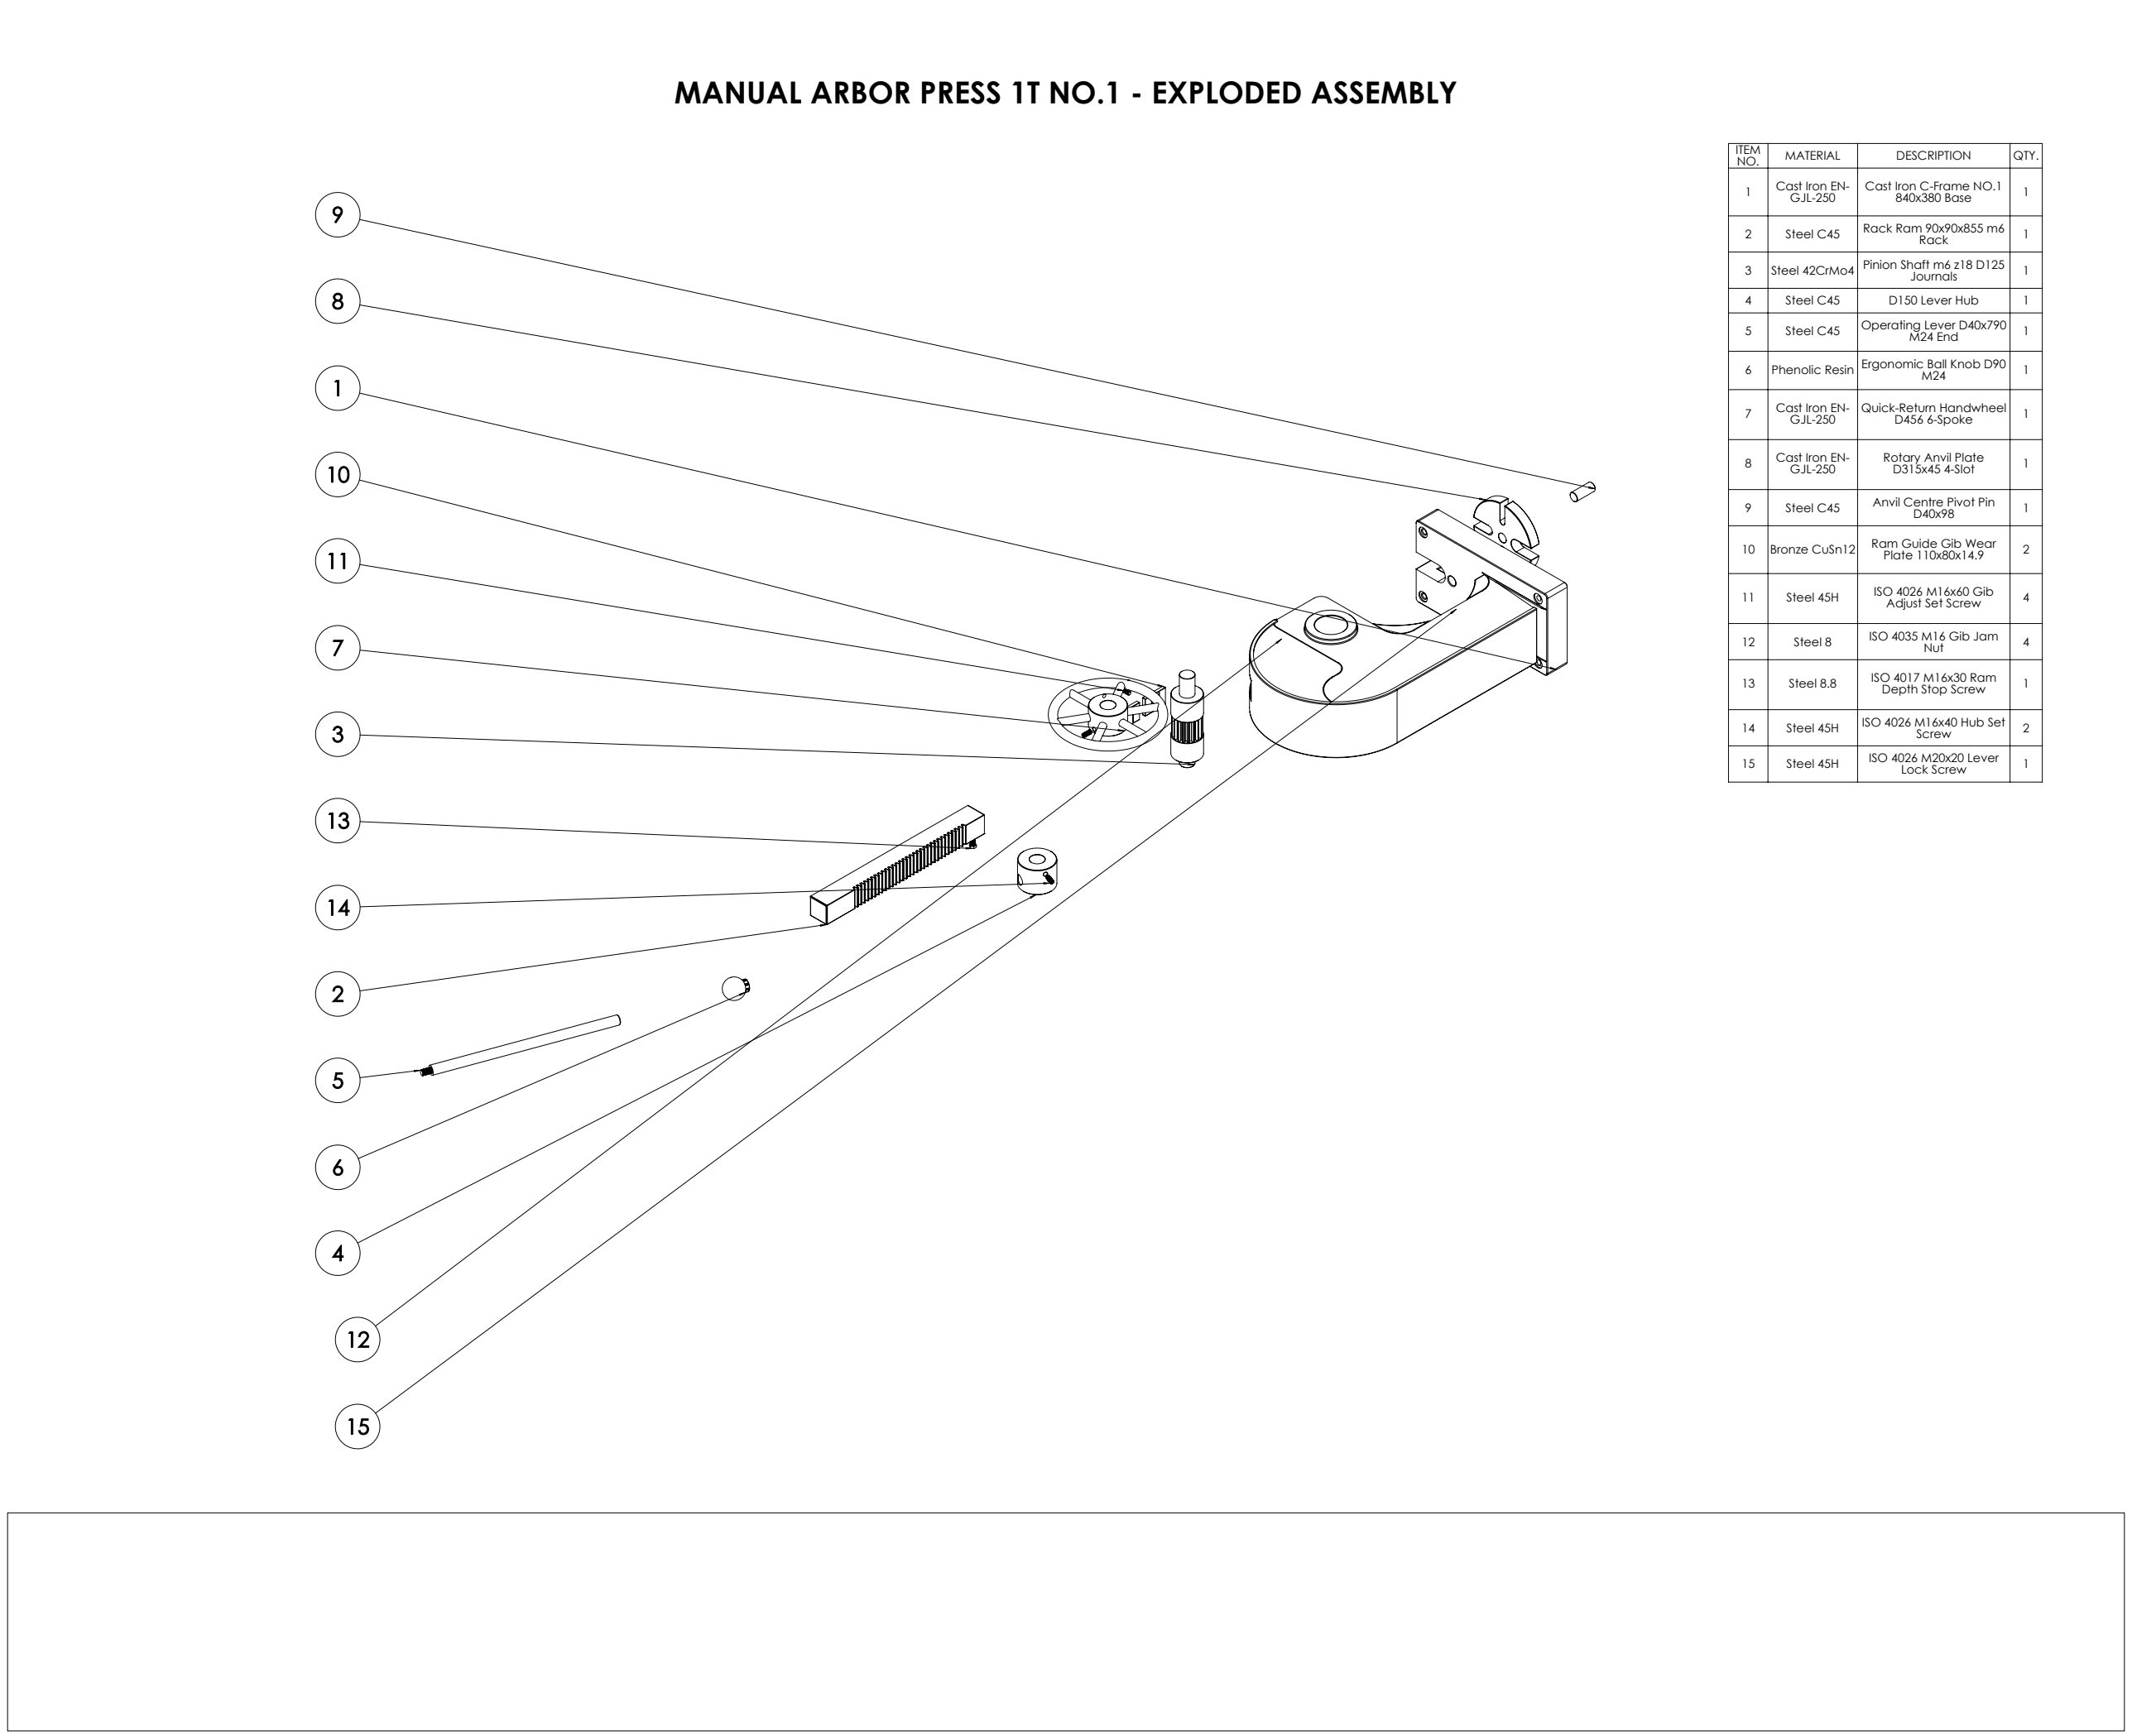
ISO-10303-21;
HEADER;
/* Generated by software containing ST-Developer
 * from STEP Tools, Inc. (www.steptools.com) 
 */

FILE_DESCRIPTION(
/* description */ (''),
/* implementation_level */ '2;1');

FILE_NAME(
/* name */ 'MAS-305',
/* time_stamp */ '2026-10-19T23:58:09-07:00',
/* author */ (''),
/* organization */ (''),
/* preprocessor_version */ 'ST-DEVELOPER v20.2',
/* originating_system */ 'Autodesk Translation Framework v15.15.0.0',
/* authorisation */ '');

FILE_SCHEMA (('AP203_CONFIGURATION_CONTROLLED_3D_DESIGN_OF_MECHANICAL_PARTS_AND_ASSEMBLIES_MIM_LF { 1 0 10303 203 3 1 4 }',
'AUTOMOTIVE_DESIGN { 1 0 10303 214 3 1 1 }','INTEGRATED_CNC_SCHEMA','MODEL_BASED_INTEGRATED_MANUFACTURING_SCHEMA',
'PROCESS_PLANNING_SCHEMA','AP242_MANAGED_MODEL_BASED_3D_ENGINEERING_MIM_LF { 1 0 10303 442 3 1 4 }'));
ENDSEC;

DATA;
#10=MECHANICAL_DESIGN_GEOMETRIC_PRESENTATION_REPRESENTATION('',(#407,#408,
#409,#410,#411,#412,#413,#414,#415,#416,#417,#418,#419,#420,#421,#422,#423,
#424,#425,#426,#427,#428,#429,#430,#431,#432,#433,#434,#435,#436,#437,#438,
#439,#440,#441,#442,#443,#444,#445,#446,#447,#448,#449,#450,#451,#452,#453,
#454,#455,#456,#457,#458,#459,#460,#461,#462,#463,#464,#465,#466),#70757);
#11=ITEM_DEFINED_TRANSFORMATION($,$,#27054,#28962);
#12=ITEM_DEFINED_TRANSFORMATION($,$,#27231,#28963);
#13=ITEM_DEFINED_TRANSFORMATION($,$,#27283,#28964);
#14=ITEM_DEFINED_TRANSFORMATION($,$,#27389,#28965);
#15=ITEM_DEFINED_TRANSFORMATION($,$,#27510,#28966);
#16=ITEM_DEFINED_TRANSFORMATION($,$,#27399,#28967);
#17=ITEM_DEFINED_TRANSFORMATION($,$,#27547,#28968);
#18=ITEM_DEFINED_TRANSFORMATION($,$,#27669,#28969);
#19=ITEM_DEFINED_TRANSFORMATION($,$,#27689,#28970);
#20=ITEM_DEFINED_TRANSFORMATION($,$,#27432,#28971);
#21=ITEM_DEFINED_TRANSFORMATION($,$,#27510,#28972);
#22=ITEM_DEFINED_TRANSFORMATION($,$,#27547,#28973);
#23=ITEM_DEFINED_TRANSFORMATION($,$,#27547,#28974);
#24=ITEM_DEFINED_TRANSFORMATION($,$,#27547,#28975);
#25=ITEM_DEFINED_TRANSFORMATION($,$,#27669,#28976);
#26=ITEM_DEFINED_TRANSFORMATION($,$,#27669,#28977);
#27=ITEM_DEFINED_TRANSFORMATION($,$,#27669,#28978);
#28=ITEM_DEFINED_TRANSFORMATION($,$,#27689,#28979);
#29=ITEM_DEFINED_TRANSFORMATION($,$,#27791,#28980);
#30=ITEM_DEFINED_TRANSFORMATION($,$,#27818,#28981);
#31=ITEM_DEFINED_TRANSFORMATION($,$,#28305,#28982);
#32=ITEM_DEFINED_TRANSFORMATION($,$,#28396,#28983);
#33=ITEM_DEFINED_TRANSFORMATION($,$,#28892,#28984);
#34=(
REPRESENTATION_RELATIONSHIP($,$,#70818,#70817)
REPRESENTATION_RELATIONSHIP_WITH_TRANSFORMATION(#11)
SHAPE_REPRESENTATION_RELATIONSHIP()
);
#35=(
REPRESENTATION_RELATIONSHIP($,$,#70819,#70817)
REPRESENTATION_RELATIONSHIP_WITH_TRANSFORMATION(#12)
SHAPE_REPRESENTATION_RELATIONSHIP()
);
#36=(
REPRESENTATION_RELATIONSHIP($,$,#70820,#70817)
REPRESENTATION_RELATIONSHIP_WITH_TRANSFORMATION(#13)
SHAPE_REPRESENTATION_RELATIONSHIP()
);
#37=(
REPRESENTATION_RELATIONSHIP($,$,#70821,#70817)
REPRESENTATION_RELATIONSHIP_WITH_TRANSFORMATION(#14)
SHAPE_REPRESENTATION_RELATIONSHIP()
);
#38=(
REPRESENTATION_RELATIONSHIP($,$,#70824,#70817)
REPRESENTATION_RELATIONSHIP_WITH_TRANSFORMATION(#15)
SHAPE_REPRESENTATION_RELATIONSHIP()
);
#39=(
REPRESENTATION_RELATIONSHIP($,$,#70822,#70817)
REPRESENTATION_RELATIONSHIP_WITH_TRANSFORMATION(#16)
SHAPE_REPRESENTATION_RELATIONSHIP()
);
#40=(
REPRESENTATION_RELATIONSHIP($,$,#70825,#70817)
REPRESENTATION_RELATIONSHIP_WITH_TRANSFORMATION(#17)
SHAPE_REPRESENTATION_RELATIONSHIP()
);
#41=(
REPRESENTATION_RELATIONSHIP($,$,#70826,#70817)
REPRESENTATION_RELATIONSHIP_WITH_TRANSFORMATION(#18)
SHAPE_REPRESENTATION_RELATIONSHIP()
);
#42=(
REPRESENTATION_RELATIONSHIP($,$,#70827,#70817)
REPRESENTATION_RELATIONSHIP_WITH_TRANSFORMATION(#19)
SHAPE_REPRESENTATION_RELATIONSHIP()
);
#43=(
REPRESENTATION_RELATIONSHIP($,$,#70823,#70817)
REPRESENTATION_RELATIONSHIP_WITH_TRANSFORMATION(#20)
SHAPE_REPRESENTATION_RELATIONSHIP()
);
#44=(
REPRESENTATION_RELATIONSHIP($,$,#70824,#70817)
REPRESENTATION_RELATIONSHIP_WITH_TRANSFORMATION(#21)
SHAPE_REPRESENTATION_RELATIONSHIP()
);
#45=(
REPRESENTATION_RELATIONSHIP($,$,#70825,#70817)
REPRESENTATION_RELATIONSHIP_WITH_TRANSFORMATION(#22)
SHAPE_REPRESENTATION_RELATIONSHIP()
);
#46=(
REPRESENTATION_RELATIONSHIP($,$,#70825,#70817)
REPRESENTATION_RELATIONSHIP_WITH_TRANSFORMATION(#23)
SHAPE_REPRESENTATION_RELATIONSHIP()
);
#47=(
REPRESENTATION_RELATIONSHIP($,$,#70825,#70817)
REPRESENTATION_RELATIONSHIP_WITH_TRANSFORMATION(#24)
SHAPE_REPRESENTATION_RELATIONSHIP()
);
#48=(
REPRESENTATION_RELATIONSHIP($,$,#70826,#70817)
REPRESENTATION_RELATIONSHIP_WITH_TRANSFORMATION(#25)
SHAPE_REPRESENTATION_RELATIONSHIP()
);
#49=(
REPRESENTATION_RELATIONSHIP($,$,#70826,#70817)
REPRESENTATION_RELATIONSHIP_WITH_TRANSFORMATION(#26)
SHAPE_REPRESENTATION_RELATIONSHIP()
);
#50=(
REPRESENTATION_RELATIONSHIP($,$,#70826,#70817)
REPRESENTATION_RELATIONSHIP_WITH_TRANSFORMATION(#27)
SHAPE_REPRESENTATION_RELATIONSHIP()
);
#51=(
REPRESENTATION_RELATIONSHIP($,$,#70827,#70817)
REPRESENTATION_RELATIONSHIP_WITH_TRANSFORMATION(#28)
SHAPE_REPRESENTATION_RELATIONSHIP()
);
#52=(
REPRESENTATION_RELATIONSHIP($,$,#70828,#70817)
REPRESENTATION_RELATIONSHIP_WITH_TRANSFORMATION(#29)
SHAPE_REPRESENTATION_RELATIONSHIP()
);
#53=(
REPRESENTATION_RELATIONSHIP($,$,#70829,#70817)
REPRESENTATION_RELATIONSHIP_WITH_TRANSFORMATION(#30)
SHAPE_REPRESENTATION_RELATIONSHIP()
);
#54=(
REPRESENTATION_RELATIONSHIP($,$,#70830,#70817)
REPRESENTATION_RELATIONSHIP_WITH_TRANSFORMATION(#31)
SHAPE_REPRESENTATION_RELATIONSHIP()
);
#55=(
REPRESENTATION_RELATIONSHIP($,$,#70831,#70817)
REPRESENTATION_RELATIONSHIP_WITH_TRANSFORMATION(#32)
SHAPE_REPRESENTATION_RELATIONSHIP()
);
#56=(
REPRESENTATION_RELATIONSHIP($,$,#70832,#70817)
REPRESENTATION_RELATIONSHIP_WITH_TRANSFORMATION(#33)
SHAPE_REPRESENTATION_RELATIONSHIP()
);
#57=CONTEXT_DEPENDENT_SHAPE_REPRESENTATION(#34,#70794);
#58=CONTEXT_DEPENDENT_SHAPE_REPRESENTATION(#35,#70795);
#59=CONTEXT_DEPENDENT_SHAPE_REPRESENTATION(#36,#70796);
#60=CONTEXT_DEPENDENT_SHAPE_REPRESENTATION(#37,#70797);
#61=CONTEXT_DEPENDENT_SHAPE_REPRESENTATION(#38,#70798);
#62=CONTEXT_DEPENDENT_SHAPE_REPRESENTATION(#39,#70799);
#63=CONTEXT_DEPENDENT_SHAPE_REPRESENTATION(#40,#70800);
#64=CONTEXT_DEPENDENT_SHAPE_REPRESENTATION(#41,#70801);
#65=CONTEXT_DEPENDENT_SHAPE_REPRESENTATION(#42,#70802);
#66=CONTEXT_DEPENDENT_SHAPE_REPRESENTATION(#43,#70803);
#67=CONTEXT_DEPENDENT_SHAPE_REPRESENTATION(#44,#70804);
#68=CONTEXT_DEPENDENT_SHAPE_REPRESENTATION(#45,#70805);
#69=CONTEXT_DEPENDENT_SHAPE_REPRESENTATION(#46,#70806);
#70=CONTEXT_DEPENDENT_SHAPE_REPRESENTATION(#47,#70807);
#71=CONTEXT_DEPENDENT_SHAPE_REPRESENTATION(#48,#70808);
#72=CONTEXT_DEPENDENT_SHAPE_REPRESENTATION(#49,#70809);
#73=CONTEXT_DEPENDENT_SHAPE_REPRESENTATION(#50,#70810);
#74=CONTEXT_DEPENDENT_SHAPE_REPRESENTATION(#51,#70811);
#75=CONTEXT_DEPENDENT_SHAPE_REPRESENTATION(#52,#70812);
#76=CONTEXT_DEPENDENT_SHAPE_REPRESENTATION(#53,#70813);
#77=CONTEXT_DEPENDENT_SHAPE_REPRESENTATION(#54,#70814);
#78=CONTEXT_DEPENDENT_SHAPE_REPRESENTATION(#55,#70815);
#79=CONTEXT_DEPENDENT_SHAPE_REPRESENTATION(#56,#70816);
#80=NEXT_ASSEMBLY_USAGE_OCCURRENCE(
'03_Pinion_Shaft_m6_z18_D125_Journals:1',
'03_Pinion_Shaft_m6_z18_D125_Journals:1',
'03_Pinion_Shaft_m6_z18_D125_Journals:1',#70834,#70835,
'03_Pinion_Shaft_m6_z18_D125_Journals:1');
#81=NEXT_ASSEMBLY_USAGE_OCCURRENCE(
'05_Operating_Lever_D40x790_M24_End:1',
'05_Operating_Lever_D40x790_M24_End:1',
'05_Operating_Lever_D40x790_M24_End:1',#70834,#70836,
'05_Operating_Lever_D40x790_M24_End:1');
#82=NEXT_ASSEMBLY_USAGE_OCCURRENCE(
'08_Rotary_Anvil_Plate_D315x45_4-Slot:1',
'08_Rotary_Anvil_Plate_D315x45_4-Slot:1',
'08_Rotary_Anvil_Plate_D315x45_4-Slot:1',#70834,#70837,
'08_Rotary_Anvil_Plate_D315x45_4-Slot:1');
#83=NEXT_ASSEMBLY_USAGE_OCCURRENCE('09_Anvil_Centre_Pivot_Pin_D40x98:1',
'09_Anvil_Centre_Pivot_Pin_D40x98:1',
'09_Anvil_Centre_Pivot_Pin_D40x98:1',#70834,#70838,
'09_Anvil_Centre_Pivot_Pin_D40x98:1');
#84=NEXT_ASSEMBLY_USAGE_OCCURRENCE(
'10_Ram_Guide_Gib_Wear_Plate_110x80x14.9:1',
'10_Ram_Guide_Gib_Wear_Plate_110x80x14.9:1',
'10_Ram_Guide_Gib_Wear_Plate_110x80x14.9:1',#70834,#70841,
'10_Ram_Guide_Gib_Wear_Plate_110x80x14.9:1');
#85=NEXT_ASSEMBLY_USAGE_OCCURRENCE(
'07_Quick-Return_Handwheel_D456_6-Spoke:1',
'07_Quick-Return_Handwheel_D456_6-Spoke:1',
'07_Quick-Return_Handwheel_D456_6-Spoke:1',#70834,#70839,
'07_Quick-Return_Handwheel_D456_6-Spoke:1');
#86=NEXT_ASSEMBLY_USAGE_OCCURRENCE(
'11_ISO_4026_M16x60_Gib_Adjust_Set_Screw:1',
'11_ISO_4026_M16x60_Gib_Adjust_Set_Screw:1',
'11_ISO_4026_M16x60_Gib_Adjust_Set_Screw:1',#70834,#70842,
'11_ISO_4026_M16x60_Gib_Adjust_Set_Screw:1');
#87=NEXT_ASSEMBLY_USAGE_OCCURRENCE('12_ISO_4035_M16_Gib_Jam_Nut:1',
'12_ISO_4035_M16_Gib_Jam_Nut:1','12_ISO_4035_M16_Gib_Jam_Nut:1',#70834,
#70843,'12_ISO_4035_M16_Gib_Jam_Nut:1');
#88=NEXT_ASSEMBLY_USAGE_OCCURRENCE('14_ISO_4026_M16x40_Hub_Set_Screw:1',
'14_ISO_4026_M16x40_Hub_Set_Screw:1',
'14_ISO_4026_M16x40_Hub_Set_Screw:1',#70834,#70844,
'14_ISO_4026_M16x40_Hub_Set_Screw:1');
#89=NEXT_ASSEMBLY_USAGE_OCCURRENCE(
'15_ISO_4026_M20x20_Lever_Lock_Screw:1',
'15_ISO_4026_M20x20_Lever_Lock_Screw:1',
'15_ISO_4026_M20x20_Lever_Lock_Screw:1',#70834,#70840,
'15_ISO_4026_M20x20_Lever_Lock_Screw:1');
#90=NEXT_ASSEMBLY_USAGE_OCCURRENCE(
'10_Ram_Guide_Gib_Wear_Plate_110x80x14.9:2',
'10_Ram_Guide_Gib_Wear_Plate_110x80x14.9:2',
'10_Ram_Guide_Gib_Wear_Plate_110x80x14.9:2',#70834,#70841,
'10_Ram_Guide_Gib_Wear_Plate_110x80x14.9:2');
#91=NEXT_ASSEMBLY_USAGE_OCCURRENCE(
'11_ISO_4026_M16x60_Gib_Adjust_Set_Screw:2',
'11_ISO_4026_M16x60_Gib_Adjust_Set_Screw:2',
'11_ISO_4026_M16x60_Gib_Adjust_Set_Screw:2',#70834,#70842,
'11_ISO_4026_M16x60_Gib_Adjust_Set_Screw:2');
#92=NEXT_ASSEMBLY_USAGE_OCCURRENCE(
'11_ISO_4026_M16x60_Gib_Adjust_Set_Screw:3',
'11_ISO_4026_M16x60_Gib_Adjust_Set_Screw:3',
'11_ISO_4026_M16x60_Gib_Adjust_Set_Screw:3',#70834,#70842,
'11_ISO_4026_M16x60_Gib_Adjust_Set_Screw:3');
#93=NEXT_ASSEMBLY_USAGE_OCCURRENCE(
'11_ISO_4026_M16x60_Gib_Adjust_Set_Screw:4',
'11_ISO_4026_M16x60_Gib_Adjust_Set_Screw:4',
'11_ISO_4026_M16x60_Gib_Adjust_Set_Screw:4',#70834,#70842,
'11_ISO_4026_M16x60_Gib_Adjust_Set_Screw:4');
#94=NEXT_ASSEMBLY_USAGE_OCCURRENCE('12_ISO_4035_M16_Gib_Jam_Nut:2',
'12_ISO_4035_M16_Gib_Jam_Nut:2','12_ISO_4035_M16_Gib_Jam_Nut:2',#70834,
#70843,'12_ISO_4035_M16_Gib_Jam_Nut:2');
#95=NEXT_ASSEMBLY_USAGE_OCCURRENCE('12_ISO_4035_M16_Gib_Jam_Nut:3',
'12_ISO_4035_M16_Gib_Jam_Nut:3','12_ISO_4035_M16_Gib_Jam_Nut:3',#70834,
#70843,'12_ISO_4035_M16_Gib_Jam_Nut:3');
#96=NEXT_ASSEMBLY_USAGE_OCCURRENCE('12_ISO_4035_M16_Gib_Jam_Nut:4',
'12_ISO_4035_M16_Gib_Jam_Nut:4','12_ISO_4035_M16_Gib_Jam_Nut:4',#70834,
#70843,'12_ISO_4035_M16_Gib_Jam_Nut:4');
#97=NEXT_ASSEMBLY_USAGE_OCCURRENCE('14_ISO_4026_M16x40_Hub_Set_Screw:2',
'14_ISO_4026_M16x40_Hub_Set_Screw:2',
'14_ISO_4026_M16x40_Hub_Set_Screw:2',#70834,#70844,
'14_ISO_4026_M16x40_Hub_Set_Screw:2');
#98=NEXT_ASSEMBLY_USAGE_OCCURRENCE('04_D150_Lever_Hub:1',
'04_D150_Lever_Hub:1','04_D150_Lever_Hub:1',#70834,#70845,
'04_D150_Lever_Hub:1');
#99=NEXT_ASSEMBLY_USAGE_OCCURRENCE('02_Rack_Ram_90x90x855_m6_Rack:1',
'02_Rack_Ram_90x90x855_m6_Rack:1','02_Rack_Ram_90x90x855_m6_Rack:1',#70834,
#70846,'02_Rack_Ram_90x90x855_m6_Rack:1');
#100=NEXT_ASSEMBLY_USAGE_OCCURRENCE('06_Ergonomic_Ball_Knob_D90_M24:1',
'06_Ergonomic_Ball_Knob_D90_M24:1','06_Ergonomic_Ball_Knob_D90_M24:1',#70834,
#70847,'06_Ergonomic_Ball_Knob_D90_M24:1');
#101=NEXT_ASSEMBLY_USAGE_OCCURRENCE(
'01_Cast_Iron_C-Frame_NO.1_840x380_Base:1',
'01_Cast_Iron_C-Frame_NO.1_840x380_Base:1',
'01_Cast_Iron_C-Frame_NO.1_840x380_Base:1',#70834,#70848,
'01_Cast_Iron_C-Frame_NO.1_840x380_Base:1');
#102=NEXT_ASSEMBLY_USAGE_OCCURRENCE(
'13_ISO_4017_M16x30_Ram_Depth_Stop_Screw:1',
'13_ISO_4017_M16x30_Ram_Depth_Stop_Screw:1',
'13_ISO_4017_M16x30_Ram_Depth_Stop_Screw:1',#70834,#70849,
'13_ISO_4017_M16x30_Ram_Depth_Stop_Screw:1');
#103=ELLIPSE('',#28418,0.424264068711927,0.3);
#104=ELLIPSE('',#28419,0.42426406871193,0.3);
#105=ELLIPSE('',#28420,0.424264068711931,0.3);
#106=ELLIPSE('',#28425,0.42426406871193,0.3);
#107=ELLIPSE('',#28426,0.424264068711927,0.3);
#108=ELLIPSE('',#28427,0.424264068711928,0.3);
#109=ELLIPSE('',#28431,0.42426406871193,0.3);
#110=ELLIPSE('',#28438,0.424264068711929,0.3);
#111=ELLIPSE('',#28443,0.424264068711926,0.3);
#112=ELLIPSE('',#28444,0.424264068711926,0.3);
#113=ELLIPSE('',#28447,0.424264068711929,0.3);
#114=ELLIPSE('',#28449,0.424264068711931,0.3);
#115=ELLIPSE('',#28458,0.424264068711927,0.3);
#116=ELLIPSE('',#28461,0.42426406871193,0.3);
#117=ELLIPSE('',#28597,5.65698522452918,4.00009261333671);
#118=ELLIPSE('',#28598,5.65698522452918,4.00009261333671);
#119=ELLIPSE('',#28641,0.424264068711926,0.3);
#120=ELLIPSE('',#28642,0.424264068711926,0.3);
#121=ELLIPSE('',#28652,0.424264068711926,0.3);
#122=ELLIPSE('',#28653,0.424264068711926,0.3);
#123=ELLIPSE('',#28709,5.65698522452937,4.00009261333671);
#124=ELLIPSE('',#28711,5.65698522452937,4.00009261333671);
#125=ELLIPSE('',#28723,11.3137084989848,8.);
#126=ELLIPSE('',#28726,11.3137084989848,8.);
#127=ELLIPSE('',#28730,2.63010371137609,2.21164478264163);
#128=ELLIPSE('',#28733,2.63010371137609,2.21164478264163);
#129=ELLIPSE('',#28734,6.83962146739207,5.75141317362232);
#130=ELLIPSE('',#28736,3.53553390593276,2.5);
#131=ELLIPSE('',#28768,11.3130048280025,7.99950242947666);
#132=ELLIPSE('',#28770,11.3130048280025,7.99950242947666);
#133=ELLIPSE('',#28840,6.83962146739207,5.75141317362232);
#134=ELLIPSE('',#28854,3.53553390593276,2.5);
#135=SPHERICAL_SURFACE('',#28394,4.5);
#136=SPHERICAL_SURFACE('',#28433,0.3);
#137=SPHERICAL_SURFACE('',#28439,0.300000000000001);
#138=SPHERICAL_SURFACE('',#28506,0.300000000000004);
#139=SPHERICAL_SURFACE('',#28510,0.299999999999997);
#140=SPHERICAL_SURFACE('',#28532,0.3);
#141=SPHERICAL_SURFACE('',#28555,0.3);
#142=TOROIDAL_SURFACE('',#27407,21.,1.8);
#143=TOROIDAL_SURFACE('',#28397,6.555,0.3);
#144=TOROIDAL_SURFACE('',#28407,6.555,0.3);
#145=TOROIDAL_SURFACE('',#28452,4.3,0.3);
#146=TOROIDAL_SURFACE('',#28476,1.4,0.3);
#147=TOROIDAL_SURFACE('',#28484,1.4,0.3);
#148=TOROIDAL_SURFACE('',#28486,1.4,0.3);
#149=TOROIDAL_SURFACE('',#28494,1.4,0.3);
#150=TOROIDAL_SURFACE('',#28496,1.4,0.3);
#151=TOROIDAL_SURFACE('',#28501,1.4,0.3);
#152=TOROIDAL_SURFACE('',#28516,30.9296013460341,0.3);
#153=TOROIDAL_SURFACE('',#28519,30.9296013460341,0.3);
#154=TOROIDAL_SURFACE('',#28541,32.7,0.3);
#155=TOROIDAL_SURFACE('',#28557,32.7,0.3);
#156=TOROIDAL_SURFACE('',#28568,1.10499999999999,0.3);
#157=TOROIDAL_SURFACE('',#28580,1.10499999999999,0.3);
#158=TOROIDAL_SURFACE('',#28586,1.10499999999999,0.3);
#159=TOROIDAL_SURFACE('',#28592,1.10499999999999,0.3);
#160=TOROIDAL_SURFACE('',#28609,2.3,0.3);
#161=TOROIDAL_SURFACE('',#28615,30.9296013460341,0.3);
#162=TOROIDAL_SURFACE('',#28621,30.9296013460341,0.3);
#163=TOROIDAL_SURFACE('',#28626,2.3,0.3);
#164=TOROIDAL_SURFACE('',#28643,1.10499999999999,0.3);
#165=TOROIDAL_SURFACE('',#28645,1.10499999999999,0.3);
#166=TOROIDAL_SURFACE('',#28647,1.10499999999999,0.3);
#167=TOROIDAL_SURFACE('',#28649,1.10499999999999,0.3);
#168=TOROIDAL_SURFACE('',#28661,32.7,0.3);
#169=TOROIDAL_SURFACE('',#28665,32.7,0.3);
#170=TOROIDAL_SURFACE('',#28944,0.8511,0.06);
#171=(
BOUNDED_CURVE()
B_SPLINE_CURVE(2,(#43625,#43626,#43627),.UNSPECIFIED.,.F.,.F.)
B_SPLINE_CURVE_WITH_KNOTS((3,3),(0.00762589341662222,0.217939135937014),
 .UNSPECIFIED.)
CURVE()
GEOMETRIC_REPRESENTATION_ITEM()
RATIONAL_B_SPLINE_CURVE((1.00000105618797,1.00001509230994,1.))
REPRESENTATION_ITEM('')
);
#172=(
BOUNDED_CURVE()
B_SPLINE_CURVE(2,(#43631,#43632,#43633),.UNSPECIFIED.,.F.,.F.)
B_SPLINE_CURVE_WITH_KNOTS((3,3),(0.,0.167475634560782),.UNSPECIFIED.)
CURVE()
GEOMETRIC_REPRESENTATION_ITEM()
RATIONAL_B_SPLINE_CURVE((1.,1.00001872457605,1.00001886903166))
REPRESENTATION_ITEM('')
);
#173=(
BOUNDED_CURVE()
B_SPLINE_CURVE(2,(#43647,#43648,#43649),.UNSPECIFIED.,.F.,.F.)
B_SPLINE_CURVE_WITH_KNOTS((3,3),(0.137287012047938,0.14598329580768),
 .UNSPECIFIED.)
CURVE()
GEOMETRIC_REPRESENTATION_ITEM()
RATIONAL_B_SPLINE_CURVE((1.,1.,1.))
REPRESENTATION_ITEM('')
);
#174=(
BOUNDED_CURVE()
B_SPLINE_CURVE(2,(#43653,#43654,#43655),.UNSPECIFIED.,.F.,.F.)
B_SPLINE_CURVE_WITH_KNOTS((3,3),(7.75867498909367,7.76962220124035),
 .UNSPECIFIED.)
CURVE()
GEOMETRIC_REPRESENTATION_ITEM()
RATIONAL_B_SPLINE_CURVE((1.,1.,1.))
REPRESENTATION_ITEM('')
);
#175=(
BOUNDED_CURVE()
B_SPLINE_CURVE(2,(#43656,#43657,#43658),.UNSPECIFIED.,.F.,.F.)
B_SPLINE_CURVE_WITH_KNOTS((3,3),(0.,0.20316916463777),.UNSPECIFIED.)
CURVE()
GEOMETRIC_REPRESENTATION_ITEM()
RATIONAL_B_SPLINE_CURVE((1.,1.00001376388279,1.00000116347276))
REPRESENTATION_ITEM('')
);
#176=(
BOUNDED_CURVE()
B_SPLINE_CURVE(2,(#43673,#43674,#43675),.UNSPECIFIED.,.F.,.F.)
B_SPLINE_CURVE_WITH_KNOTS((3,3),(0.170079793729576,0.3375554282914),
 .UNSPECIFIED.)
CURVE()
GEOMETRIC_REPRESENTATION_ITEM()
RATIONAL_B_SPLINE_CURVE((1.00001886905196,1.00001872459619,1.))
REPRESENTATION_ITEM('')
);
#177=(
BOUNDED_CURVE()
B_SPLINE_CURVE(2,(#43679,#43680,#43681),.UNSPECIFIED.,.F.,.F.)
B_SPLINE_CURVE_WITH_KNOTS((3,3),(0.,0.210313242519936),.UNSPECIFIED.)
CURVE()
GEOMETRIC_REPRESENTATION_ITEM()
RATIONAL_B_SPLINE_CURVE((1.,1.00001509226017,1.00000105618449))
REPRESENTATION_ITEM('')
);
#178=(
BOUNDED_CURVE()
B_SPLINE_CURVE(2,(#43694,#43695,#43696),.UNSPECIFIED.,.F.,.F.)
B_SPLINE_CURVE_WITH_KNOTS((3,3),(0.,0.17930472101048),.UNSPECIFIED.)
CURVE()
GEOMETRIC_REPRESENTATION_ITEM()
RATIONAL_B_SPLINE_CURVE((1.,1.,1.))
REPRESENTATION_ITEM('')
);
#179=(
BOUNDED_CURVE()
B_SPLINE_CURVE(2,(#43703,#43704,#43705),.UNSPECIFIED.,.F.,.F.)
B_SPLINE_CURVE_WITH_KNOTS((3,3),(7.54305180428147,7.55174808804129),
 .UNSPECIFIED.)
CURVE()
GEOMETRIC_REPRESENTATION_ITEM()
RATIONAL_B_SPLINE_CURVE((1.,1.,1.))
REPRESENTATION_ITEM('')
);
#180=(
BOUNDED_CURVE()
B_SPLINE_CURVE(2,(#43722,#43723,#43724),.UNSPECIFIED.,.F.,.F.)
B_SPLINE_CURVE_WITH_KNOTS((3,3),(0.177416517606212,0.356721238616782),
 .UNSPECIFIED.)
CURVE()
GEOMETRIC_REPRESENTATION_ITEM()
RATIONAL_B_SPLINE_CURVE((1.,1.,1.))
REPRESENTATION_ITEM('')
);
#181=(
BOUNDED_CURVE()
B_SPLINE_CURVE(2,(#43757,#43758,#43759),.UNSPECIFIED.,.F.,.F.)
B_SPLINE_CURVE_WITH_KNOTS((3,3),(0.166982558562854,0.32848249154248),
 .UNSPECIFIED.)
CURVE()
GEOMETRIC_REPRESENTATION_ITEM()
RATIONAL_B_SPLINE_CURVE((1.00001732315097,1.00001703876093,1.))
REPRESENTATION_ITEM('')
);
#182=(
BOUNDED_CURVE()
B_SPLINE_CURVE(2,(#43760,#43761,#43762),.UNSPECIFIED.,.F.,.F.)
B_SPLINE_CURVE_WITH_KNOTS((3,3),(0.,0.188171618307079),.UNSPECIFIED.)
CURVE()
GEOMETRIC_REPRESENTATION_ITEM()
RATIONAL_B_SPLINE_CURVE((1.,1.,1.))
REPRESENTATION_ITEM('')
);
#183=(
BOUNDED_CURVE()
B_SPLINE_CURVE(2,(#43766,#43767,#43768),.UNSPECIFIED.,.F.,.F.)
B_SPLINE_CURVE_WITH_KNOTS((3,3),(0.00896598248719952,0.212135147124771),
 .UNSPECIFIED.)
CURVE()
GEOMETRIC_REPRESENTATION_ITEM()
RATIONAL_B_SPLINE_CURVE((1.00000116347024,1.00001376385308,1.))
REPRESENTATION_ITEM('')
);
#184=(
BOUNDED_CURVE()
B_SPLINE_CURVE(2,(#43772,#43773,#43774),.UNSPECIFIED.,.F.,.F.)
B_SPLINE_CURVE_WITH_KNOTS((3,3),(0.,0.161499932979635),.UNSPECIFIED.)
CURVE()
GEOMETRIC_REPRESENTATION_ITEM()
RATIONAL_B_SPLINE_CURVE((1.,1.00001703876093,1.00001732315097))
REPRESENTATION_ITEM('')
);
#185=(
BOUNDED_CURVE()
B_SPLINE_CURVE(2,(#43792,#43793,#43794),.UNSPECIFIED.,.F.,.F.)
B_SPLINE_CURVE_WITH_KNOTS((3,3),(0.143033593949376,0.153980806095915),
 .UNSPECIFIED.)
CURVE()
GEOMETRIC_REPRESENTATION_ITEM()
RATIONAL_B_SPLINE_CURVE((1.,1.,1.))
REPRESENTATION_ITEM('')
);
#186=(
BOUNDED_CURVE()
B_SPLINE_CURVE(2,(#43800,#43801,#43802),.UNSPECIFIED.,.F.,.F.)
B_SPLINE_CURVE_WITH_KNOTS((3,3),(0.18255185197649,0.370723470283569),
 .UNSPECIFIED.)
CURVE()
GEOMETRIC_REPRESENTATION_ITEM()
RATIONAL_B_SPLINE_CURVE((1.,1.,1.))
REPRESENTATION_ITEM('')
);
#187=(
BOUNDED_CURVE()
B_SPLINE_CURVE(2,(#43820,#43821,#43822),.UNSPECIFIED.,.F.,.F.)
B_SPLINE_CURVE_WITH_KNOTS((3,3),(0.166073953914202,0.324403911055146),
 .UNSPECIFIED.)
CURVE()
GEOMETRIC_REPRESENTATION_ITEM()
RATIONAL_B_SPLINE_CURVE((1.00001663891698,1.00001625098222,1.))
REPRESENTATION_ITEM('')
);
#188=(
BOUNDED_CURVE()
B_SPLINE_CURVE(2,(#43823,#43824,#43825),.UNSPECIFIED.,.F.,.F.)
B_SPLINE_CURVE_WITH_KNOTS((3,3),(0.,0.193708051007078),.UNSPECIFIED.)
CURVE()
GEOMETRIC_REPRESENTATION_ITEM()
RATIONAL_B_SPLINE_CURVE((1.,1.,1.))
REPRESENTATION_ITEM('')
);
#189=(
BOUNDED_CURVE()
B_SPLINE_CURVE(2,(#43843,#43844,#43845),.UNSPECIFIED.,.F.,.F.)
B_SPLINE_CURVE_WITH_KNOTS((3,3),(0.00815575297236999,0.214933042676883),
 .UNSPECIFIED.)
CURVE()
GEOMETRIC_REPRESENTATION_ITEM()
RATIONAL_B_SPLINE_CURVE((1.00000109358995,1.00001440998863,1.))
REPRESENTATION_ITEM('')
);
#190=(
BOUNDED_CURVE()
B_SPLINE_CURVE(2,(#43849,#43850,#43851),.UNSPECIFIED.,.F.,.F.)
B_SPLINE_CURVE_WITH_KNOTS((3,3),(0.,0.164543974719834),.UNSPECIFIED.)
CURVE()
GEOMETRIC_REPRESENTATION_ITEM()
RATIONAL_B_SPLINE_CURVE((1.,1.00001786148183,1.00001806362432))
REPRESENTATION_ITEM('')
);
#191=(
BOUNDED_CURVE()
B_SPLINE_CURVE(2,(#43869,#43870,#43871),.UNSPECIFIED.,.F.,.F.)
B_SPLINE_CURVE_WITH_KNOTS((3,3),(0.140031413282733,0.149652192224334),
 .UNSPECIFIED.)
CURVE()
GEOMETRIC_REPRESENTATION_ITEM()
RATIONAL_B_SPLINE_CURVE((1.,1.,1.))
REPRESENTATION_ITEM('')
);
#192=(
BOUNDED_CURVE()
B_SPLINE_CURVE(2,(#43877,#43878,#43879),.UNSPECIFIED.,.F.,.F.)
B_SPLINE_CURVE_WITH_KNOTS((3,3),(0.180004690478429,0.363403446267975),
 .UNSPECIFIED.)
CURVE()
GEOMETRIC_REPRESENTATION_ITEM()
RATIONAL_B_SPLINE_CURVE((1.,1.,1.))
REPRESENTATION_ITEM('')
);
#193=(
BOUNDED_CURVE()
B_SPLINE_CURVE(2,(#43884,#43885,#43886),.UNSPECIFIED.,.F.,.F.)
B_SPLINE_CURVE_WITH_KNOTS((3,3),(0.168310970500792,0.332854945221182),
 .UNSPECIFIED.)
CURVE()
GEOMETRIC_REPRESENTATION_ITEM()
RATIONAL_B_SPLINE_CURVE((1.00001806363053,1.00001786148798,1.))
REPRESENTATION_ITEM('')
);
#194=(
BOUNDED_CURVE()
B_SPLINE_CURVE(2,(#43890,#43891,#43892),.UNSPECIFIED.,.F.,.F.)
B_SPLINE_CURVE_WITH_KNOTS((3,3),(0.,0.206777289704965),.UNSPECIFIED.)
CURVE()
GEOMETRIC_REPRESENTATION_ITEM()
RATIONAL_B_SPLINE_CURVE((1.,1.00001441002009,1.00000109359234))
REPRESENTATION_ITEM('')
);
#195=(
BOUNDED_CURVE()
B_SPLINE_CURVE(2,(#43905,#43906,#43907),.UNSPECIFIED.,.F.,.F.)
B_SPLINE_CURVE_WITH_KNOTS((3,3),(0.,0.183398755789119),.UNSPECIFIED.)
CURVE()
GEOMETRIC_REPRESENTATION_ITEM()
RATIONAL_B_SPLINE_CURVE((1.,1.,1.))
REPRESENTATION_ITEM('')
);
#196=(
BOUNDED_CURVE()
B_SPLINE_CURVE(2,(#43909,#43910,#43911),.UNSPECIFIED.,.F.,.F.)
B_SPLINE_CURVE_WITH_KNOTS((3,3),(0.185074227573043,0.378782278580072),
 .UNSPECIFIED.)
CURVE()
GEOMETRIC_REPRESENTATION_ITEM()
RATIONAL_B_SPLINE_CURVE((1.,1.,1.))
REPRESENTATION_ITEM('')
);
#197=(
BOUNDED_CURVE()
B_SPLINE_CURVE(2,(#43912,#43913,#43914),.UNSPECIFIED.,.F.,.F.)
B_SPLINE_CURVE_WITH_KNOTS((3,3),(0.,0.158329957141101),.UNSPECIFIED.)
CURVE()
GEOMETRIC_REPRESENTATION_ITEM()
RATIONAL_B_SPLINE_CURVE((1.,1.00001625097861,1.00001663891328))
REPRESENTATION_ITEM('')
);
#198=(
BOUNDED_CURVE()
B_SPLINE_CURVE(2,(#43929,#43930,#43931),.UNSPECIFIED.,.F.,.F.)
B_SPLINE_CURVE_WITH_KNOTS((3,3),(0.0100528190707853,0.209523932952566),
 .UNSPECIFIED.)
CURVE()
GEOMETRIC_REPRESENTATION_ITEM()
RATIONAL_B_SPLINE_CURVE((1.00000126177961,1.00001314919847,1.))
REPRESENTATION_ITEM('')
);
#199=(
BOUNDED_CURVE()
B_SPLINE_CURVE(2,(#43949,#43950,#43951),.UNSPECIFIED.,.F.,.F.)
B_SPLINE_CURVE_WITH_KNOTS((3,3),(0.146334104657409,0.159049105721225),
 .UNSPECIFIED.)
CURVE()
GEOMETRIC_REPRESENTATION_ITEM()
RATIONAL_B_SPLINE_CURVE((1.,1.,1.))
REPRESENTATION_ITEM('')
);
#200=(
BOUNDED_CURVE()
B_SPLINE_CURVE(2,(#43962,#43963,#43964),.UNSPECIFIED.,.F.,.F.)
B_SPLINE_CURVE_WITH_KNOTS((3,3),(0.,0.199471113881606),.UNSPECIFIED.)
CURVE()
GEOMETRIC_REPRESENTATION_ITEM()
RATIONAL_B_SPLINE_CURVE((1.,1.00001314920547,1.00000126178028))
REPRESENTATION_ITEM('')
);
#201=(
BOUNDED_CURVE()
B_SPLINE_CURVE(2,(#44023,#44024,#44025),.UNSPECIFIED.,.F.,.F.)
B_SPLINE_CURVE_WITH_KNOTS((3,3),(7.87870547859755,7.89142047966152),
 .UNSPECIFIED.)
CURVE()
GEOMETRIC_REPRESENTATION_ITEM()
RATIONAL_B_SPLINE_CURVE((1.,1.,1.))
REPRESENTATION_ITEM('')
);
#202=(
BOUNDED_CURVE()
B_SPLINE_CURVE(2,(#44035,#44036,#44037),.UNSPECIFIED.,.F.,.F.)
B_SPLINE_CURVE_WITH_KNOTS((3,3),(7.6471088967316,7.6567296756733),
 .UNSPECIFIED.)
CURVE()
GEOMETRIC_REPRESENTATION_ITEM()
RATIONAL_B_SPLINE_CURVE((1.,1.,1.))
REPRESENTATION_ITEM('')
);
#203=(
BOUNDED_CURVE()
B_SPLINE_CURVE(2,(#47308,#47309,#47310),.UNSPECIFIED.,.F.,.F.)
B_SPLINE_CURVE_WITH_KNOTS((3,3),(0.,0.00348481894602421),.UNSPECIFIED.)
CURVE()
GEOMETRIC_REPRESENTATION_ITEM()
RATIONAL_B_SPLINE_CURVE((1.,1.00000419109631,1.))
REPRESENTATION_ITEM('')
);
#204=(
BOUNDED_CURVE()
B_SPLINE_CURVE(2,(#47312,#47313,#47314),.UNSPECIFIED.,.F.,.F.)
B_SPLINE_CURVE_WITH_KNOTS((3,3),(0.,0.0034848189460241),.UNSPECIFIED.)
CURVE()
GEOMETRIC_REPRESENTATION_ITEM()
RATIONAL_B_SPLINE_CURVE((1.,1.00000419078036,1.))
REPRESENTATION_ITEM('')
);
#205=(
BOUNDED_CURVE()
B_SPLINE_CURVE(2,(#47317,#47318,#47319),.UNSPECIFIED.,.F.,.F.)
B_SPLINE_CURVE_WITH_KNOTS((3,3),(0.,0.00348481894602397),.UNSPECIFIED.)
CURVE()
GEOMETRIC_REPRESENTATION_ITEM()
RATIONAL_B_SPLINE_CURVE((1.,1.00000419109938,1.))
REPRESENTATION_ITEM('')
);
#206=(
BOUNDED_CURVE()
B_SPLINE_CURVE(2,(#47321,#47322,#47323),.UNSPECIFIED.,.F.,.F.)
B_SPLINE_CURVE_WITH_KNOTS((3,3),(0.,0.00348481894602389),.UNSPECIFIED.)
CURVE()
GEOMETRIC_REPRESENTATION_ITEM()
RATIONAL_B_SPLINE_CURVE((1.,1.0000041910806,1.))
REPRESENTATION_ITEM('')
);
#207=(
BOUNDED_CURVE()
B_SPLINE_CURVE(2,(#47326,#47327,#47328),.UNSPECIFIED.,.F.,.F.)
B_SPLINE_CURVE_WITH_KNOTS((3,3),(0.,0.003484818946024),.UNSPECIFIED.)
CURVE()
GEOMETRIC_REPRESENTATION_ITEM()
RATIONAL_B_SPLINE_CURVE((1.,1.00000419096159,1.))
REPRESENTATION_ITEM('')
);
#208=(
BOUNDED_CURVE()
B_SPLINE_CURVE(2,(#47330,#47331,#47332),.UNSPECIFIED.,.F.,.F.)
B_SPLINE_CURVE_WITH_KNOTS((3,3),(0.,0.00348481894602396),.UNSPECIFIED.)
CURVE()
GEOMETRIC_REPRESENTATION_ITEM()
RATIONAL_B_SPLINE_CURVE((1.,1.00000419112827,1.))
REPRESENTATION_ITEM('')
);
#209=(
BOUNDED_CURVE()
B_SPLINE_CURVE(2,(#47335,#47336,#47337),.UNSPECIFIED.,.F.,.F.)
B_SPLINE_CURVE_WITH_KNOTS((3,3),(0.,0.00348481894602387),.UNSPECIFIED.)
CURVE()
GEOMETRIC_REPRESENTATION_ITEM()
RATIONAL_B_SPLINE_CURVE((1.,1.00000419105483,1.))
REPRESENTATION_ITEM('')
);
#210=(
BOUNDED_CURVE()
B_SPLINE_CURVE(2,(#47339,#47340,#47341),.UNSPECIFIED.,.F.,.F.)
B_SPLINE_CURVE_WITH_KNOTS((3,3),(0.,0.00348481894602378),.UNSPECIFIED.)
CURVE()
GEOMETRIC_REPRESENTATION_ITEM()
RATIONAL_B_SPLINE_CURVE((1.,1.00000419099658,1.))
REPRESENTATION_ITEM('')
);
#211=(
BOUNDED_CURVE()
B_SPLINE_CURVE(2,(#47344,#47345,#47346),.UNSPECIFIED.,.F.,.F.)
B_SPLINE_CURVE_WITH_KNOTS((3,3),(0.,0.00348481894602419),.UNSPECIFIED.)
CURVE()
GEOMETRIC_REPRESENTATION_ITEM()
RATIONAL_B_SPLINE_CURVE((1.,1.00000419117121,1.))
REPRESENTATION_ITEM('')
);
#212=(
BOUNDED_CURVE()
B_SPLINE_CURVE(2,(#47348,#47349,#47350),.UNSPECIFIED.,.F.,.F.)
B_SPLINE_CURVE_WITH_KNOTS((3,3),(0.,0.00348481894602411),.UNSPECIFIED.)
CURVE()
GEOMETRIC_REPRESENTATION_ITEM()
RATIONAL_B_SPLINE_CURVE((1.,1.00000419088834,1.))
REPRESENTATION_ITEM('')
);
#213=(
BOUNDED_CURVE()
B_SPLINE_CURVE(2,(#47353,#47354,#47355),.UNSPECIFIED.,.F.,.F.)
B_SPLINE_CURVE_WITH_KNOTS((3,3),(0.,0.00348481894602378),.UNSPECIFIED.)
CURVE()
GEOMETRIC_REPRESENTATION_ITEM()
RATIONAL_B_SPLINE_CURVE((1.,1.00000419109063,1.))
REPRESENTATION_ITEM('')
);
#214=(
BOUNDED_CURVE()
B_SPLINE_CURVE(2,(#47357,#47358,#47359),.UNSPECIFIED.,.F.,.F.)
B_SPLINE_CURVE_WITH_KNOTS((3,3),(0.,0.00348481894602365),.UNSPECIFIED.)
CURVE()
GEOMETRIC_REPRESENTATION_ITEM()
RATIONAL_B_SPLINE_CURVE((1.,1.00000419111732,1.))
REPRESENTATION_ITEM('')
);
#215=(
BOUNDED_CURVE()
B_SPLINE_CURVE(2,(#54486,#54487,#54488),.UNSPECIFIED.,.F.,.F.)
B_SPLINE_CURVE_WITH_KNOTS((3,3),(0.,0.00348603246849772),.UNSPECIFIED.)
CURVE()
GEOMETRIC_REPRESENTATION_ITEM()
RATIONAL_B_SPLINE_CURVE((1.,1.00000655818292,1.))
REPRESENTATION_ITEM('')
);
#216=(
BOUNDED_CURVE()
B_SPLINE_CURVE(2,(#54490,#54491,#54492),.UNSPECIFIED.,.F.,.F.)
B_SPLINE_CURVE_WITH_KNOTS((3,3),(0.,0.0034860324684977),.UNSPECIFIED.)
CURVE()
GEOMETRIC_REPRESENTATION_ITEM()
RATIONAL_B_SPLINE_CURVE((1.,1.00000655824651,1.))
REPRESENTATION_ITEM('')
);
#217=(
BOUNDED_CURVE()
B_SPLINE_CURVE(2,(#54495,#54496,#54497),.UNSPECIFIED.,.F.,.F.)
B_SPLINE_CURVE_WITH_KNOTS((3,3),(0.,0.00348603246849777),.UNSPECIFIED.)
CURVE()
GEOMETRIC_REPRESENTATION_ITEM()
RATIONAL_B_SPLINE_CURVE((1.,1.00000655828125,1.))
REPRESENTATION_ITEM('')
);
#218=(
BOUNDED_CURVE()
B_SPLINE_CURVE(2,(#54499,#54500,#54501),.UNSPECIFIED.,.F.,.F.)
B_SPLINE_CURVE_WITH_KNOTS((3,3),(0.,0.00348603246849785),.UNSPECIFIED.)
CURVE()
GEOMETRIC_REPRESENTATION_ITEM()
RATIONAL_B_SPLINE_CURVE((1.,1.00000655858972,1.))
REPRESENTATION_ITEM('')
);
#219=(
BOUNDED_CURVE()
B_SPLINE_CURVE(2,(#54504,#54505,#54506),.UNSPECIFIED.,.F.,.F.)
B_SPLINE_CURVE_WITH_KNOTS((3,3),(0.,0.00348603246849743),.UNSPECIFIED.)
CURVE()
GEOMETRIC_REPRESENTATION_ITEM()
RATIONAL_B_SPLINE_CURVE((1.,1.00000655826316,1.))
REPRESENTATION_ITEM('')
);
#220=(
BOUNDED_CURVE()
B_SPLINE_CURVE(2,(#54508,#54509,#54510),.UNSPECIFIED.,.F.,.F.)
B_SPLINE_CURVE_WITH_KNOTS((3,3),(0.,0.00348603246849747),.UNSPECIFIED.)
CURVE()
GEOMETRIC_REPRESENTATION_ITEM()
RATIONAL_B_SPLINE_CURVE((1.,1.00000655837246,1.))
REPRESENTATION_ITEM('')
);
#221=(
BOUNDED_CURVE()
B_SPLINE_CURVE(2,(#54513,#54514,#54515),.UNSPECIFIED.,.F.,.F.)
B_SPLINE_CURVE_WITH_KNOTS((3,3),(0.,0.00348603246849727),.UNSPECIFIED.)
CURVE()
GEOMETRIC_REPRESENTATION_ITEM()
RATIONAL_B_SPLINE_CURVE((1.,1.00000655774933,1.))
REPRESENTATION_ITEM('')
);
#222=(
BOUNDED_CURVE()
B_SPLINE_CURVE(2,(#54517,#54518,#54519),.UNSPECIFIED.,.F.,.F.)
B_SPLINE_CURVE_WITH_KNOTS((3,3),(0.,0.00348603246849747),.UNSPECIFIED.)
CURVE()
GEOMETRIC_REPRESENTATION_ITEM()
RATIONAL_B_SPLINE_CURVE((1.,1.00000655778188,1.))
REPRESENTATION_ITEM('')
);
#223=(
BOUNDED_CURVE()
B_SPLINE_CURVE(2,(#54522,#54523,#54524),.UNSPECIFIED.,.F.,.F.)
B_SPLINE_CURVE_WITH_KNOTS((3,3),(0.,0.00348603246849769),.UNSPECIFIED.)
CURVE()
GEOMETRIC_REPRESENTATION_ITEM()
RATIONAL_B_SPLINE_CURVE((1.,1.00000655825998,1.))
REPRESENTATION_ITEM('')
);
#224=(
BOUNDED_CURVE()
B_SPLINE_CURVE(2,(#54526,#54527,#54528),.UNSPECIFIED.,.F.,.F.)
B_SPLINE_CURVE_WITH_KNOTS((3,3),(0.,0.00348603246849761),.UNSPECIFIED.)
CURVE()
GEOMETRIC_REPRESENTATION_ITEM()
RATIONAL_B_SPLINE_CURVE((1.,1.00000655838487,1.))
REPRESENTATION_ITEM('')
);
#225=(
BOUNDED_CURVE()
B_SPLINE_CURVE(2,(#54531,#54532,#54533),.UNSPECIFIED.,.F.,.F.)
B_SPLINE_CURVE_WITH_KNOTS((3,3),(0.,0.00348603246849764),.UNSPECIFIED.)
CURVE()
GEOMETRIC_REPRESENTATION_ITEM()
RATIONAL_B_SPLINE_CURVE((1.,1.00000655822052,1.))
REPRESENTATION_ITEM('')
);
#226=(
BOUNDED_CURVE()
B_SPLINE_CURVE(2,(#54535,#54536,#54537),.UNSPECIFIED.,.F.,.F.)
B_SPLINE_CURVE_WITH_KNOTS((3,3),(0.,0.00348603246849749),.UNSPECIFIED.)
CURVE()
GEOMETRIC_REPRESENTATION_ITEM()
RATIONAL_B_SPLINE_CURVE((1.,1.00000655832735,1.))
REPRESENTATION_ITEM('')
);
#227=(
BOUNDED_CURVE()
B_SPLINE_CURVE(2,(#54642,#54643,#54644),.UNSPECIFIED.,.F.,.F.)
B_SPLINE_CURVE_WITH_KNOTS((3,3),(0.083069206448341,0.799733019594622),
 .UNSPECIFIED.)
CURVE()
GEOMETRIC_REPRESENTATION_ITEM()
RATIONAL_B_SPLINE_CURVE((1.01933756729741,1.09818360252296,1.09818360252296))
REPRESENTATION_ITEM('')
);
#228=(
BOUNDED_CURVE()
B_SPLINE_CURVE(2,(#54646,#54647,#54648),.UNSPECIFIED.,.F.,.F.)
B_SPLINE_CURVE_WITH_KNOTS((3,3),(0.0830692064483412,1.5163968327409),
 .UNSPECIFIED.)
CURVE()
GEOMETRIC_REPRESENTATION_ITEM()
RATIONAL_B_SPLINE_CURVE((1.01933756729741,1.17702963774851,1.01933756729741))
REPRESENTATION_ITEM('')
);
#229=(
BOUNDED_CURVE()
B_SPLINE_CURVE(2,(#54650,#54651,#54652),.UNSPECIFIED.,.F.,.F.)
B_SPLINE_CURVE_WITH_KNOTS((3,3),(0.0830692064483411,1.5163968327409),
 .UNSPECIFIED.)
CURVE()
GEOMETRIC_REPRESENTATION_ITEM()
RATIONAL_B_SPLINE_CURVE((1.01933756729741,1.17702963774851,1.01933756729741))
REPRESENTATION_ITEM('')
);
#230=(
BOUNDED_CURVE()
B_SPLINE_CURVE(2,(#54654,#54655,#54656),.UNSPECIFIED.,.F.,.F.)
B_SPLINE_CURVE_WITH_KNOTS((3,3),(0.0830692064483411,1.5163968327409),
 .UNSPECIFIED.)
CURVE()
GEOMETRIC_REPRESENTATION_ITEM()
RATIONAL_B_SPLINE_CURVE((1.01933756729741,1.17702963774851,1.01933756729741))
REPRESENTATION_ITEM('')
);
#231=(
BOUNDED_CURVE()
B_SPLINE_CURVE(2,(#54658,#54659,#54660),.UNSPECIFIED.,.F.,.F.)
B_SPLINE_CURVE_WITH_KNOTS((3,3),(0.083069206448341,1.5163968327409),
 .UNSPECIFIED.)
CURVE()
GEOMETRIC_REPRESENTATION_ITEM()
RATIONAL_B_SPLINE_CURVE((1.01933756729741,1.17702963774852,1.01933756729741))
REPRESENTATION_ITEM('')
);
#232=(
BOUNDED_CURVE()
B_SPLINE_CURVE(2,(#54662,#54663,#54664),.UNSPECIFIED.,.F.,.F.)
B_SPLINE_CURVE_WITH_KNOTS((3,3),(0.0830692064483414,1.5163968327409),
 .UNSPECIFIED.)
CURVE()
GEOMETRIC_REPRESENTATION_ITEM()
RATIONAL_B_SPLINE_CURVE((1.01933756729741,1.17702963774851,1.01933756729741))
REPRESENTATION_ITEM('')
);
#233=(
BOUNDED_CURVE()
B_SPLINE_CURVE(2,(#54665,#54666,#54667),.UNSPECIFIED.,.F.,.F.)
B_SPLINE_CURVE_WITH_KNOTS((3,3),(0.799733019594622,1.5163968327409),
 .UNSPECIFIED.)
CURVE()
GEOMETRIC_REPRESENTATION_ITEM()
RATIONAL_B_SPLINE_CURVE((1.09818360252296,1.09818360252296,1.01933756729741))
REPRESENTATION_ITEM('')
);
#234=(
BOUNDED_CURVE()
B_SPLINE_CURVE(2,(#54672,#54673,#54674),.UNSPECIFIED.,.F.,.F.)
B_SPLINE_CURVE_WITH_KNOTS((3,3),(0.083069206448341,1.5163968327409),
 .UNSPECIFIED.)
CURVE()
GEOMETRIC_REPRESENTATION_ITEM()
RATIONAL_B_SPLINE_CURVE((1.01933756729741,1.17702963774851,1.01933756729741))
REPRESENTATION_ITEM('')
);
#235=(
BOUNDED_CURVE()
B_SPLINE_CURVE(2,(#54679,#54680,#54681),.UNSPECIFIED.,.F.,.F.)
B_SPLINE_CURVE_WITH_KNOTS((3,3),(0.083069206448341,1.5163968327409),
 .UNSPECIFIED.)
CURVE()
GEOMETRIC_REPRESENTATION_ITEM()
RATIONAL_B_SPLINE_CURVE((1.01933756729741,1.17702963774851,1.01933756729741))
REPRESENTATION_ITEM('')
);
#236=(
BOUNDED_CURVE()
B_SPLINE_CURVE(2,(#54685,#54686,#54687),.UNSPECIFIED.,.F.,.F.)
B_SPLINE_CURVE_WITH_KNOTS((3,3),(0.0830692064483412,1.5163968327409),
 .UNSPECIFIED.)
CURVE()
GEOMETRIC_REPRESENTATION_ITEM()
RATIONAL_B_SPLINE_CURVE((1.01933756729741,1.17702963774851,1.01933756729741))
REPRESENTATION_ITEM('')
);
#237=(
BOUNDED_CURVE()
B_SPLINE_CURVE(2,(#54690,#54691,#54692),.UNSPECIFIED.,.F.,.F.)
B_SPLINE_CURVE_WITH_KNOTS((3,3),(0.0830692064483409,1.5163968327409),
 .UNSPECIFIED.)
CURVE()
GEOMETRIC_REPRESENTATION_ITEM()
RATIONAL_B_SPLINE_CURVE((1.01933756729741,1.17702963774851,1.01933756729741))
REPRESENTATION_ITEM('')
);
#238=(
BOUNDED_CURVE()
B_SPLINE_CURVE(2,(#54694,#54695,#54696),.UNSPECIFIED.,.F.,.F.)
B_SPLINE_CURVE_WITH_KNOTS((3,3),(0.799733019594622,1.5163968327409),
 .UNSPECIFIED.)
CURVE()
GEOMETRIC_REPRESENTATION_ITEM()
RATIONAL_B_SPLINE_CURVE((1.09818360252296,1.09818360252296,1.01933756729741))
REPRESENTATION_ITEM('')
);
#239=(
BOUNDED_CURVE()
B_SPLINE_CURVE(2,(#54699,#54700,#54701),.UNSPECIFIED.,.F.,.F.)
B_SPLINE_CURVE_WITH_KNOTS((3,3),(0.0830692064483412,0.799733019594622),
 .UNSPECIFIED.)
CURVE()
GEOMETRIC_REPRESENTATION_ITEM()
RATIONAL_B_SPLINE_CURVE((1.01933756729741,1.09818360252296,1.09818360252296))
REPRESENTATION_ITEM('')
);
#240=(
BOUNDED_CURVE()
B_SPLINE_CURVE(2,(#54702,#54703,#54704),.UNSPECIFIED.,.F.,.F.)
B_SPLINE_CURVE_WITH_KNOTS((3,3),(0.0830692064483414,1.5163968327409),
 .UNSPECIFIED.)
CURVE()
GEOMETRIC_REPRESENTATION_ITEM()
RATIONAL_B_SPLINE_CURVE((1.01933756729741,1.17702963774851,1.01933756729741))
REPRESENTATION_ITEM('')
);
#241=(
BOUNDED_CURVE()
B_SPLINE_CURVE(2,(#59352,#59353,#59354),.UNSPECIFIED.,.F.,.F.)
B_SPLINE_CURVE_WITH_KNOTS((3,3),(0.,0.00348603246849772),.UNSPECIFIED.)
CURVE()
GEOMETRIC_REPRESENTATION_ITEM()
RATIONAL_B_SPLINE_CURVE((1.,1.00000655818292,1.))
REPRESENTATION_ITEM('')
);
#242=(
BOUNDED_CURVE()
B_SPLINE_CURVE(2,(#59356,#59357,#59358),.UNSPECIFIED.,.F.,.F.)
B_SPLINE_CURVE_WITH_KNOTS((3,3),(0.,0.0034860324684977),.UNSPECIFIED.)
CURVE()
GEOMETRIC_REPRESENTATION_ITEM()
RATIONAL_B_SPLINE_CURVE((1.,1.00000655824651,1.))
REPRESENTATION_ITEM('')
);
#243=(
BOUNDED_CURVE()
B_SPLINE_CURVE(2,(#59361,#59362,#59363),.UNSPECIFIED.,.F.,.F.)
B_SPLINE_CURVE_WITH_KNOTS((3,3),(0.,0.00348603246849777),.UNSPECIFIED.)
CURVE()
GEOMETRIC_REPRESENTATION_ITEM()
RATIONAL_B_SPLINE_CURVE((1.,1.00000655828125,1.))
REPRESENTATION_ITEM('')
);
#244=(
BOUNDED_CURVE()
B_SPLINE_CURVE(2,(#59365,#59366,#59367),.UNSPECIFIED.,.F.,.F.)
B_SPLINE_CURVE_WITH_KNOTS((3,3),(0.,0.00348603246849785),.UNSPECIFIED.)
CURVE()
GEOMETRIC_REPRESENTATION_ITEM()
RATIONAL_B_SPLINE_CURVE((1.,1.00000655858972,1.))
REPRESENTATION_ITEM('')
);
#245=(
BOUNDED_CURVE()
B_SPLINE_CURVE(2,(#59370,#59371,#59372),.UNSPECIFIED.,.F.,.F.)
B_SPLINE_CURVE_WITH_KNOTS((3,3),(0.,0.00348603246849743),.UNSPECIFIED.)
CURVE()
GEOMETRIC_REPRESENTATION_ITEM()
RATIONAL_B_SPLINE_CURVE((1.,1.00000655826316,1.))
REPRESENTATION_ITEM('')
);
#246=(
BOUNDED_CURVE()
B_SPLINE_CURVE(2,(#59374,#59375,#59376),.UNSPECIFIED.,.F.,.F.)
B_SPLINE_CURVE_WITH_KNOTS((3,3),(0.,0.00348603246849747),.UNSPECIFIED.)
CURVE()
GEOMETRIC_REPRESENTATION_ITEM()
RATIONAL_B_SPLINE_CURVE((1.,1.00000655837246,1.))
REPRESENTATION_ITEM('')
);
#247=(
BOUNDED_CURVE()
B_SPLINE_CURVE(2,(#59379,#59380,#59381),.UNSPECIFIED.,.F.,.F.)
B_SPLINE_CURVE_WITH_KNOTS((3,3),(0.,0.00348603246849727),.UNSPECIFIED.)
CURVE()
GEOMETRIC_REPRESENTATION_ITEM()
RATIONAL_B_SPLINE_CURVE((1.,1.00000655774933,1.))
REPRESENTATION_ITEM('')
);
#248=(
BOUNDED_CURVE()
B_SPLINE_CURVE(2,(#59383,#59384,#59385),.UNSPECIFIED.,.F.,.F.)
B_SPLINE_CURVE_WITH_KNOTS((3,3),(0.,0.00348603246849747),.UNSPECIFIED.)
CURVE()
GEOMETRIC_REPRESENTATION_ITEM()
RATIONAL_B_SPLINE_CURVE((1.,1.00000655778188,1.))
REPRESENTATION_ITEM('')
);
#249=(
BOUNDED_CURVE()
B_SPLINE_CURVE(2,(#59388,#59389,#59390),.UNSPECIFIED.,.F.,.F.)
B_SPLINE_CURVE_WITH_KNOTS((3,3),(0.,0.00348603246849769),.UNSPECIFIED.)
CURVE()
GEOMETRIC_REPRESENTATION_ITEM()
RATIONAL_B_SPLINE_CURVE((1.,1.00000655825998,1.))
REPRESENTATION_ITEM('')
);
#250=(
BOUNDED_CURVE()
B_SPLINE_CURVE(2,(#59392,#59393,#59394),.UNSPECIFIED.,.F.,.F.)
B_SPLINE_CURVE_WITH_KNOTS((3,3),(0.,0.00348603246849761),.UNSPECIFIED.)
CURVE()
GEOMETRIC_REPRESENTATION_ITEM()
RATIONAL_B_SPLINE_CURVE((1.,1.00000655838487,1.))
REPRESENTATION_ITEM('')
);
#251=(
BOUNDED_CURVE()
B_SPLINE_CURVE(2,(#59397,#59398,#59399),.UNSPECIFIED.,.F.,.F.)
B_SPLINE_CURVE_WITH_KNOTS((3,3),(0.,0.00348603246849764),.UNSPECIFIED.)
CURVE()
GEOMETRIC_REPRESENTATION_ITEM()
RATIONAL_B_SPLINE_CURVE((1.,1.00000655822052,1.))
REPRESENTATION_ITEM('')
);
#252=(
BOUNDED_CURVE()
B_SPLINE_CURVE(2,(#59401,#59402,#59403),.UNSPECIFIED.,.F.,.F.)
B_SPLINE_CURVE_WITH_KNOTS((3,3),(0.,0.00348603246849749),.UNSPECIFIED.)
CURVE()
GEOMETRIC_REPRESENTATION_ITEM()
RATIONAL_B_SPLINE_CURVE((1.,1.00000655832735,1.))
REPRESENTATION_ITEM('')
);
#253=(
BOUNDED_CURVE()
B_SPLINE_CURVE(2,(#64951,#64952,#64953),.UNSPECIFIED.,.F.,.F.)
B_SPLINE_CURVE_WITH_KNOTS((3,3),(0.394392820917162,0.426830556686088),
 .UNSPECIFIED.)
CURVE()
GEOMETRIC_REPRESENTATION_ITEM()
RATIONAL_B_SPLINE_CURVE((1.00046081345666,1.00036632900905,1.00025318515883))
REPRESENTATION_ITEM('')
);
#254=(
BOUNDED_CURVE()
B_SPLINE_CURVE(2,(#64957,#64958,#64959),.UNSPECIFIED.,.F.,.F.)
B_SPLINE_CURVE_WITH_KNOTS((3,3),(0.0334492257654482,0.0658869615343763),
 .UNSPECIFIED.)
CURVE()
GEOMETRIC_REPRESENTATION_ITEM()
RATIONAL_B_SPLINE_CURVE((1.00025318515883,1.00036632900905,1.00046081345666))
REPRESENTATION_ITEM('')
);
#255=(
BOUNDED_CURVE()
B_SPLINE_CURVE(2,(#64996,#64997,#64998),.UNSPECIFIED.,.F.,.F.)
B_SPLINE_CURVE_WITH_KNOTS((3,3),(0.,0.193661196741385),.UNSPECIFIED.)
CURVE()
GEOMETRIC_REPRESENTATION_ITEM()
RATIONAL_B_SPLINE_CURVE((1.,1.00036563245858,1.00040353743124))
REPRESENTATION_ITEM('')
);
#256=(
BOUNDED_CURVE()
B_SPLINE_CURVE(2,(#65154,#65155,#65156),.UNSPECIFIED.,.F.,.F.)
B_SPLINE_CURVE_WITH_KNOTS((3,3),(0.238458916052879,0.432120112749345),
 .UNSPECIFIED.)
CURVE()
GEOMETRIC_REPRESENTATION_ITEM()
RATIONAL_B_SPLINE_CURVE((1.00040353742038,1.0003656324504,1.))
REPRESENTATION_ITEM('')
);
#257=(
BOUNDED_CURVE()
B_SPLINE_CURVE(2,(#65254,#65255,#65256),.UNSPECIFIED.,.F.,.F.)
B_SPLINE_CURVE_WITH_KNOTS((3,3),(0.486252464127642,0.752075607120858),
 .UNSPECIFIED.)
CURVE()
GEOMETRIC_REPRESENTATION_ITEM()
RATIONAL_B_SPLINE_CURVE((1.,1.,1.))
REPRESENTATION_ITEM('')
);
#258=(
BOUNDED_CURVE()
B_SPLINE_CURVE(2,(#65267,#65268,#65269),.UNSPECIFIED.,.F.,.F.)
B_SPLINE_CURVE_WITH_KNOTS((3,3),(0.121648463702186,0.387471606699022),
 .UNSPECIFIED.)
CURVE()
GEOMETRIC_REPRESENTATION_ITEM()
RATIONAL_B_SPLINE_CURVE((1.,1.,1.))
REPRESENTATION_ITEM('')
);
#259=(
BOUNDED_CURVE()
B_SPLINE_CURVE(2,(#65453,#65454,#65455),.UNSPECIFIED.,.F.,.F.)
B_SPLINE_CURVE_WITH_KNOTS((3,3),(0.000218747198876324,0.428298822677418),
 .UNSPECIFIED.)
CURVE()
GEOMETRIC_REPRESENTATION_ITEM()
RATIONAL_B_SPLINE_CURVE((1.,1.,1.))
REPRESENTATION_ITEM('')
);
#260=(
BOUNDED_CURVE()
B_SPLINE_CURVE(2,(#65456,#65457,#65458),.UNSPECIFIED.,.F.,.F.)
B_SPLINE_CURVE_WITH_KNOTS((3,3),(0.432240466163625,0.733007100595233),
 .UNSPECIFIED.)
CURVE()
GEOMETRIC_REPRESENTATION_ITEM()
RATIONAL_B_SPLINE_CURVE((1.,1.,1.))
REPRESENTATION_ITEM('')
);
#261=(
BOUNDED_CURVE()
B_SPLINE_CURVE(2,(#65913,#65914,#65915),.UNSPECIFIED.,.F.,.F.)
B_SPLINE_CURVE_WITH_KNOTS((3,3),(0.,0.428080075478541),.UNSPECIFIED.)
CURVE()
GEOMETRIC_REPRESENTATION_ITEM()
RATIONAL_B_SPLINE_CURVE((1.,1.,1.))
REPRESENTATION_ITEM('')
);
#262=(
BOUNDED_CURVE()
B_SPLINE_CURVE(2,(#65916,#65917,#65918),.UNSPECIFIED.,.F.,.F.)
B_SPLINE_CURVE_WITH_KNOTS((3,3),(0.12344249829562,0.424209132727228),
 .UNSPECIFIED.)
CURVE()
GEOMETRIC_REPRESENTATION_ITEM()
RATIONAL_B_SPLINE_CURVE((1.,1.,1.))
REPRESENTATION_ITEM('')
);
#263=(
BOUNDED_CURVE()
B_SPLINE_CURVE(2,(#70654,#70655,#70656),.UNSPECIFIED.,.F.,.F.)
B_SPLINE_CURVE_WITH_KNOTS((3,3),(0.0830692064483412,1.5163968327409),
 .UNSPECIFIED.)
CURVE()
GEOMETRIC_REPRESENTATION_ITEM()
RATIONAL_B_SPLINE_CURVE((1.01933756729741,1.17702963774851,1.01933756729741))
REPRESENTATION_ITEM('')
);
#264=(
BOUNDED_CURVE()
B_SPLINE_CURVE(2,(#70658,#70659,#70660),.UNSPECIFIED.,.F.,.F.)
B_SPLINE_CURVE_WITH_KNOTS((3,3),(0.0830692064483407,1.5163968327409),
 .UNSPECIFIED.)
CURVE()
GEOMETRIC_REPRESENTATION_ITEM()
RATIONAL_B_SPLINE_CURVE((1.01933756729741,1.17702963774851,1.01933756729741))
REPRESENTATION_ITEM('')
);
#265=(
BOUNDED_CURVE()
B_SPLINE_CURVE(2,(#70662,#70663,#70664),.UNSPECIFIED.,.F.,.F.)
B_SPLINE_CURVE_WITH_KNOTS((3,3),(0.0830692064483414,1.5163968327409),
 .UNSPECIFIED.)
CURVE()
GEOMETRIC_REPRESENTATION_ITEM()
RATIONAL_B_SPLINE_CURVE((1.01933756729741,1.17702963774851,1.01933756729741))
REPRESENTATION_ITEM('')
);
#266=(
BOUNDED_CURVE()
B_SPLINE_CURVE(2,(#70666,#70667,#70668),.UNSPECIFIED.,.F.,.F.)
B_SPLINE_CURVE_WITH_KNOTS((3,3),(0.0830692064483412,1.5163968327409),
 .UNSPECIFIED.)
CURVE()
GEOMETRIC_REPRESENTATION_ITEM()
RATIONAL_B_SPLINE_CURVE((1.01933756729741,1.17702963774851,1.01933756729741))
REPRESENTATION_ITEM('')
);
#267=(
BOUNDED_CURVE()
B_SPLINE_CURVE(2,(#70670,#70671,#70672),.UNSPECIFIED.,.F.,.F.)
B_SPLINE_CURVE_WITH_KNOTS((3,3),(0.799733019594622,1.5163968327409),
 .UNSPECIFIED.)
CURVE()
GEOMETRIC_REPRESENTATION_ITEM()
RATIONAL_B_SPLINE_CURVE((1.09818360252296,1.09818360252296,1.01933756729741))
REPRESENTATION_ITEM('')
);
#268=(
BOUNDED_CURVE()
B_SPLINE_CURVE(2,(#70677,#70678,#70679),.UNSPECIFIED.,.F.,.F.)
B_SPLINE_CURVE_WITH_KNOTS((3,3),(0.083069206448341,0.799733019594622),
 .UNSPECIFIED.)
CURVE()
GEOMETRIC_REPRESENTATION_ITEM()
RATIONAL_B_SPLINE_CURVE((1.01933756729741,1.09818360252296,1.09818360252296))
REPRESENTATION_ITEM('')
);
#269=(
BOUNDED_CURVE()
B_SPLINE_CURVE(2,(#70680,#70681,#70682),.UNSPECIFIED.,.F.,.F.)
B_SPLINE_CURVE_WITH_KNOTS((3,3),(0.0830692064483408,1.5163968327409),
 .UNSPECIFIED.)
CURVE()
GEOMETRIC_REPRESENTATION_ITEM()
RATIONAL_B_SPLINE_CURVE((1.01933756729741,1.17702963774851,1.01933756729741))
REPRESENTATION_ITEM('')
);
#270=B_SPLINE_SURFACE_WITH_KNOTS('',3,3,((#42029,#42030,#42031,#42032,#42033,
#42034,#42035,#42036,#42037,#42038,#42039,#42040,#42041,#42042,#42043,#42044,
#42045,#42046,#42047,#42048,#42049,#42050,#42051,#42052,#42053,#42054,#42055,
#42056,#42057,#42058,#42059,#42060,#42061,#42062,#42063,#42064,#42065,#42066,
#42067,#42068,#42069,#42070,#42071,#42072,#42073,#42074,#42075,#42076,#42077,
#42078,#42079,#42080,#42081,#42082,#42083,#42084,#42085,#42086,#42087,#42088,
#42089,#42090,#42091,#42092,#42093,#42094,#42095,#42096,#42097,#42098,#42099,
#42100,#42101,#42102,#42103,#42104,#42105,#42106,#42107,#42108,#42109,#42110,
#42111,#42112,#42113,#42114,#42115,#42116,#42117,#42118,#42119,#42120,#42121,
#42122,#42123,#42124,#42125,#42126,#42127,#42128,#42129,#42130,#42131,#42132,
#42133,#42134,#42135,#42136,#42137,#42138,#42139,#42140,#42141,#42142,#42143,
#42144,#42145,#42146,#42147,#42148,#42149,#42150,#42151,#42152,#42153,#42154,
#42155,#42156,#42157,#42158,#42159,#42160,#42161,#42162,#42163,#42164,#42165,
#42166,#42167,#42168,#42169,#42170,#42171,#42172,#42173,#42174,#42175,#42176,
#42177,#42178,#42179,#42180,#42181,#42182,#42183,#42184,#42185,#42186,#42187,
#42188,#42189,#42190,#42191,#42192,#42193,#42194,#42195),(#42196,#42197,
#42198,#42199,#42200,#42201,#42202,#42203,#42204,#42205,#42206,#42207,#42208,
#42209,#42210,#42211,#42212,#42213,#42214,#42215,#42216,#42217,#42218,#42219,
#42220,#42221,#42222,#42223,#42224,#42225,#42226,#42227,#42228,#42229,#42230,
#42231,#42232,#42233,#42234,#42235,#42236,#42237,#42238,#42239,#42240,#42241,
#42242,#42243,#42244,#42245,#42246,#42247,#42248,#42249,#42250,#42251,#42252,
#42253,#42254,#42255,#42256,#42257,#42258,#42259,#42260,#42261,#42262,#42263,
#42264,#42265,#42266,#42267,#42268,#42269,#42270,#42271,#42272,#42273,#42274,
#42275,#42276,#42277,#42278,#42279,#42280,#42281,#42282,#42283,#42284,#42285,
#42286,#42287,#42288,#42289,#42290,#42291,#42292,#42293,#42294,#42295,#42296,
#42297,#42298,#42299,#42300,#42301,#42302,#42303,#42304,#42305,#42306,#42307,
#42308,#42309,#42310,#42311,#42312,#42313,#42314,#42315,#42316,#42317,#42318,
#42319,#42320,#42321,#42322,#42323,#42324,#42325,#42326,#42327,#42328,#42329,
#42330,#42331,#42332,#42333,#42334,#42335,#42336,#42337,#42338,#42339,#42340,
#42341,#42342,#42343,#42344,#42345,#42346,#42347,#42348,#42349,#42350,#42351,
#42352,#42353,#42354,#42355,#42356,#42357,#42358,#42359,#42360,#42361,#42362),
(#42363,#42364,#42365,#42366,#42367,#42368,#42369,#42370,#42371,#42372,
#42373,#42374,#42375,#42376,#42377,#42378,#42379,#42380,#42381,#42382,#42383,
#42384,#42385,#42386,#42387,#42388,#42389,#42390,#42391,#42392,#42393,#42394,
#42395,#42396,#42397,#42398,#42399,#42400,#42401,#42402,#42403,#42404,#42405,
#42406,#42407,#42408,#42409,#42410,#42411,#42412,#42413,#42414,#42415,#42416,
#42417,#42418,#42419,#42420,#42421,#42422,#42423,#42424,#42425,#42426,#42427,
#42428,#42429,#42430,#42431,#42432,#42433,#42434,#42435,#42436,#42437,#42438,
#42439,#42440,#42441,#42442,#42443,#42444,#42445,#42446,#42447,#42448,#42449,
#42450,#42451,#42452,#42453,#42454,#42455,#42456,#42457,#42458,#42459,#42460,
#42461,#42462,#42463,#42464,#42465,#42466,#42467,#42468,#42469,#42470,#42471,
#42472,#42473,#42474,#42475,#42476,#42477,#42478,#42479,#42480,#42481,#42482,
#42483,#42484,#42485,#42486,#42487,#42488,#42489,#42490,#42491,#42492,#42493,
#42494,#42495,#42496,#42497,#42498,#42499,#42500,#42501,#42502,#42503,#42504,
#42505,#42506,#42507,#42508,#42509,#42510,#42511,#42512,#42513,#42514,#42515,
#42516,#42517,#42518,#42519,#42520,#42521,#42522,#42523,#42524,#42525,#42526,
#42527,#42528,#42529),(#42530,#42531,#42532,#42533,#42534,#42535,#42536,
#42537,#42538,#42539,#42540,#42541,#42542,#42543,#42544,#42545,#42546,#42547,
#42548,#42549,#42550,#42551,#42552,#42553,#42554,#42555,#42556,#42557,#42558,
#42559,#42560,#42561,#42562,#42563,#42564,#42565,#42566,#42567,#42568,#42569,
#42570,#42571,#42572,#42573,#42574,#42575,#42576,#42577,#42578,#42579,#42580,
#42581,#42582,#42583,#42584,#42585,#42586,#42587,#42588,#42589,#42590,#42591,
#42592,#42593,#42594,#42595,#42596,#42597,#42598,#42599,#42600,#42601,#42602,
#42603,#42604,#42605,#42606,#42607,#42608,#42609,#42610,#42611,#42612,#42613,
#42614,#42615,#42616,#42617,#42618,#42619,#42620,#42621,#42622,#42623,#42624,
#42625,#42626,#42627,#42628,#42629,#42630,#42631,#42632,#42633,#42634,#42635,
#42636,#42637,#42638,#42639,#42640,#42641,#42642,#42643,#42644,#42645,#42646,
#42647,#42648,#42649,#42650,#42651,#42652,#42653,#42654,#42655,#42656,#42657,
#42658,#42659,#42660,#42661,#42662,#42663,#42664,#42665,#42666,#42667,#42668,
#42669,#42670,#42671,#42672,#42673,#42674,#42675,#42676,#42677,#42678,#42679,
#42680,#42681,#42682,#42683,#42684,#42685,#42686,#42687,#42688,#42689,#42690,
#42691,#42692,#42693,#42694,#42695,#42696)),.UNSPECIFIED.,.F.,.F.,.F.,(4,
4),(4,1,1,1,1,1,1,1,1,1,1,1,1,1,1,1,1,1,1,1,1,1,1,1,1,1,1,1,1,1,1,1,1,1,
1,1,1,1,1,1,1,1,1,1,1,1,1,1,1,1,1,1,1,1,1,1,1,1,1,1,1,1,1,1,1,1,1,1,1,1,
1,1,1,1,1,1,1,1,1,1,1,1,1,1,1,1,1,1,1,1,1,1,1,1,1,1,1,1,1,1,1,1,1,1,1,1,
1,1,1,1,1,1,1,1,1,1,1,1,1,1,1,1,1,1,1,1,1,1,1,1,1,1,1,1,1,1,1,1,1,1,1,1,
1,1,1,1,1,1,1,1,1,1,1,1,1,1,1,1,1,1,1,1,1,1,4),(0.,0.198319817466637),(8.29931545526195,
8.79726554162164,9.29521562798133,9.79316571434102,10.2911158007007,10.7890658870604,
11.2870159734201,11.7849660597798,12.2829161461395,12.7808662324992,13.2788163188589,
13.7767664052186,14.2747164915782,14.7726665779379,15.2706166642976,15.7685667506573,
16.266516837017,16.7644669233767,17.2624170097364,17.7603670960961,18.2583171824558,
18.7562672688155,19.2542173551752,19.7521674415349,20.2501175278945,20.7480676142542,
21.2460177006139,21.7439677869736,22.2419178733333,22.739867959693,23.2378180460527,
23.7357681324124,24.2337182187721,24.7316683051318,25.2296183914915,25.7275684778511,
26.2255185642108,26.7234686505705,27.2214187369302,27.7193688232899,28.2173189096496,
28.7152689960093,29.213219082369,29.7111691687287,30.2091192550884,30.7070693414481,
31.2050194278078,31.7029695141674,32.2009196005271,32.6988696868868,33.1968197732465,
33.6947698596062,34.1927199459659,34.6906700323256,35.1886201186853,35.686570205045,
36.1845202914047,36.6824703777644,37.1804204641241,37.6783705504837,38.1763206368434,
38.6742707232031,39.1722208095628,39.6701708959225,40.1681209822822,40.6660710686419,
41.1640211550016,41.6619712413613,42.159921327721,42.6578714140807,43.1558215004404,
43.6537715868,44.1517216731597,44.6496717595194,45.1476218458791,45.6455719322388,
46.1435220185985,46.6414721049582,47.1394221913179,47.6373722776776,48.1353223640373,
48.633272450397,49.1312225367567,49.6291726231163,50.127122709476,50.6250727958357,
51.1230228821954,51.6209729685551,52.1189230549148,52.6168731412745,53.1148232276342,
53.6127733139939,54.1107234003536,54.6086734867133,55.106623573073,55.6045736594326,
56.1025237457923,56.600473832152,57.0984239185117,57.5963740048714,58.0943240912311,
58.5922741775908,59.0902242639505,59.5881743503102,60.0861244366699,60.5840745230296,
61.0820246093893,61.5799746957489,62.0779247821086,62.5758748684683,63.073824954828,
63.5717750411877,64.0697251275474,64.5676752139071,65.0656253002668,65.5635753866265,
66.0615254729862,66.5594755593459,67.0574256457055,67.5553757320652,68.0533258184249,
68.5512759047846,69.0492259911443,69.547176077504,70.0451261638637,70.5430762502234,
71.0410263365831,71.5389764229428,72.0369265093025,72.5348765956622,73.0328266820218,
73.5307767683815,74.0287268547412,74.5266769411009,75.0246270274606,75.5225771138203,
76.02052720018,76.5184772865397,77.0164273728994,77.5143774592591,78.0123275456188,
78.5102776319785,79.0082277183381,79.5061778046978,80.0041278910575,80.5020779774172,
81.0000280637769,81.4979781501366,81.9959282364963,82.493878322856,82.9918284092157,
83.4897784955754,83.9877285819351,84.4856786682948,84.9836287546544,85.4815788410141,
85.9795289273738,86.4774790137335,86.9754291000932,87.4733791864529,87.9713292728126,
88.4692793591723,88.967229445532,89.4651795318917,89.9631296182514),
 .UNSPECIFIED.);
#271=B_SPLINE_SURFACE_WITH_KNOTS('',3,3,((#42914,#42915,#42916,#42917,#42918,
#42919,#42920,#42921,#42922,#42923,#42924,#42925,#42926,#42927,#42928,#42929,
#42930,#42931,#42932,#42933,#42934,#42935,#42936,#42937,#42938,#42939,#42940,
#42941,#42942,#42943,#42944,#42945,#42946,#42947,#42948,#42949,#42950,#42951,
#42952,#42953,#42954,#42955,#42956,#42957,#42958,#42959,#42960,#42961,#42962,
#42963,#42964,#42965,#42966,#42967,#42968,#42969,#42970,#42971,#42972,#42973,
#42974,#42975,#42976,#42977,#42978,#42979,#42980,#42981,#42982,#42983,#42984,
#42985,#42986,#42987,#42988,#42989,#42990,#42991,#42992,#42993,#42994,#42995,
#42996,#42997,#42998,#42999,#43000,#43001,#43002,#43003,#43004,#43005,#43006,
#43007,#43008,#43009,#43010,#43011,#43012,#43013,#43014,#43015,#43016,#43017,
#43018,#43019,#43020,#43021,#43022,#43023,#43024,#43025,#43026,#43027,#43028,
#43029,#43030,#43031,#43032,#43033,#43034,#43035,#43036,#43037,#43038,#43039,
#43040,#43041,#43042,#43043,#43044,#43045,#43046,#43047,#43048,#43049,#43050,
#43051,#43052,#43053,#43054,#43055,#43056,#43057,#43058,#43059,#43060,#43061,
#43062,#43063,#43064,#43065,#43066,#43067,#43068,#43069,#43070,#43071,#43072,
#43073,#43074,#43075,#43076,#43077,#43078,#43079,#43080),(#43081,#43082,
#43083,#43084,#43085,#43086,#43087,#43088,#43089,#43090,#43091,#43092,#43093,
#43094,#43095,#43096,#43097,#43098,#43099,#43100,#43101,#43102,#43103,#43104,
#43105,#43106,#43107,#43108,#43109,#43110,#43111,#43112,#43113,#43114,#43115,
#43116,#43117,#43118,#43119,#43120,#43121,#43122,#43123,#43124,#43125,#43126,
#43127,#43128,#43129,#43130,#43131,#43132,#43133,#43134,#43135,#43136,#43137,
#43138,#43139,#43140,#43141,#43142,#43143,#43144,#43145,#43146,#43147,#43148,
#43149,#43150,#43151,#43152,#43153,#43154,#43155,#43156,#43157,#43158,#43159,
#43160,#43161,#43162,#43163,#43164,#43165,#43166,#43167,#43168,#43169,#43170,
#43171,#43172,#43173,#43174,#43175,#43176,#43177,#43178,#43179,#43180,#43181,
#43182,#43183,#43184,#43185,#43186,#43187,#43188,#43189,#43190,#43191,#43192,
#43193,#43194,#43195,#43196,#43197,#43198,#43199,#43200,#43201,#43202,#43203,
#43204,#43205,#43206,#43207,#43208,#43209,#43210,#43211,#43212,#43213,#43214,
#43215,#43216,#43217,#43218,#43219,#43220,#43221,#43222,#43223,#43224,#43225,
#43226,#43227,#43228,#43229,#43230,#43231,#43232,#43233,#43234,#43235,#43236,
#43237,#43238,#43239,#43240,#43241,#43242,#43243,#43244,#43245,#43246,#43247),
(#43248,#43249,#43250,#43251,#43252,#43253,#43254,#43255,#43256,#43257,
#43258,#43259,#43260,#43261,#43262,#43263,#43264,#43265,#43266,#43267,#43268,
#43269,#43270,#43271,#43272,#43273,#43274,#43275,#43276,#43277,#43278,#43279,
#43280,#43281,#43282,#43283,#43284,#43285,#43286,#43287,#43288,#43289,#43290,
#43291,#43292,#43293,#43294,#43295,#43296,#43297,#43298,#43299,#43300,#43301,
#43302,#43303,#43304,#43305,#43306,#43307,#43308,#43309,#43310,#43311,#43312,
#43313,#43314,#43315,#43316,#43317,#43318,#43319,#43320,#43321,#43322,#43323,
#43324,#43325,#43326,#43327,#43328,#43329,#43330,#43331,#43332,#43333,#43334,
#43335,#43336,#43337,#43338,#43339,#43340,#43341,#43342,#43343,#43344,#43345,
#43346,#43347,#43348,#43349,#43350,#43351,#43352,#43353,#43354,#43355,#43356,
#43357,#43358,#43359,#43360,#43361,#43362,#43363,#43364,#43365,#43366,#43367,
#43368,#43369,#43370,#43371,#43372,#43373,#43374,#43375,#43376,#43377,#43378,
#43379,#43380,#43381,#43382,#43383,#43384,#43385,#43386,#43387,#43388,#43389,
#43390,#43391,#43392,#43393,#43394,#43395,#43396,#43397,#43398,#43399,#43400,
#43401,#43402,#43403,#43404,#43405,#43406,#43407,#43408,#43409,#43410,#43411,
#43412,#43413,#43414),(#43415,#43416,#43417,#43418,#43419,#43420,#43421,
#43422,#43423,#43424,#43425,#43426,#43427,#43428,#43429,#43430,#43431,#43432,
#43433,#43434,#43435,#43436,#43437,#43438,#43439,#43440,#43441,#43442,#43443,
#43444,#43445,#43446,#43447,#43448,#43449,#43450,#43451,#43452,#43453,#43454,
#43455,#43456,#43457,#43458,#43459,#43460,#43461,#43462,#43463,#43464,#43465,
#43466,#43467,#43468,#43469,#43470,#43471,#43472,#43473,#43474,#43475,#43476,
#43477,#43478,#43479,#43480,#43481,#43482,#43483,#43484,#43485,#43486,#43487,
#43488,#43489,#43490,#43491,#43492,#43493,#43494,#43495,#43496,#43497,#43498,
#43499,#43500,#43501,#43502,#43503,#43504,#43505,#43506,#43507,#43508,#43509,
#43510,#43511,#43512,#43513,#43514,#43515,#43516,#43517,#43518,#43519,#43520,
#43521,#43522,#43523,#43524,#43525,#43526,#43527,#43528,#43529,#43530,#43531,
#43532,#43533,#43534,#43535,#43536,#43537,#43538,#43539,#43540,#43541,#43542,
#43543,#43544,#43545,#43546,#43547,#43548,#43549,#43550,#43551,#43552,#43553,
#43554,#43555,#43556,#43557,#43558,#43559,#43560,#43561,#43562,#43563,#43564,
#43565,#43566,#43567,#43568,#43569,#43570,#43571,#43572,#43573,#43574,#43575,
#43576,#43577,#43578,#43579,#43580,#43581)),.UNSPECIFIED.,.F.,.F.,.F.,(4,
4),(4,1,1,1,1,1,1,1,1,1,1,1,1,1,1,1,1,1,1,1,1,1,1,1,1,1,1,1,1,1,1,1,1,1,
1,1,1,1,1,1,1,1,1,1,1,1,1,1,1,1,1,1,1,1,1,1,1,1,1,1,1,1,1,1,1,1,1,1,1,1,
1,1,1,1,1,1,1,1,1,1,1,1,1,1,1,1,1,1,1,1,1,1,1,1,1,1,1,1,1,1,1,1,1,1,1,1,
1,1,1,1,1,1,1,1,1,1,1,1,1,1,1,1,1,1,1,1,1,1,1,1,1,1,1,1,1,1,1,1,1,1,1,1,
1,1,1,1,1,1,1,1,1,1,1,1,1,1,1,1,1,1,1,1,1,1,4),(0.,0.198319817466637),(11.6150328478181,
12.1129829341778,12.6109330205375,13.1088831068972,13.6068331932569,14.1047832796166,
14.6027333659763,15.100683452336,15.5986335386957,16.0965836250554,16.594533711415,
17.0924837977747,17.5904338841344,18.0883839704941,18.5863340568538,19.0842841432135,
19.5822342295732,20.0801843159329,20.5781344022926,21.0760844886523,21.574034575012,
22.0719846613717,22.5699347477313,23.067884834091,23.5658349204507,24.0637850068104,
24.5617350931701,25.0596851795298,25.5576352658895,26.0555853522492,26.5535354386089,
27.0514855249686,27.5494356113283,28.047385697688,28.5453357840476,29.0432858704073,
29.541235956767,30.0391860431267,30.5371361294864,31.0350862158461,31.5330363022058,
32.0309863885655,32.5289364749252,33.0268865612849,33.5248366476446,34.0227867340043,
34.520736820364,35.0186869067236,35.5166369930833,36.014587079443,36.5125371658027,
37.0104872521624,37.5084373385221,38.0063874248818,38.5043375112415,39.0022875976012,
39.5002376839609,39.9981877703206,40.4961378566802,40.9940879430399,41.4920380293996,
41.9899881157593,42.487938202119,42.9858882884787,43.4838383748384,43.9817884611981,
44.4797385475578,44.9776886339175,45.4756387202772,45.9735888066369,46.4715388929966,
46.9694889793562,47.4674390657159,47.9653891520756,48.4633392384353,48.961289324795,
49.4592394111547,49.9571894975144,50.4551395838741,50.9530896702338,51.4510397565935,
51.9489898429532,52.4469399293129,52.9448900156726,53.4428401020322,53.9407901883919,
54.4387402747516,54.9366903611113,55.434640447471,55.9325905338307,56.4305406201904,
56.9284907065501,57.4264407929098,57.9243908792695,58.4223409656292,58.9202910519889,
59.4182411383485,59.9161912247082,60.4141413110679,60.9120913974276,61.4100414837873,
61.907991570147,62.4059416565067,62.9038917428664,63.4018418292261,63.8997919155858,
64.3977420019455,64.8956920883052,65.3936421746648,65.8915922610245,66.3895423473842,
66.8874924337439,67.3854425201036,67.8833926064633,68.381342692823,68.8792927791827,
69.3772428655424,69.8751929519021,70.3731430382618,70.8710931246215,71.3690432109811,
71.8669932973408,72.3649433837005,72.8628934700602,73.3608435564199,73.8587936427796,
74.3567437291393,74.854693815499,75.3526439018587,75.8505939882184,76.3485440745781,
76.8464941609378,77.3444442472975,77.8423943336572,78.3403444200168,78.8382945063765,
79.3362445927362,79.8341946790959,80.3321447654556,80.8300948518153,81.328044938175,
81.8259950245347,82.3239451108944,82.8218951972541,83.3198452836138,83.8177953699735,
84.3157454563331,84.8136955426928,85.3116456290525,85.8095957154122,86.3075458017719,
86.8054958881316,87.3034459744913,87.801396060851,88.2993461472107,88.7972962335704,
89.2952463199301,89.7931964062898,90.2911464926494,90.7890965790091,91.2870466653688,
91.7849967517285,92.2829468380882,92.7808969244479,93.2788470108076),
 .UNSPECIFIED.);
#272=B_SPLINE_SURFACE_WITH_KNOTS('',3,3,((#44072,#44073,#44074,#44075,#44076,
#44077,#44078,#44079,#44080,#44081,#44082,#44083,#44084,#44085,#44086,#44087,
#44088,#44089,#44090,#44091,#44092,#44093,#44094,#44095,#44096,#44097,#44098,
#44099,#44100,#44101,#44102,#44103,#44104,#44105,#44106,#44107,#44108,#44109,
#44110,#44111,#44112,#44113,#44114,#44115,#44116,#44117,#44118,#44119,#44120,
#44121,#44122,#44123,#44124,#44125,#44126,#44127,#44128,#44129,#44130,#44131,
#44132,#44133,#44134,#44135,#44136),(#44137,#44138,#44139,#44140,#44141,
#44142,#44143,#44144,#44145,#44146,#44147,#44148,#44149,#44150,#44151,#44152,
#44153,#44154,#44155,#44156,#44157,#44158,#44159,#44160,#44161,#44162,#44163,
#44164,#44165,#44166,#44167,#44168,#44169,#44170,#44171,#44172,#44173,#44174,
#44175,#44176,#44177,#44178,#44179,#44180,#44181,#44182,#44183,#44184,#44185,
#44186,#44187,#44188,#44189,#44190,#44191,#44192,#44193,#44194,#44195,#44196,
#44197,#44198,#44199,#44200,#44201),(#44202,#44203,#44204,#44205,#44206,
#44207,#44208,#44209,#44210,#44211,#44212,#44213,#44214,#44215,#44216,#44217,
#44218,#44219,#44220,#44221,#44222,#44223,#44224,#44225,#44226,#44227,#44228,
#44229,#44230,#44231,#44232,#44233,#44234,#44235,#44236,#44237,#44238,#44239,
#44240,#44241,#44242,#44243,#44244,#44245,#44246,#44247,#44248,#44249,#44250,
#44251,#44252,#44253,#44254,#44255,#44256,#44257,#44258,#44259,#44260,#44261,
#44262,#44263,#44264,#44265,#44266),(#44267,#44268,#44269,#44270,#44271,
#44272,#44273,#44274,#44275,#44276,#44277,#44278,#44279,#44280,#44281,#44282,
#44283,#44284,#44285,#44286,#44287,#44288,#44289,#44290,#44291,#44292,#44293,
#44294,#44295,#44296,#44297,#44298,#44299,#44300,#44301,#44302,#44303,#44304,
#44305,#44306,#44307,#44308,#44309,#44310,#44311,#44312,#44313,#44314,#44315,
#44316,#44317,#44318,#44319,#44320,#44321,#44322,#44323,#44324,#44325,#44326,
#44327,#44328,#44329,#44330,#44331)),.UNSPECIFIED.,.F.,.T.,.F.,(4,4),(4,
1,1,1,1,1,1,1,1,1,1,1,1,1,1,1,1,1,1,1,1,1,1,1,1,1,1,1,1,1,1,1,1,1,1,1,1,
1,1,1,1,1,1,1,1,1,1,1,1,1,1,1,1,1,1,1,1,1,1,1,1,1,4),(0.,1.),(0.,0.346838652723539,
0.433548315904424,0.455225731699645,0.476903147494867,0.498580563290088,
0.520257979085309,0.693677305447079,0.7153547212423,0.737032137037521,0.780386968627963,
0.823741800218406,0.867096631808848,0.953806294989733,0.997161126580175,
1.04051595817062,1.38735461089416,1.39096751352669,1.39458041615923,1.4018062214243,
1.41625783195445,1.42348363721953,1.4307094424846,1.44516105301475,1.50296749513534,
1.56077393725593,1.61858037937652,1.7341932636177,1.79199970573829,1.84980614785888,
2.08103191634124,2.13883835846183,2.19664480058242,2.25445124270301,2.31225768482359,
2.54348345330595,2.65909633754713,2.77470922178831,2.94812854815008,3.12154787451185,
3.20825753769274,3.29496720087362,3.38167686405451,3.42503169564495,3.43587040354256,
3.44670911144017,3.45754781933778,3.46838652723539,3.64180585359716,3.81522517995893,
3.85858001154937,3.90193484313982,3.9886445063207,4.07535416950159,4.11870900109203,
4.16206383268247,4.33548315904424,4.34632186694185,4.35716057483946,4.37883799063468,
4.42219282222513,4.50890248540601,4.85574113812955),.UNSPECIFIED.);
#273=B_SPLINE_SURFACE_WITH_KNOTS('',3,3,((#44815,#44816,#44817,#44818,#44819,
#44820,#44821,#44822,#44823,#44824,#44825,#44826,#44827,#44828,#44829,#44830,
#44831,#44832,#44833,#44834,#44835,#44836,#44837),(#44838,#44839,#44840,
#44841,#44842,#44843,#44844,#44845,#44846,#44847,#44848,#44849,#44850,#44851,
#44852,#44853,#44854,#44855,#44856,#44857,#44858,#44859,#44860),(#44861,
#44862,#44863,#44864,#44865,#44866,#44867,#44868,#44869,#44870,#44871,#44872,
#44873,#44874,#44875,#44876,#44877,#44878,#44879,#44880,#44881,#44882,#44883),
(#44884,#44885,#44886,#44887,#44888,#44889,#44890,#44891,#44892,#44893,
#44894,#44895,#44896,#44897,#44898,#44899,#44900,#44901,#44902,#44903,#44904,
#44905,#44906)),.UNSPECIFIED.,.F.,.T.,.F.,(4,4),(4,1,1,1,1,2,2,1,1,1,1,
1,2,1,1,1,1,4),(0.,1.),(1.16422336569995,1.62550842979414,2.08679349388834,
2.31743602593544,2.54807855798254,3.00936362207673,3.08125863299769,3.36971080227501,
3.65816297155233,3.73027601387166,3.802389056191,3.94661514082966,4.23506731010698,
4.71432612693143,5.19358494375588,5.67284376058034,5.91247316899256,6.15210257740479),
 .UNSPECIFIED.);
#274=B_SPLINE_SURFACE_WITH_KNOTS('',3,3,((#46301,#46302,#46303,#46304,#46305,
#46306,#46307,#46308,#46309,#46310,#46311,#46312,#46313,#46314,#46315,#46316,
#46317,#46318,#46319,#46320,#46321,#46322,#46323,#46324,#46325,#46326,#46327,
#46328,#46329,#46330,#46331,#46332,#46333,#46334,#46335,#46336,#46337,#46338,
#46339,#46340,#46341,#46342,#46343,#46344,#46345,#46346,#46347,#46348,#46349,
#46350,#46351,#46352,#46353,#46354,#46355,#46356,#46357,#46358,#46359,#46360,
#46361,#46362,#46363,#46364,#46365,#46366,#46367,#46368,#46369,#46370,#46371,
#46372,#46373,#46374,#46375,#46376,#46377,#46378,#46379,#46380,#46381,#46382,
#46383,#46384,#46385,#46386,#46387,#46388,#46389,#46390,#46391,#46392,#46393),
(#46394,#46395,#46396,#46397,#46398,#46399,#46400,#46401,#46402,#46403,
#46404,#46405,#46406,#46407,#46408,#46409,#46410,#46411,#46412,#46413,#46414,
#46415,#46416,#46417,#46418,#46419,#46420,#46421,#46422,#46423,#46424,#46425,
#46426,#46427,#46428,#46429,#46430,#46431,#46432,#46433,#46434,#46435,#46436,
#46437,#46438,#46439,#46440,#46441,#46442,#46443,#46444,#46445,#46446,#46447,
#46448,#46449,#46450,#46451,#46452,#46453,#46454,#46455,#46456,#46457,#46458,
#46459,#46460,#46461,#46462,#46463,#46464,#46465,#46466,#46467,#46468,#46469,
#46470,#46471,#46472,#46473,#46474,#46475,#46476,#46477,#46478,#46479,#46480,
#46481,#46482,#46483,#46484,#46485,#46486),(#46487,#46488,#46489,#46490,
#46491,#46492,#46493,#46494,#46495,#46496,#46497,#46498,#46499,#46500,#46501,
#46502,#46503,#46504,#46505,#46506,#46507,#46508,#46509,#46510,#46511,#46512,
#46513,#46514,#46515,#46516,#46517,#46518,#46519,#46520,#46521,#46522,#46523,
#46524,#46525,#46526,#46527,#46528,#46529,#46530,#46531,#46532,#46533,#46534,
#46535,#46536,#46537,#46538,#46539,#46540,#46541,#46542,#46543,#46544,#46545,
#46546,#46547,#46548,#46549,#46550,#46551,#46552,#46553,#46554,#46555,#46556,
#46557,#46558,#46559,#46560,#46561,#46562,#46563,#46564,#46565,#46566,#46567,
#46568,#46569,#46570,#46571,#46572,#46573,#46574,#46575,#46576,#46577,#46578,
#46579),(#46580,#46581,#46582,#46583,#46584,#46585,#46586,#46587,#46588,
#46589,#46590,#46591,#46592,#46593,#46594,#46595,#46596,#46597,#46598,#46599,
#46600,#46601,#46602,#46603,#46604,#46605,#46606,#46607,#46608,#46609,#46610,
#46611,#46612,#46613,#46614,#46615,#46616,#46617,#46618,#46619,#46620,#46621,
#46622,#46623,#46624,#46625,#46626,#46627,#46628,#46629,#46630,#46631,#46632,
#46633,#46634,#46635,#46636,#46637,#46638,#46639,#46640,#46641,#46642,#46643,
#46644,#46645,#46646,#46647,#46648,#46649,#46650,#46651,#46652,#46653,#46654,
#46655,#46656,#46657,#46658,#46659,#46660,#46661,#46662,#46663,#46664,#46665,
#46666,#46667,#46668,#46669,#46670,#46671,#46672)),.UNSPECIFIED.,.F.,.F.,
 .F.,(4,4),(4,1,1,1,1,1,1,1,1,1,1,1,1,1,1,1,1,1,1,1,1,1,1,1,1,1,1,1,1,1,
1,1,1,1,1,1,1,1,1,1,1,1,1,1,1,1,1,1,1,1,1,1,1,1,1,1,1,1,1,1,1,1,1,1,1,1,
1,1,1,1,1,1,1,1,1,1,1,1,1,1,1,1,1,1,1,1,1,1,1,1,4),(0.,0.164689164286341),
(8.30638927278254,8.80158653784135,9.29678380290015,9.79198106795896,10.2871783330178,
10.7823755980766,11.2775728631354,11.7727701281942,12.267967393253,12.7631646583118,
13.2583619233706,13.7535591884294,14.2487564534882,14.743953718547,15.2391509836058,
15.7343482486646,16.2295455137234,16.7247427787822,17.219940043841,17.7151373088998,
18.2103345739587,18.7055318390175,19.2007291040763,19.6959263691351,20.1911236341939,
20.6863208992527,21.1815181643115,21.6767154293703,22.1719126944291,22.6671099594879,
23.1623072245467,23.6575044896055,24.1527017546643,24.6478990197231,25.1430962847819,
25.6382935498407,26.1334908148995,26.6286880799584,27.1238853450172,27.619082610076,
28.1142798751348,28.6094771401936,29.1046744052524,29.5998716703112,30.09506893537,
30.5902662004288,31.0854634654876,31.5806607305464,32.0758579956052,32.571055260664,
33.0662525257228,33.5614497907816,34.0566470558404,34.5518443208992,35.0470415859581,
35.5422388510169,36.0374361160757,36.5326333811345,37.0278306461933,37.5230279112521,
38.0182251763109,38.5134224413697,39.0086197064285,39.5038169714873,39.9990142365461,
40.4942115016049,40.9894087666637,41.4846060317225,41.9798032967813,42.4750005618401,
42.9701978268989,43.4653950919578,43.9605923570166,44.4557896220754,44.9509868871342,
45.446184152193,45.9413814172518,46.4365786823106,46.9317759473694,47.4269732124282,
47.922170477487,48.4173677425458,48.9125650076046,49.4077622726634,49.9029595377222,
50.398156802781,50.8933540678398,51.3885513328986,51.8837485979574,52.3789458630163,
52.8741431280751),.UNSPECIFIED.);
#275=B_SPLINE_SURFACE_WITH_KNOTS('',3,3,((#46887,#46888,#46889,#46890,#46891,
#46892,#46893,#46894,#46895,#46896,#46897,#46898,#46899,#46900,#46901,#46902,
#46903,#46904,#46905,#46906,#46907,#46908,#46909,#46910,#46911,#46912,#46913,
#46914,#46915,#46916,#46917,#46918,#46919,#46920,#46921,#46922,#46923,#46924,
#46925,#46926,#46927,#46928,#46929,#46930,#46931,#46932,#46933,#46934,#46935,
#46936,#46937,#46938,#46939,#46940,#46941,#46942,#46943,#46944,#46945,#46946,
#46947,#46948,#46949,#46950,#46951,#46952,#46953,#46954,#46955,#46956,#46957,
#46958,#46959,#46960,#46961,#46962,#46963,#46964,#46965,#46966,#46967,#46968,
#46969,#46970,#46971,#46972,#46973,#46974,#46975,#46976,#46977,#46978,#46979),
(#46980,#46981,#46982,#46983,#46984,#46985,#46986,#46987,#46988,#46989,
#46990,#46991,#46992,#46993,#46994,#46995,#46996,#46997,#46998,#46999,#47000,
#47001,#47002,#47003,#47004,#47005,#47006,#47007,#47008,#47009,#47010,#47011,
#47012,#47013,#47014,#47015,#47016,#47017,#47018,#47019,#47020,#47021,#47022,
#47023,#47024,#47025,#47026,#47027,#47028,#47029,#47030,#47031,#47032,#47033,
#47034,#47035,#47036,#47037,#47038,#47039,#47040,#47041,#47042,#47043,#47044,
#47045,#47046,#47047,#47048,#47049,#47050,#47051,#47052,#47053,#47054,#47055,
#47056,#47057,#47058,#47059,#47060,#47061,#47062,#47063,#47064,#47065,#47066,
#47067,#47068,#47069,#47070,#47071,#47072),(#47073,#47074,#47075,#47076,
#47077,#47078,#47079,#47080,#47081,#47082,#47083,#47084,#47085,#47086,#47087,
#47088,#47089,#47090,#47091,#47092,#47093,#47094,#47095,#47096,#47097,#47098,
#47099,#47100,#47101,#47102,#47103,#47104,#47105,#47106,#47107,#47108,#47109,
#47110,#47111,#47112,#47113,#47114,#47115,#47116,#47117,#47118,#47119,#47120,
#47121,#47122,#47123,#47124,#47125,#47126,#47127,#47128,#47129,#47130,#47131,
#47132,#47133,#47134,#47135,#47136,#47137,#47138,#47139,#47140,#47141,#47142,
#47143,#47144,#47145,#47146,#47147,#47148,#47149,#47150,#47151,#47152,#47153,
#47154,#47155,#47156,#47157,#47158,#47159,#47160,#47161,#47162,#47163,#47164,
#47165),(#47166,#47167,#47168,#47169,#47170,#47171,#47172,#47173,#47174,
#47175,#47176,#47177,#47178,#47179,#47180,#47181,#47182,#47183,#47184,#47185,
#47186,#47187,#47188,#47189,#47190,#47191,#47192,#47193,#47194,#47195,#47196,
#47197,#47198,#47199,#47200,#47201,#47202,#47203,#47204,#47205,#47206,#47207,
#47208,#47209,#47210,#47211,#47212,#47213,#47214,#47215,#47216,#47217,#47218,
#47219,#47220,#47221,#47222,#47223,#47224,#47225,#47226,#47227,#47228,#47229,
#47230,#47231,#47232,#47233,#47234,#47235,#47236,#47237,#47238,#47239,#47240,
#47241,#47242,#47243,#47244,#47245,#47246,#47247,#47248,#47249,#47250,#47251,
#47252,#47253,#47254,#47255,#47256,#47257,#47258)),.UNSPECIFIED.,.F.,.F.,
 .F.,(4,4),(4,1,1,1,1,1,1,1,1,1,1,1,1,1,1,1,1,1,1,1,1,1,1,1,1,1,1,1,1,1,
1,1,1,1,1,1,1,1,1,1,1,1,1,1,1,1,1,1,1,1,1,1,1,1,1,1,1,1,1,1,1,1,1,1,1,1,
1,1,1,1,1,1,1,1,1,1,1,1,1,1,1,1,1,1,1,1,1,1,1,1,4),(0.,0.164689164286341),
(11.6152142277547,12.1104114928135,12.6056087578723,13.1008060229311,13.59600328799,
14.0912005530488,14.5863978181076,15.0815950831664,15.5767923482252,16.071989613284,
16.5671868783428,17.0623841434016,17.5575814084604,18.0527786735192,18.547975938578,
19.0431732036368,19.5383704686956,20.0335677337544,20.5287649988132,21.023962263872,
21.5191595289308,22.0143567939897,22.5095540590485,23.0047513241073,23.4999485891661,
23.9951458542249,24.4903431192837,24.9855403843425,25.4807376494013,25.9759349144601,
26.4711321795189,26.9663294445777,27.4615267096365,27.9567239746953,28.4519212397541,
28.9471185048129,29.4423157698717,29.9375130349305,30.4327102999894,30.9279075650482,
31.423104830107,31.9183020951658,32.4134993602246,32.9086966252834,33.4038938903422,
33.899091155401,34.3942884204598,34.8894856855186,35.3846829505774,35.8798802156362,
36.375077480695,36.8702747457538,37.3654720108126,37.8606692758714,38.3558665409303,
38.8510638059891,39.3462610710479,39.8414583361067,40.3366556011655,40.8318528662243,
41.3270501312831,41.8222473963419,42.3174446614007,42.8126419264595,43.3078391915183,
43.8030364565771,44.2982337216359,44.7934309866947,45.2886282517535,45.7838255168123,
46.2790227818711,46.7742200469299,47.2694173119888,47.7646145770476,48.2598118421064,
48.7550091071652,49.250206372224,49.7454036372828,50.2406009023416,50.7357981674004,
51.2309954324592,51.726192697518,52.2213899625768,52.7165872276356,53.2117844926944,
53.7069817577532,54.202179022812,54.6973762878708,55.1925735529296,55.6877708179885,
56.1829680830473),.UNSPECIFIED.);
#276=B_SPLINE_SURFACE_WITH_KNOTS('',3,3,((#51283,#51284,#51285,#51286,#51287,
#51288,#51289,#51290,#51291,#51292,#51293,#51294,#51295,#51296,#51297,#51298,
#51299,#51300,#51301,#51302,#51303,#51304,#51305,#51306,#51307,#51308,#51309,
#51310,#51311,#51312,#51313,#51314,#51315,#51316,#51317,#51318,#51319,#51320,
#51321,#51322,#51323,#51324,#51325,#51326,#51327,#51328,#51329,#51330,#51331,
#51332,#51333,#51334,#51335,#51336,#51337,#51338,#51339,#51340,#51341,#51342,
#51343,#51344,#51345,#51346,#51347,#51348,#51349,#51350,#51351,#51352,#51353,
#51354,#51355,#51356,#51357,#51358,#51359,#51360,#51361,#51362,#51363,#51364,
#51365,#51366,#51367,#51368,#51369,#51370,#51371,#51372,#51373,#51374,#51375,
#51376,#51377,#51378,#51379,#51380,#51381,#51382,#51383,#51384,#51385,#51386,
#51387,#51388,#51389,#51390,#51391,#51392,#51393,#51394,#51395,#51396,#51397,
#51398,#51399,#51400,#51401,#51402,#51403,#51404,#51405,#51406,#51407,#51408,
#51409,#51410,#51411,#51412,#51413,#51414,#51415,#51416,#51417,#51418,#51419,
#51420,#51421,#51422,#51423,#51424,#51425,#51426,#51427,#51428,#51429,#51430,
#51431,#51432,#51433,#51434,#51435,#51436,#51437,#51438,#51439,#51440,#51441,
#51442,#51443,#51444,#51445,#51446,#51447,#51448,#51449,#51450,#51451,#51452,
#51453,#51454,#51455,#51456,#51457,#51458,#51459,#51460,#51461,#51462,#51463,
#51464,#51465,#51466,#51467,#51468,#51469,#51470,#51471,#51472,#51473,#51474,
#51475,#51476,#51477,#51478,#51479,#51480,#51481,#51482,#51483,#51484,#51485,
#51486,#51487,#51488,#51489,#51490,#51491,#51492,#51493,#51494,#51495,#51496,
#51497,#51498,#51499,#51500,#51501,#51502,#51503,#51504,#51505,#51506,#51507,
#51508,#51509,#51510,#51511,#51512,#51513,#51514,#51515,#51516,#51517,#51518,
#51519,#51520,#51521,#51522,#51523,#51524,#51525,#51526,#51527,#51528,#51529,
#51530,#51531,#51532,#51533,#51534,#51535,#51536,#51537,#51538,#51539,#51540,
#51541,#51542,#51543,#51544,#51545,#51546,#51547,#51548,#51549,#51550,#51551,
#51552,#51553,#51554,#51555,#51556,#51557,#51558,#51559,#51560,#51561,#51562,
#51563,#51564,#51565,#51566,#51567,#51568,#51569,#51570,#51571,#51572,#51573,
#51574,#51575,#51576,#51577,#51578,#51579,#51580,#51581,#51582,#51583,#51584,
#51585,#51586,#51587,#51588,#51589,#51590,#51591,#51592,#51593,#51594,#51595,
#51596,#51597,#51598,#51599,#51600,#51601,#51602,#51603,#51604,#51605,#51606,
#51607,#51608,#51609,#51610,#51611,#51612,#51613,#51614,#51615,#51616,#51617,
#51618,#51619,#51620,#51621,#51622,#51623,#51624,#51625,#51626,#51627,#51628,
#51629,#51630,#51631,#51632,#51633,#51634,#51635,#51636,#51637,#51638,#51639,
#51640,#51641,#51642,#51643,#51644,#51645,#51646,#51647,#51648,#51649,#51650,
#51651),(#51652,#51653,#51654,#51655,#51656,#51657,#51658,#51659,#51660,
#51661,#51662,#51663,#51664,#51665,#51666,#51667,#51668,#51669,#51670,#51671,
#51672,#51673,#51674,#51675,#51676,#51677,#51678,#51679,#51680,#51681,#51682,
#51683,#51684,#51685,#51686,#51687,#51688,#51689,#51690,#51691,#51692,#51693,
#51694,#51695,#51696,#51697,#51698,#51699,#51700,#51701,#51702,#51703,#51704,
#51705,#51706,#51707,#51708,#51709,#51710,#51711,#51712,#51713,#51714,#51715,
#51716,#51717,#51718,#51719,#51720,#51721,#51722,#51723,#51724,#51725,#51726,
#51727,#51728,#51729,#51730,#51731,#51732,#51733,#51734,#51735,#51736,#51737,
#51738,#51739,#51740,#51741,#51742,#51743,#51744,#51745,#51746,#51747,#51748,
#51749,#51750,#51751,#51752,#51753,#51754,#51755,#51756,#51757,#51758,#51759,
#51760,#51761,#51762,#51763,#51764,#51765,#51766,#51767,#51768,#51769,#51770,
#51771,#51772,#51773,#51774,#51775,#51776,#51777,#51778,#51779,#51780,#51781,
#51782,#51783,#51784,#51785,#51786,#51787,#51788,#51789,#51790,#51791,#51792,
#51793,#51794,#51795,#51796,#51797,#51798,#51799,#51800,#51801,#51802,#51803,
#51804,#51805,#51806,#51807,#51808,#51809,#51810,#51811,#51812,#51813,#51814,
#51815,#51816,#51817,#51818,#51819,#51820,#51821,#51822,#51823,#51824,#51825,
#51826,#51827,#51828,#51829,#51830,#51831,#51832,#51833,#51834,#51835,#51836,
#51837,#51838,#51839,#51840,#51841,#51842,#51843,#51844,#51845,#51846,#51847,
#51848,#51849,#51850,#51851,#51852,#51853,#51854,#51855,#51856,#51857,#51858,
#51859,#51860,#51861,#51862,#51863,#51864,#51865,#51866,#51867,#51868,#51869,
#51870,#51871,#51872,#51873,#51874,#51875,#51876,#51877,#51878,#51879,#51880,
#51881,#51882,#51883,#51884,#51885,#51886,#51887,#51888,#51889,#51890,#51891,
#51892,#51893,#51894,#51895,#51896,#51897,#51898,#51899,#51900,#51901,#51902,
#51903,#51904,#51905,#51906,#51907,#51908,#51909,#51910,#51911,#51912,#51913,
#51914,#51915,#51916,#51917,#51918,#51919,#51920,#51921,#51922,#51923,#51924,
#51925,#51926,#51927,#51928,#51929,#51930,#51931,#51932,#51933,#51934,#51935,
#51936,#51937,#51938,#51939,#51940,#51941,#51942,#51943,#51944,#51945,#51946,
#51947,#51948,#51949,#51950,#51951,#51952,#51953,#51954,#51955,#51956,#51957,
#51958,#51959,#51960,#51961,#51962,#51963,#51964,#51965,#51966,#51967,#51968,
#51969,#51970,#51971,#51972,#51973,#51974,#51975,#51976,#51977,#51978,#51979,
#51980,#51981,#51982,#51983,#51984,#51985,#51986,#51987,#51988,#51989,#51990,
#51991,#51992,#51993,#51994,#51995,#51996,#51997,#51998,#51999,#52000,#52001,
#52002,#52003,#52004,#52005,#52006,#52007,#52008,#52009,#52010,#52011,#52012,
#52013,#52014,#52015,#52016,#52017,#52018,#52019,#52020),(#52021,#52022,
#52023,#52024,#52025,#52026,#52027,#52028,#52029,#52030,#52031,#52032,#52033,
#52034,#52035,#52036,#52037,#52038,#52039,#52040,#52041,#52042,#52043,#52044,
#52045,#52046,#52047,#52048,#52049,#52050,#52051,#52052,#52053,#52054,#52055,
#52056,#52057,#52058,#52059,#52060,#52061,#52062,#52063,#52064,#52065,#52066,
#52067,#52068,#52069,#52070,#52071,#52072,#52073,#52074,#52075,#52076,#52077,
#52078,#52079,#52080,#52081,#52082,#52083,#52084,#52085,#52086,#52087,#52088,
#52089,#52090,#52091,#52092,#52093,#52094,#52095,#52096,#52097,#52098,#52099,
#52100,#52101,#52102,#52103,#52104,#52105,#52106,#52107,#52108,#52109,#52110,
#52111,#52112,#52113,#52114,#52115,#52116,#52117,#52118,#52119,#52120,#52121,
#52122,#52123,#52124,#52125,#52126,#52127,#52128,#52129,#52130,#52131,#52132,
#52133,#52134,#52135,#52136,#52137,#52138,#52139,#52140,#52141,#52142,#52143,
#52144,#52145,#52146,#52147,#52148,#52149,#52150,#52151,#52152,#52153,#52154,
#52155,#52156,#52157,#52158,#52159,#52160,#52161,#52162,#52163,#52164,#52165,
#52166,#52167,#52168,#52169,#52170,#52171,#52172,#52173,#52174,#52175,#52176,
#52177,#52178,#52179,#52180,#52181,#52182,#52183,#52184,#52185,#52186,#52187,
#52188,#52189,#52190,#52191,#52192,#52193,#52194,#52195,#52196,#52197,#52198,
#52199,#52200,#52201,#52202,#52203,#52204,#52205,#52206,#52207,#52208,#52209,
#52210,#52211,#52212,#52213,#52214,#52215,#52216,#52217,#52218,#52219,#52220,
#52221,#52222,#52223,#52224,#52225,#52226,#52227,#52228,#52229,#52230,#52231,
#52232,#52233,#52234,#52235,#52236,#52237,#52238,#52239,#52240,#52241,#52242,
#52243,#52244,#52245,#52246,#52247,#52248,#52249,#52250,#52251,#52252,#52253,
#52254,#52255,#52256,#52257,#52258,#52259,#52260,#52261,#52262,#52263,#52264,
#52265,#52266,#52267,#52268,#52269,#52270,#52271,#52272,#52273,#52274,#52275,
#52276,#52277,#52278,#52279,#52280,#52281,#52282,#52283,#52284,#52285,#52286,
#52287,#52288,#52289,#52290,#52291,#52292,#52293,#52294,#52295,#52296,#52297,
#52298,#52299,#52300,#52301,#52302,#52303,#52304,#52305,#52306,#52307,#52308,
#52309,#52310,#52311,#52312,#52313,#52314,#52315,#52316,#52317,#52318,#52319,
#52320,#52321,#52322,#52323,#52324,#52325,#52326,#52327,#52328,#52329,#52330,
#52331,#52332,#52333,#52334,#52335,#52336,#52337,#52338,#52339,#52340,#52341,
#52342,#52343,#52344,#52345,#52346,#52347,#52348,#52349,#52350,#52351,#52352,
#52353,#52354,#52355,#52356,#52357,#52358,#52359,#52360,#52361,#52362,#52363,
#52364,#52365,#52366,#52367,#52368,#52369,#52370,#52371,#52372,#52373,#52374,
#52375,#52376,#52377,#52378,#52379,#52380,#52381,#52382,#52383,#52384,#52385,
#52386,#52387,#52388,#52389),(#52390,#52391,#52392,#52393,#52394,#52395,
#52396,#52397,#52398,#52399,#52400,#52401,#52402,#52403,#52404,#52405,#52406,
#52407,#52408,#52409,#52410,#52411,#52412,#52413,#52414,#52415,#52416,#52417,
#52418,#52419,#52420,#52421,#52422,#52423,#52424,#52425,#52426,#52427,#52428,
#52429,#52430,#52431,#52432,#52433,#52434,#52435,#52436,#52437,#52438,#52439,
#52440,#52441,#52442,#52443,#52444,#52445,#52446,#52447,#52448,#52449,#52450,
#52451,#52452,#52453,#52454,#52455,#52456,#52457,#52458,#52459,#52460,#52461,
#52462,#52463,#52464,#52465,#52466,#52467,#52468,#52469,#52470,#52471,#52472,
#52473,#52474,#52475,#52476,#52477,#52478,#52479,#52480,#52481,#52482,#52483,
#52484,#52485,#52486,#52487,#52488,#52489,#52490,#52491,#52492,#52493,#52494,
#52495,#52496,#52497,#52498,#52499,#52500,#52501,#52502,#52503,#52504,#52505,
#52506,#52507,#52508,#52509,#52510,#52511,#52512,#52513,#52514,#52515,#52516,
#52517,#52518,#52519,#52520,#52521,#52522,#52523,#52524,#52525,#52526,#52527,
#52528,#52529,#52530,#52531,#52532,#52533,#52534,#52535,#52536,#52537,#52538,
#52539,#52540,#52541,#52542,#52543,#52544,#52545,#52546,#52547,#52548,#52549,
#52550,#52551,#52552,#52553,#52554,#52555,#52556,#52557,#52558,#52559,#52560,
#52561,#52562,#52563,#52564,#52565,#52566,#52567,#52568,#52569,#52570,#52571,
#52572,#52573,#52574,#52575,#52576,#52577,#52578,#52579,#52580,#52581,#52582,
#52583,#52584,#52585,#52586,#52587,#52588,#52589,#52590,#52591,#52592,#52593,
#52594,#52595,#52596,#52597,#52598,#52599,#52600,#52601,#52602,#52603,#52604,
#52605,#52606,#52607,#52608,#52609,#52610,#52611,#52612,#52613,#52614,#52615,
#52616,#52617,#52618,#52619,#52620,#52621,#52622,#52623,#52624,#52625,#52626,
#52627,#52628,#52629,#52630,#52631,#52632,#52633,#52634,#52635,#52636,#52637,
#52638,#52639,#52640,#52641,#52642,#52643,#52644,#52645,#52646,#52647,#52648,
#52649,#52650,#52651,#52652,#52653,#52654,#52655,#52656,#52657,#52658,#52659,
#52660,#52661,#52662,#52663,#52664,#52665,#52666,#52667,#52668,#52669,#52670,
#52671,#52672,#52673,#52674,#52675,#52676,#52677,#52678,#52679,#52680,#52681,
#52682,#52683,#52684,#52685,#52686,#52687,#52688,#52689,#52690,#52691,#52692,
#52693,#52694,#52695,#52696,#52697,#52698,#52699,#52700,#52701,#52702,#52703,
#52704,#52705,#52706,#52707,#52708,#52709,#52710,#52711,#52712,#52713,#52714,
#52715,#52716,#52717,#52718,#52719,#52720,#52721,#52722,#52723,#52724,#52725,
#52726,#52727,#52728,#52729,#52730,#52731,#52732,#52733,#52734,#52735,#52736,
#52737,#52738,#52739,#52740,#52741,#52742,#52743,#52744,#52745,#52746,#52747,
#52748,#52749,#52750,#52751,#52752,#52753,#52754,#52755,#52756,#52757,#52758)),
 .UNSPECIFIED.,.F.,.F.,.F.,(4,4),(4,1,1,1,1,1,1,1,1,1,1,1,1,1,1,1,1,1,1,
1,1,1,1,1,1,1,1,1,1,1,1,1,1,1,1,1,1,1,1,1,1,1,1,1,1,1,1,1,1,1,1,1,1,1,1,
1,1,1,1,1,1,1,1,1,1,1,1,1,1,1,1,1,1,1,1,1,1,1,1,1,1,1,1,1,1,1,1,1,1,1,1,
1,1,1,1,1,1,1,1,1,1,1,1,1,1,1,1,1,1,1,1,1,1,1,1,1,1,1,1,1,1,1,1,1,1,1,1,
1,1,1,1,1,1,1,1,1,1,1,1,1,1,1,1,1,1,1,1,1,1,1,1,1,1,1,1,1,1,1,1,1,1,1,1,
1,1,1,1,1,1,1,1,1,1,1,1,1,1,1,1,1,1,1,1,1,1,1,1,1,1,1,1,1,1,1,1,1,1,1,1,
1,1,1,1,1,1,1,1,1,1,1,1,1,1,1,1,1,1,1,1,1,1,1,1,1,1,1,1,1,1,1,1,1,1,1,1,
1,1,1,1,1,1,1,1,1,1,1,1,1,1,1,1,1,1,1,1,1,1,1,1,1,1,1,1,1,1,1,1,1,1,1,1,
1,1,1,1,1,1,1,1,1,1,1,1,1,1,1,1,1,1,1,1,1,1,1,1,1,1,1,1,1,1,1,1,1,1,1,1,
1,1,1,1,1,1,1,1,1,1,1,1,1,1,1,1,1,1,1,1,1,1,1,1,1,1,1,1,1,1,1,1,1,1,1,1,
1,1,1,1,1,1,1,1,1,1,1,1,1,1,1,1,1,1,1,1,1,1,1,4),(0.,0.132097741590586),
(8.30112925462635,8.79930764192242,9.29748602921848,9.79566441651454,10.2938428038106,
10.7920211911067,11.2901995784027,11.7883779656988,12.2865563529949,12.7847347402909,
13.282913127587,13.781091514883,14.2792699021791,14.7774482894752,15.2756266767712,
15.7738050640673,16.2719834513634,16.7701618386594,17.2683402259555,17.7665186132516,
18.2646970005476,18.7628753878437,19.2610537751397,19.7592321624358,20.2574105497319,
20.7555889370279,21.253767324324,21.7519457116201,22.2501240989161,22.7483024862122,
23.2464808735082,23.7446592608043,24.2428376481004,24.7410160353964,25.2391944226925,
25.7373728099886,26.2355511972846,26.7337295845807,27.2319079718768,27.7300863591728,
28.2282647464689,28.7264431337649,29.224621521061,29.7227999083571,30.2209782956531,
30.7191566829492,31.2173350702453,31.7155134575413,32.2136918448374,32.7118702321334,
33.2100486194295,33.7082270067256,34.2064053940216,34.7045837813177,35.2027621686138,
35.7009405559098,36.1991189432059,36.697297330502,37.195475717798,37.6936541050941,
38.1918324923901,38.6900108796862,39.1881892669823,39.6863676542783,40.1845460415744,
40.6827244288705,41.1809028161665,41.6790812034626,42.1772595907587,42.6754379780547,
43.1736163653508,43.6717947526468,44.1699731399429,44.668151527239,45.166329914535,
45.6645083018311,46.1626866891272,46.6608650764232,47.1590434637193,47.6572218510153,
48.1554002383114,48.6535786256075,49.1517570129035,49.6499354001996,50.1481137874957,
50.6462921747917,51.1444705620878,51.6426489493839,52.1408273366799,52.639005723976,
53.137184111272,53.6353624985681,54.1335408858642,54.6317192731602,55.1298976604563,
55.6280760477524,56.1262544350484,56.6244328223445,57.1226112096405,57.6207895969366,
58.1189679842327,58.6171463715287,59.1153247588248,59.6135031461209,60.1116815334169,
60.609859920713,61.108038308009,61.6062166953051,62.1043950826012,62.6025734698972,
63.1007518571933,63.5989302444894,64.0971086317854,64.5952870190815,65.0934654063776,
65.5916437936736,66.0898221809697,66.5880005682658,67.0861789555618,67.5843573428579,
68.0825357301539,68.58071411745,69.0788925047461,69.5770708920421,70.0752492793382,
70.5734276666342,71.0716060539303,71.5697844412264,72.0679628285224,72.5661412158185,
73.0643196031146,73.5624979904106,74.0606763777067,74.5588547650028,75.0570331522988,
75.5552115395949,76.053389926891,76.551568314187,77.0497467014831,77.5479250887791,
78.0461034760752,78.5442818633713,79.0424602506673,79.5406386379634,80.0388170252594,
80.5369954125555,81.0351737998516,81.5333521871476,82.0315305744437,82.5297089617398,
83.0278873490358,83.5260657363319,84.024244123628,84.522422510924,85.0206008982201,
85.5187792855161,86.0169576728122,86.5151360601083,87.0133144474043,87.5114928347004,
88.0096712219965,88.5078496092925,89.0060279965886,89.5042063838847,90.0023847711807,
90.5005631584768,90.9987415457728,91.4969199330689,91.995098320365,92.493276707661,
92.9914550949571,93.4896334822532,93.9878118695492,94.4859902568453,94.9841686441413,
95.4823470314374,95.9805254187335,96.4787038060295,96.9768821933256,97.4750605806217,
97.9732389679177,98.4714173552138,98.9695957425099,99.4677741298059,99.965952517102,
100.464130904398,100.962309291694,101.46048767899,101.958666066286,102.456844453582,
102.955022840878,103.453201228174,103.95137961547,104.449558002767,104.947736390063,
105.445914777359,105.944093164655,106.442271551951,106.940449939247,107.438628326543,
107.936806713839,108.434985101135,108.933163488431,109.431341875727,109.929520263023,
110.427698650319,110.925877037615,111.424055424911,111.922233812207,112.420412199504,
112.9185905868,113.416768974096,113.914947361392,114.413125748688,114.911304135984,
115.40948252328,115.907660910576,116.405839297872,116.904017685168,117.402196072464,
117.90037445976,118.398552847056,118.896731234352,119.394909621648,119.893088008945,
120.391266396241,120.889444783537,121.387623170833,121.885801558129,122.383979945425,
122.882158332721,123.380336720017,123.878515107313,124.376693494609,124.874871881905,
125.373050269201,125.871228656497,126.369407043793,126.867585431089,127.365763818385,
127.863942205682,128.362120592978,128.860298980274,129.35847736757,129.856655754866,
130.354834142162,130.853012529458,131.351190916754,131.84936930405,132.347547691346,
132.845726078642,133.343904465938,133.842082853234,134.34026124053,134.838439627826,
135.336618015122,135.834796402419,136.332974789715,136.831153177011,137.329331564307,
137.827509951603,138.325688338899,138.823866726195,139.322045113491,139.820223500787,
140.318401888083,140.816580275379,141.314758662675,141.812937049971,142.311115437267,
142.809293824563,143.307472211859,143.805650599156,144.303828986452,144.802007373748,
145.300185761044,145.79836414834,146.296542535636,146.794720922932,147.292899310228,
147.791077697524,148.28925608482,148.787434472116,149.285612859412,149.783791246708,
150.281969634004,150.7801480213,151.278326408596,151.776504795893,152.274683183189,
152.772861570485,153.271039957781,153.769218345077,154.267396732373,154.765575119669,
155.263753506965,155.761931894261,156.260110281557,156.758288668853,157.256467056149,
157.754645443445,158.252823830741,158.751002218037,159.249180605333,159.74735899263,
160.245537379926,160.743715767222,161.241894154518,161.740072541814,162.23825092911,
162.736429316406,163.234607703702,163.732786090998,164.230964478294,164.72914286559,
165.227321252886,165.725499640182,166.223678027478,166.721856414774,167.220034802071,
167.718213189367,168.216391576663,168.714569963959,169.212748351255,169.710926738551,
170.209105125847,170.707283513143,171.205461900439,171.703640287735,172.201818675031,
172.699997062327,173.198175449623,173.696353836919,174.194532224215,174.692710611511,
175.190888998808,175.689067386104,176.1872457734,176.685424160696,177.183602547992,
177.681780935288,178.179959322584,178.67813770988,179.176316097176,179.674494484472,
180.172672871768,180.670851259064,181.16902964636,181.667208033656,182.165386420952,
182.663564808248,183.161743195545,183.659921582841,184.158099970137,184.656278357433,
185.154456744729,185.652635132025,186.150813519321,186.648991906617,187.147170293913,
187.645348681209,188.143527068505,188.641705455801,189.139883843097,189.638062230393,
190.136240617689,190.634419004985),.UNSPECIFIED.);
#277=B_SPLINE_SURFACE_WITH_KNOTS('',3,3,((#52964,#52965,#52966,#52967,#52968,
#52969,#52970,#52971,#52972,#52973,#52974,#52975,#52976,#52977,#52978,#52979,
#52980,#52981,#52982,#52983,#52984,#52985,#52986,#52987,#52988,#52989,#52990,
#52991,#52992,#52993,#52994,#52995,#52996,#52997,#52998,#52999,#53000,#53001,
#53002,#53003,#53004,#53005,#53006,#53007,#53008,#53009,#53010,#53011,#53012,
#53013,#53014,#53015,#53016,#53017,#53018,#53019,#53020,#53021,#53022,#53023,
#53024,#53025,#53026,#53027,#53028,#53029,#53030,#53031,#53032,#53033,#53034,
#53035,#53036,#53037,#53038,#53039,#53040,#53041,#53042,#53043,#53044,#53045,
#53046,#53047,#53048,#53049,#53050,#53051,#53052,#53053,#53054,#53055,#53056,
#53057,#53058,#53059,#53060,#53061,#53062,#53063,#53064,#53065,#53066,#53067,
#53068,#53069,#53070,#53071,#53072,#53073,#53074,#53075,#53076,#53077,#53078,
#53079,#53080,#53081,#53082,#53083,#53084,#53085,#53086,#53087,#53088,#53089,
#53090,#53091,#53092,#53093,#53094,#53095,#53096,#53097,#53098,#53099,#53100,
#53101,#53102,#53103,#53104,#53105,#53106,#53107,#53108,#53109,#53110,#53111,
#53112,#53113,#53114,#53115,#53116,#53117,#53118,#53119,#53120,#53121,#53122,
#53123,#53124,#53125,#53126,#53127,#53128,#53129,#53130,#53131,#53132,#53133,
#53134,#53135,#53136,#53137,#53138,#53139,#53140,#53141,#53142,#53143,#53144,
#53145,#53146,#53147,#53148,#53149,#53150,#53151,#53152,#53153,#53154,#53155,
#53156,#53157,#53158,#53159,#53160,#53161,#53162,#53163,#53164,#53165,#53166,
#53167,#53168,#53169,#53170,#53171,#53172,#53173,#53174,#53175,#53176,#53177,
#53178,#53179,#53180,#53181,#53182,#53183,#53184,#53185,#53186,#53187,#53188,
#53189,#53190,#53191,#53192,#53193,#53194,#53195,#53196,#53197,#53198,#53199,
#53200,#53201,#53202,#53203,#53204,#53205,#53206,#53207,#53208,#53209,#53210,
#53211,#53212,#53213,#53214,#53215,#53216,#53217,#53218,#53219,#53220,#53221,
#53222,#53223,#53224,#53225,#53226,#53227,#53228,#53229,#53230,#53231,#53232,
#53233,#53234,#53235,#53236,#53237,#53238,#53239,#53240,#53241,#53242,#53243,
#53244,#53245,#53246,#53247,#53248,#53249,#53250,#53251,#53252,#53253,#53254,
#53255,#53256,#53257,#53258,#53259,#53260,#53261,#53262,#53263,#53264,#53265,
#53266,#53267,#53268,#53269,#53270,#53271,#53272,#53273,#53274,#53275,#53276,
#53277,#53278,#53279,#53280,#53281,#53282,#53283,#53284,#53285,#53286,#53287,
#53288,#53289,#53290,#53291,#53292,#53293,#53294,#53295,#53296,#53297,#53298,
#53299,#53300,#53301,#53302,#53303,#53304,#53305,#53306,#53307,#53308,#53309,
#53310,#53311,#53312,#53313,#53314,#53315,#53316,#53317,#53318,#53319,#53320,
#53321,#53322,#53323,#53324,#53325,#53326,#53327,#53328,#53329,#53330,#53331,
#53332),(#53333,#53334,#53335,#53336,#53337,#53338,#53339,#53340,#53341,
#53342,#53343,#53344,#53345,#53346,#53347,#53348,#53349,#53350,#53351,#53352,
#53353,#53354,#53355,#53356,#53357,#53358,#53359,#53360,#53361,#53362,#53363,
#53364,#53365,#53366,#53367,#53368,#53369,#53370,#53371,#53372,#53373,#53374,
#53375,#53376,#53377,#53378,#53379,#53380,#53381,#53382,#53383,#53384,#53385,
#53386,#53387,#53388,#53389,#53390,#53391,#53392,#53393,#53394,#53395,#53396,
#53397,#53398,#53399,#53400,#53401,#53402,#53403,#53404,#53405,#53406,#53407,
#53408,#53409,#53410,#53411,#53412,#53413,#53414,#53415,#53416,#53417,#53418,
#53419,#53420,#53421,#53422,#53423,#53424,#53425,#53426,#53427,#53428,#53429,
#53430,#53431,#53432,#53433,#53434,#53435,#53436,#53437,#53438,#53439,#53440,
#53441,#53442,#53443,#53444,#53445,#53446,#53447,#53448,#53449,#53450,#53451,
#53452,#53453,#53454,#53455,#53456,#53457,#53458,#53459,#53460,#53461,#53462,
#53463,#53464,#53465,#53466,#53467,#53468,#53469,#53470,#53471,#53472,#53473,
#53474,#53475,#53476,#53477,#53478,#53479,#53480,#53481,#53482,#53483,#53484,
#53485,#53486,#53487,#53488,#53489,#53490,#53491,#53492,#53493,#53494,#53495,
#53496,#53497,#53498,#53499,#53500,#53501,#53502,#53503,#53504,#53505,#53506,
#53507,#53508,#53509,#53510,#53511,#53512,#53513,#53514,#53515,#53516,#53517,
#53518,#53519,#53520,#53521,#53522,#53523,#53524,#53525,#53526,#53527,#53528,
#53529,#53530,#53531,#53532,#53533,#53534,#53535,#53536,#53537,#53538,#53539,
#53540,#53541,#53542,#53543,#53544,#53545,#53546,#53547,#53548,#53549,#53550,
#53551,#53552,#53553,#53554,#53555,#53556,#53557,#53558,#53559,#53560,#53561,
#53562,#53563,#53564,#53565,#53566,#53567,#53568,#53569,#53570,#53571,#53572,
#53573,#53574,#53575,#53576,#53577,#53578,#53579,#53580,#53581,#53582,#53583,
#53584,#53585,#53586,#53587,#53588,#53589,#53590,#53591,#53592,#53593,#53594,
#53595,#53596,#53597,#53598,#53599,#53600,#53601,#53602,#53603,#53604,#53605,
#53606,#53607,#53608,#53609,#53610,#53611,#53612,#53613,#53614,#53615,#53616,
#53617,#53618,#53619,#53620,#53621,#53622,#53623,#53624,#53625,#53626,#53627,
#53628,#53629,#53630,#53631,#53632,#53633,#53634,#53635,#53636,#53637,#53638,
#53639,#53640,#53641,#53642,#53643,#53644,#53645,#53646,#53647,#53648,#53649,
#53650,#53651,#53652,#53653,#53654,#53655,#53656,#53657,#53658,#53659,#53660,
#53661,#53662,#53663,#53664,#53665,#53666,#53667,#53668,#53669,#53670,#53671,
#53672,#53673,#53674,#53675,#53676,#53677,#53678,#53679,#53680,#53681,#53682,
#53683,#53684,#53685,#53686,#53687,#53688,#53689,#53690,#53691,#53692,#53693,
#53694,#53695,#53696,#53697,#53698,#53699,#53700,#53701),(#53702,#53703,
#53704,#53705,#53706,#53707,#53708,#53709,#53710,#53711,#53712,#53713,#53714,
#53715,#53716,#53717,#53718,#53719,#53720,#53721,#53722,#53723,#53724,#53725,
#53726,#53727,#53728,#53729,#53730,#53731,#53732,#53733,#53734,#53735,#53736,
#53737,#53738,#53739,#53740,#53741,#53742,#53743,#53744,#53745,#53746,#53747,
#53748,#53749,#53750,#53751,#53752,#53753,#53754,#53755,#53756,#53757,#53758,
#53759,#53760,#53761,#53762,#53763,#53764,#53765,#53766,#53767,#53768,#53769,
#53770,#53771,#53772,#53773,#53774,#53775,#53776,#53777,#53778,#53779,#53780,
#53781,#53782,#53783,#53784,#53785,#53786,#53787,#53788,#53789,#53790,#53791,
#53792,#53793,#53794,#53795,#53796,#53797,#53798,#53799,#53800,#53801,#53802,
#53803,#53804,#53805,#53806,#53807,#53808,#53809,#53810,#53811,#53812,#53813,
#53814,#53815,#53816,#53817,#53818,#53819,#53820,#53821,#53822,#53823,#53824,
#53825,#53826,#53827,#53828,#53829,#53830,#53831,#53832,#53833,#53834,#53835,
#53836,#53837,#53838,#53839,#53840,#53841,#53842,#53843,#53844,#53845,#53846,
#53847,#53848,#53849,#53850,#53851,#53852,#53853,#53854,#53855,#53856,#53857,
#53858,#53859,#53860,#53861,#53862,#53863,#53864,#53865,#53866,#53867,#53868,
#53869,#53870,#53871,#53872,#53873,#53874,#53875,#53876,#53877,#53878,#53879,
#53880,#53881,#53882,#53883,#53884,#53885,#53886,#53887,#53888,#53889,#53890,
#53891,#53892,#53893,#53894,#53895,#53896,#53897,#53898,#53899,#53900,#53901,
#53902,#53903,#53904,#53905,#53906,#53907,#53908,#53909,#53910,#53911,#53912,
#53913,#53914,#53915,#53916,#53917,#53918,#53919,#53920,#53921,#53922,#53923,
#53924,#53925,#53926,#53927,#53928,#53929,#53930,#53931,#53932,#53933,#53934,
#53935,#53936,#53937,#53938,#53939,#53940,#53941,#53942,#53943,#53944,#53945,
#53946,#53947,#53948,#53949,#53950,#53951,#53952,#53953,#53954,#53955,#53956,
#53957,#53958,#53959,#53960,#53961,#53962,#53963,#53964,#53965,#53966,#53967,
#53968,#53969,#53970,#53971,#53972,#53973,#53974,#53975,#53976,#53977,#53978,
#53979,#53980,#53981,#53982,#53983,#53984,#53985,#53986,#53987,#53988,#53989,
#53990,#53991,#53992,#53993,#53994,#53995,#53996,#53997,#53998,#53999,#54000,
#54001,#54002,#54003,#54004,#54005,#54006,#54007,#54008,#54009,#54010,#54011,
#54012,#54013,#54014,#54015,#54016,#54017,#54018,#54019,#54020,#54021,#54022,
#54023,#54024,#54025,#54026,#54027,#54028,#54029,#54030,#54031,#54032,#54033,
#54034,#54035,#54036,#54037,#54038,#54039,#54040,#54041,#54042,#54043,#54044,
#54045,#54046,#54047,#54048,#54049,#54050,#54051,#54052,#54053,#54054,#54055,
#54056,#54057,#54058,#54059,#54060,#54061,#54062,#54063,#54064,#54065,#54066,
#54067,#54068,#54069,#54070),(#54071,#54072,#54073,#54074,#54075,#54076,
#54077,#54078,#54079,#54080,#54081,#54082,#54083,#54084,#54085,#54086,#54087,
#54088,#54089,#54090,#54091,#54092,#54093,#54094,#54095,#54096,#54097,#54098,
#54099,#54100,#54101,#54102,#54103,#54104,#54105,#54106,#54107,#54108,#54109,
#54110,#54111,#54112,#54113,#54114,#54115,#54116,#54117,#54118,#54119,#54120,
#54121,#54122,#54123,#54124,#54125,#54126,#54127,#54128,#54129,#54130,#54131,
#54132,#54133,#54134,#54135,#54136,#54137,#54138,#54139,#54140,#54141,#54142,
#54143,#54144,#54145,#54146,#54147,#54148,#54149,#54150,#54151,#54152,#54153,
#54154,#54155,#54156,#54157,#54158,#54159,#54160,#54161,#54162,#54163,#54164,
#54165,#54166,#54167,#54168,#54169,#54170,#54171,#54172,#54173,#54174,#54175,
#54176,#54177,#54178,#54179,#54180,#54181,#54182,#54183,#54184,#54185,#54186,
#54187,#54188,#54189,#54190,#54191,#54192,#54193,#54194,#54195,#54196,#54197,
#54198,#54199,#54200,#54201,#54202,#54203,#54204,#54205,#54206,#54207,#54208,
#54209,#54210,#54211,#54212,#54213,#54214,#54215,#54216,#54217,#54218,#54219,
#54220,#54221,#54222,#54223,#54224,#54225,#54226,#54227,#54228,#54229,#54230,
#54231,#54232,#54233,#54234,#54235,#54236,#54237,#54238,#54239,#54240,#54241,
#54242,#54243,#54244,#54245,#54246,#54247,#54248,#54249,#54250,#54251,#54252,
#54253,#54254,#54255,#54256,#54257,#54258,#54259,#54260,#54261,#54262,#54263,
#54264,#54265,#54266,#54267,#54268,#54269,#54270,#54271,#54272,#54273,#54274,
#54275,#54276,#54277,#54278,#54279,#54280,#54281,#54282,#54283,#54284,#54285,
#54286,#54287,#54288,#54289,#54290,#54291,#54292,#54293,#54294,#54295,#54296,
#54297,#54298,#54299,#54300,#54301,#54302,#54303,#54304,#54305,#54306,#54307,
#54308,#54309,#54310,#54311,#54312,#54313,#54314,#54315,#54316,#54317,#54318,
#54319,#54320,#54321,#54322,#54323,#54324,#54325,#54326,#54327,#54328,#54329,
#54330,#54331,#54332,#54333,#54334,#54335,#54336,#54337,#54338,#54339,#54340,
#54341,#54342,#54343,#54344,#54345,#54346,#54347,#54348,#54349,#54350,#54351,
#54352,#54353,#54354,#54355,#54356,#54357,#54358,#54359,#54360,#54361,#54362,
#54363,#54364,#54365,#54366,#54367,#54368,#54369,#54370,#54371,#54372,#54373,
#54374,#54375,#54376,#54377,#54378,#54379,#54380,#54381,#54382,#54383,#54384,
#54385,#54386,#54387,#54388,#54389,#54390,#54391,#54392,#54393,#54394,#54395,
#54396,#54397,#54398,#54399,#54400,#54401,#54402,#54403,#54404,#54405,#54406,
#54407,#54408,#54409,#54410,#54411,#54412,#54413,#54414,#54415,#54416,#54417,
#54418,#54419,#54420,#54421,#54422,#54423,#54424,#54425,#54426,#54427,#54428,
#54429,#54430,#54431,#54432,#54433,#54434,#54435,#54436,#54437,#54438,#54439)),
 .UNSPECIFIED.,.F.,.F.,.F.,(4,4),(4,1,1,1,1,1,1,1,1,1,1,1,1,1,1,1,1,1,1,
1,1,1,1,1,1,1,1,1,1,1,1,1,1,1,1,1,1,1,1,1,1,1,1,1,1,1,1,1,1,1,1,1,1,1,1,
1,1,1,1,1,1,1,1,1,1,1,1,1,1,1,1,1,1,1,1,1,1,1,1,1,1,1,1,1,1,1,1,1,1,1,1,
1,1,1,1,1,1,1,1,1,1,1,1,1,1,1,1,1,1,1,1,1,1,1,1,1,1,1,1,1,1,1,1,1,1,1,1,
1,1,1,1,1,1,1,1,1,1,1,1,1,1,1,1,1,1,1,1,1,1,1,1,1,1,1,1,1,1,1,1,1,1,1,1,
1,1,1,1,1,1,1,1,1,1,1,1,1,1,1,1,1,1,1,1,1,1,1,1,1,1,1,1,1,1,1,1,1,1,1,1,
1,1,1,1,1,1,1,1,1,1,1,1,1,1,1,1,1,1,1,1,1,1,1,1,1,1,1,1,1,1,1,1,1,1,1,1,
1,1,1,1,1,1,1,1,1,1,1,1,1,1,1,1,1,1,1,1,1,1,1,1,1,1,1,1,1,1,1,1,1,1,1,1,
1,1,1,1,1,1,1,1,1,1,1,1,1,1,1,1,1,1,1,1,1,1,1,1,1,1,1,1,1,1,1,1,1,1,1,1,
1,1,1,1,1,1,1,1,1,1,1,1,1,1,1,1,1,1,1,1,1,1,1,1,1,1,1,1,1,1,1,1,1,1,1,1,
1,1,1,1,1,1,1,1,1,1,1,1,1,1,1,1,1,1,1,1,1,1,1,4),(0.,0.132097741590586),
(11.6150328478184,12.1132112351144,12.6113896224105,13.1095680097066,13.6077463970026,
14.1059247842987,14.6041031715948,15.1022815588908,15.6004599461869,16.0986383334829,
16.596816720779,17.0949951080751,17.5931734953711,18.0913518826672,18.5895302699633,
19.0877086572593,19.5858870445554,20.0840654318515,20.5822438191475,21.0804222064436,
21.5786005937396,22.0767789810357,22.5749573683318,23.0731357556278,23.5713141429239,
24.06949253022,24.567670917516,25.0658493048121,25.5640276921081,26.0622060794042,
26.5603844667003,27.0585628539963,27.5567412412924,28.0549196285885,28.5530980158845,
29.0512764031806,29.5494547904767,30.0476331777727,30.5458115650688,31.0439899523648,
31.5421683396609,32.040346726957,32.538525114253,33.0367035015491,33.5348818888452,
34.0330602761412,34.5312386634373,35.0294170507333,35.5275954380294,36.0257738253255,
36.5239522126215,37.0221305999176,37.5203089872137,38.0184873745097,38.5166657618058,
39.0148441491019,39.5130225363979,40.011200923694,40.50937931099,41.0075576982861,
41.5057360855822,42.0039144728782,42.5020928601743,43.0002712474704,43.4984496347664,
43.9966280220625,44.4948064093585,44.9929847966546,45.4911631839507,45.9893415712467,
46.4875199585428,46.9856983458389,47.4838767331349,47.982055120431,48.480233507727,
48.9784118950231,49.4765902823192,49.9747686696152,50.4729470569113,50.9711254442074,
51.4693038315034,51.9674822187995,52.4656606060956,52.9638389933916,53.4620173806877,
53.9601957679837,54.4583741552798,54.9565525425759,55.4547309298719,55.952909317168,
56.4510877044641,56.9492660917601,57.4474444790562,57.9456228663523,58.4438012536483,
58.9419796409444,59.4401580282404,59.9383364155365,60.4365148028326,60.9346931901286,
61.4328715774247,61.9310499647208,62.4292283520168,62.9274067393129,63.425585126609,
63.923763513905,64.4219419012011,64.9201202884971,65.4182986757932,65.9164770630893,
66.4146554503853,66.9128338376814,67.4110122249775,67.9091906122735,68.4073689995696,
68.9055473868656,69.4037257741617,69.9019041614578,70.4000825487538,70.8982609360499,
71.396439323346,71.894617710642,72.3927960979381,72.8909744852342,73.3891528725302,
73.8873312598263,74.3855096471223,74.8836880344184,75.3818664217145,75.8800448090105,
76.3782231963066,76.8764015836027,77.3745799708987,77.8727583581948,78.3709367454909,
78.8691151327869,79.367293520083,79.865471907379,80.3636502946751,80.8618286819712,
81.3600070692672,81.8581854565633,82.3563638438594,82.8545422311554,83.3527206184515,
83.8508990057476,84.3490773930436,84.8472557803397,85.3454341676357,85.8436125549318,
86.3417909422279,86.8399693295239,87.33814771682,87.8363261041161,88.3345044914121,
88.8326828787082,89.3308612660042,89.8290396533003,90.3272180405964,90.8253964278924,
91.3235748151885,91.8217532024846,92.3199315897806,92.8181099770767,93.3162883643727,
93.8144667516688,94.3126451389649,94.8108235262609,95.309001913557,95.8071803008531,
96.3053586881491,96.8035370754452,97.3017154627413,97.7998938500373,98.2980722373334,
98.7962506246294,99.2944290119255,99.7926073992216,100.290785786518,100.788964173814,
101.28714256111,101.785320948406,102.283499335702,102.781677722998,103.279856110294,
103.77803449759,104.276212884886,104.774391272182,105.272569659478,105.770748046774,
106.26892643407,106.767104821366,107.265283208663,107.763461595959,108.261639983255,
108.759818370551,109.257996757847,109.756175145143,110.254353532439,110.752531919735,
111.250710307031,111.748888694327,112.247067081623,112.745245468919,113.243423856215,
113.741602243511,114.239780630807,114.737959018103,115.2361374054,115.734315792696,
116.232494179992,116.730672567288,117.228850954584,117.72702934188,118.225207729176,
118.723386116472,119.221564503768,119.719742891064,120.21792127836,120.716099665656,
121.214278052952,121.712456440248,122.210634827544,122.70881321484,123.206991602137,
123.705169989433,124.203348376729,124.701526764025,125.199705151321,125.697883538617,
126.196061925913,126.694240313209,127.192418700505,127.690597087801,128.188775475097,
128.686953862393,129.185132249689,129.683310636985,130.181489024281,130.679667411577,
131.177845798874,131.67602418617,132.174202573466,132.672380960762,133.170559348058,
133.668737735354,134.16691612265,134.665094509946,135.163272897242,135.661451284538,
136.159629671834,136.65780805913,137.155986446426,137.654164833722,138.152343221018,
138.650521608314,139.148699995611,139.646878382907,140.145056770203,140.643235157499,
141.141413544795,141.639591932091,142.137770319387,142.635948706683,143.134127093979,
143.632305481275,144.130483868571,144.628662255867,145.126840643163,145.625019030459,
146.123197417755,146.621375805052,147.119554192348,147.617732579644,148.11591096694,
148.614089354236,149.112267741532,149.610446128828,150.108624516124,150.60680290342,
151.104981290716,151.603159678012,152.101338065308,152.599516452604,153.0976948399,
153.595873227196,154.094051614492,154.592230001789,155.090408389085,155.588586776381,
156.086765163677,156.584943550973,157.083121938269,157.581300325565,158.079478712861,
158.577657100157,159.075835487453,159.574013874749,160.072192262045,160.570370649341,
161.068549036637,161.566727423933,162.064905811229,162.563084198526,163.061262585822,
163.559440973118,164.057619360414,164.55579774771,165.053976135006,165.552154522302,
166.050332909598,166.548511296894,167.04668968419,167.544868071486,168.043046458782,
168.541224846078,169.039403233374,169.53758162067,170.035760007966,170.533938395263,
171.032116782559,171.530295169855,172.028473557151,172.526651944447,173.024830331743,
173.523008719039,174.021187106335,174.519365493631,175.017543880927,175.515722268223,
176.013900655519,176.512079042815,177.010257430111,177.508435817407,178.006614204703,
178.504792592,179.002970979296,179.501149366592,179.999327753888,180.497506141184,
180.99568452848,181.493862915776,181.992041303072,182.490219690368,182.988398077664,
183.48657646496,183.984754852256,184.482933239552,184.981111626848,185.479290014144,
185.97746840144,186.475646788737,186.973825176033,187.472003563329,187.970181950625,
188.468360337921,188.966538725217,189.464717112513,189.962895499809,190.461073887105,
190.959252274401,191.457430661697,191.955609048993,192.453787436289,192.951965823585,
193.450144210881,193.948322598177),.UNSPECIFIED.);
#278=B_SPLINE_SURFACE_WITH_KNOTS('',3,3,((#57157,#57158,#57159,#57160,#57161,
#57162,#57163,#57164,#57165,#57166,#57167,#57168,#57169,#57170,#57171,#57172,
#57173,#57174,#57175,#57176,#57177,#57178,#57179,#57180,#57181,#57182,#57183,
#57184,#57185,#57186,#57187,#57188,#57189,#57190,#57191,#57192,#57193,#57194,
#57195,#57196,#57197,#57198,#57199,#57200,#57201,#57202,#57203,#57204,#57205,
#57206,#57207,#57208,#57209,#57210,#57211,#57212,#57213,#57214,#57215,#57216,
#57217,#57218,#57219,#57220,#57221,#57222,#57223,#57224,#57225,#57226,#57227,
#57228,#57229,#57230,#57231,#57232,#57233,#57234,#57235,#57236,#57237,#57238,
#57239,#57240,#57241,#57242,#57243,#57244,#57245,#57246,#57247,#57248,#57249,
#57250,#57251,#57252,#57253,#57254,#57255,#57256,#57257,#57258,#57259,#57260,
#57261,#57262,#57263,#57264,#57265,#57266,#57267,#57268,#57269,#57270,#57271,
#57272,#57273,#57274,#57275,#57276,#57277,#57278,#57279,#57280,#57281,#57282,
#57283,#57284,#57285,#57286,#57287,#57288,#57289,#57290,#57291,#57292,#57293,
#57294,#57295,#57296,#57297,#57298,#57299,#57300,#57301,#57302,#57303,#57304,
#57305,#57306,#57307,#57308,#57309,#57310,#57311,#57312,#57313,#57314,#57315,
#57316,#57317,#57318,#57319,#57320,#57321,#57322,#57323,#57324,#57325,#57326,
#57327,#57328,#57329,#57330,#57331,#57332,#57333,#57334,#57335,#57336,#57337,
#57338,#57339,#57340,#57341,#57342,#57343,#57344,#57345,#57346,#57347,#57348,
#57349,#57350,#57351,#57352,#57353,#57354,#57355,#57356,#57357,#57358,#57359,
#57360,#57361,#57362,#57363,#57364,#57365,#57366,#57367,#57368,#57369,#57370,
#57371,#57372,#57373,#57374,#57375,#57376,#57377,#57378,#57379,#57380,#57381,
#57382,#57383,#57384,#57385,#57386,#57387,#57388,#57389,#57390,#57391,#57392,
#57393,#57394,#57395,#57396,#57397,#57398,#57399),(#57400,#57401,#57402,
#57403,#57404,#57405,#57406,#57407,#57408,#57409,#57410,#57411,#57412,#57413,
#57414,#57415,#57416,#57417,#57418,#57419,#57420,#57421,#57422,#57423,#57424,
#57425,#57426,#57427,#57428,#57429,#57430,#57431,#57432,#57433,#57434,#57435,
#57436,#57437,#57438,#57439,#57440,#57441,#57442,#57443,#57444,#57445,#57446,
#57447,#57448,#57449,#57450,#57451,#57452,#57453,#57454,#57455,#57456,#57457,
#57458,#57459,#57460,#57461,#57462,#57463,#57464,#57465,#57466,#57467,#57468,
#57469,#57470,#57471,#57472,#57473,#57474,#57475,#57476,#57477,#57478,#57479,
#57480,#57481,#57482,#57483,#57484,#57485,#57486,#57487,#57488,#57489,#57490,
#57491,#57492,#57493,#57494,#57495,#57496,#57497,#57498,#57499,#57500,#57501,
#57502,#57503,#57504,#57505,#57506,#57507,#57508,#57509,#57510,#57511,#57512,
#57513,#57514,#57515,#57516,#57517,#57518,#57519,#57520,#57521,#57522,#57523,
#57524,#57525,#57526,#57527,#57528,#57529,#57530,#57531,#57532,#57533,#57534,
#57535,#57536,#57537,#57538,#57539,#57540,#57541,#57542,#57543,#57544,#57545,
#57546,#57547,#57548,#57549,#57550,#57551,#57552,#57553,#57554,#57555,#57556,
#57557,#57558,#57559,#57560,#57561,#57562,#57563,#57564,#57565,#57566,#57567,
#57568,#57569,#57570,#57571,#57572,#57573,#57574,#57575,#57576,#57577,#57578,
#57579,#57580,#57581,#57582,#57583,#57584,#57585,#57586,#57587,#57588,#57589,
#57590,#57591,#57592,#57593,#57594,#57595,#57596,#57597,#57598,#57599,#57600,
#57601,#57602,#57603,#57604,#57605,#57606,#57607,#57608,#57609,#57610,#57611,
#57612,#57613,#57614,#57615,#57616,#57617,#57618,#57619,#57620,#57621,#57622,
#57623,#57624,#57625,#57626,#57627,#57628,#57629,#57630,#57631,#57632,#57633,
#57634,#57635,#57636,#57637,#57638,#57639,#57640,#57641,#57642),(#57643,
#57644,#57645,#57646,#57647,#57648,#57649,#57650,#57651,#57652,#57653,#57654,
#57655,#57656,#57657,#57658,#57659,#57660,#57661,#57662,#57663,#57664,#57665,
#57666,#57667,#57668,#57669,#57670,#57671,#57672,#57673,#57674,#57675,#57676,
#57677,#57678,#57679,#57680,#57681,#57682,#57683,#57684,#57685,#57686,#57687,
#57688,#57689,#57690,#57691,#57692,#57693,#57694,#57695,#57696,#57697,#57698,
#57699,#57700,#57701,#57702,#57703,#57704,#57705,#57706,#57707,#57708,#57709,
#57710,#57711,#57712,#57713,#57714,#57715,#57716,#57717,#57718,#57719,#57720,
#57721,#57722,#57723,#57724,#57725,#57726,#57727,#57728,#57729,#57730,#57731,
#57732,#57733,#57734,#57735,#57736,#57737,#57738,#57739,#57740,#57741,#57742,
#57743,#57744,#57745,#57746,#57747,#57748,#57749,#57750,#57751,#57752,#57753,
#57754,#57755,#57756,#57757,#57758,#57759,#57760,#57761,#57762,#57763,#57764,
#57765,#57766,#57767,#57768,#57769,#57770,#57771,#57772,#57773,#57774,#57775,
#57776,#57777,#57778,#57779,#57780,#57781,#57782,#57783,#57784,#57785,#57786,
#57787,#57788,#57789,#57790,#57791,#57792,#57793,#57794,#57795,#57796,#57797,
#57798,#57799,#57800,#57801,#57802,#57803,#57804,#57805,#57806,#57807,#57808,
#57809,#57810,#57811,#57812,#57813,#57814,#57815,#57816,#57817,#57818,#57819,
#57820,#57821,#57822,#57823,#57824,#57825,#57826,#57827,#57828,#57829,#57830,
#57831,#57832,#57833,#57834,#57835,#57836,#57837,#57838,#57839,#57840,#57841,
#57842,#57843,#57844,#57845,#57846,#57847,#57848,#57849,#57850,#57851,#57852,
#57853,#57854,#57855,#57856,#57857,#57858,#57859,#57860,#57861,#57862,#57863,
#57864,#57865,#57866,#57867,#57868,#57869,#57870,#57871,#57872,#57873,#57874,
#57875,#57876,#57877,#57878,#57879,#57880,#57881,#57882,#57883,#57884,#57885),
(#57886,#57887,#57888,#57889,#57890,#57891,#57892,#57893,#57894,#57895,
#57896,#57897,#57898,#57899,#57900,#57901,#57902,#57903,#57904,#57905,#57906,
#57907,#57908,#57909,#57910,#57911,#57912,#57913,#57914,#57915,#57916,#57917,
#57918,#57919,#57920,#57921,#57922,#57923,#57924,#57925,#57926,#57927,#57928,
#57929,#57930,#57931,#57932,#57933,#57934,#57935,#57936,#57937,#57938,#57939,
#57940,#57941,#57942,#57943,#57944,#57945,#57946,#57947,#57948,#57949,#57950,
#57951,#57952,#57953,#57954,#57955,#57956,#57957,#57958,#57959,#57960,#57961,
#57962,#57963,#57964,#57965,#57966,#57967,#57968,#57969,#57970,#57971,#57972,
#57973,#57974,#57975,#57976,#57977,#57978,#57979,#57980,#57981,#57982,#57983,
#57984,#57985,#57986,#57987,#57988,#57989,#57990,#57991,#57992,#57993,#57994,
#57995,#57996,#57997,#57998,#57999,#58000,#58001,#58002,#58003,#58004,#58005,
#58006,#58007,#58008,#58009,#58010,#58011,#58012,#58013,#58014,#58015,#58016,
#58017,#58018,#58019,#58020,#58021,#58022,#58023,#58024,#58025,#58026,#58027,
#58028,#58029,#58030,#58031,#58032,#58033,#58034,#58035,#58036,#58037,#58038,
#58039,#58040,#58041,#58042,#58043,#58044,#58045,#58046,#58047,#58048,#58049,
#58050,#58051,#58052,#58053,#58054,#58055,#58056,#58057,#58058,#58059,#58060,
#58061,#58062,#58063,#58064,#58065,#58066,#58067,#58068,#58069,#58070,#58071,
#58072,#58073,#58074,#58075,#58076,#58077,#58078,#58079,#58080,#58081,#58082,
#58083,#58084,#58085,#58086,#58087,#58088,#58089,#58090,#58091,#58092,#58093,
#58094,#58095,#58096,#58097,#58098,#58099,#58100,#58101,#58102,#58103,#58104,
#58105,#58106,#58107,#58108,#58109,#58110,#58111,#58112,#58113,#58114,#58115,
#58116,#58117,#58118,#58119,#58120,#58121,#58122,#58123,#58124,#58125,#58126,
#58127,#58128)),.UNSPECIFIED.,.F.,.F.,.F.,(4,4),(4,1,1,1,1,1,1,1,1,1,1,
1,1,1,1,1,1,1,1,1,1,1,1,1,1,1,1,1,1,1,1,1,1,1,1,1,1,1,1,1,1,1,1,1,1,1,1,
1,1,1,1,1,1,1,1,1,1,1,1,1,1,1,1,1,1,1,1,1,1,1,1,1,1,1,1,1,1,1,1,1,1,1,1,
1,1,1,1,1,1,1,1,1,1,1,1,1,1,1,1,1,1,1,1,1,1,1,1,1,1,1,1,1,1,1,1,1,1,1,1,
1,1,1,1,1,1,1,1,1,1,1,1,1,1,1,1,1,1,1,1,1,1,1,1,1,1,1,1,1,1,1,1,1,1,1,1,
1,1,1,1,1,1,1,1,1,1,1,1,1,1,1,1,1,1,1,1,1,1,1,1,1,1,1,1,1,1,1,1,1,1,1,1,
1,1,1,1,1,1,1,1,1,1,1,1,1,1,1,1,1,1,1,1,1,1,1,1,1,1,1,1,1,1,1,1,1,1,1,1,
1,1,1,1,1,1,1,1,1,1,1,1,1,4),(0.,0.132097741590586),(8.30112925462614,8.79905190745349,
9.29697456028084,9.79489721310818,10.2928198659355,10.7907425187629,11.2886651715902,
11.7865878244176,12.2845104772449,12.7824331300723,13.2803557828996,13.778278435727,
14.2762010885543,14.7741237413817,15.272046394209,15.7699690470363,16.2678916998637,
16.765814352691,17.2637370055184,17.7616596583457,18.2595823111731,18.7575049640004,
19.2554276168278,19.7533502696551,20.2512729224825,20.7491955753098,21.2471182281372,
21.7450408809645,22.2429635337919,22.7408861866192,23.2388088394466,23.7367314922739,
24.2346541451012,24.7325767979286,25.2304994507559,25.7284221035833,26.2263447564106,
26.724267409238,27.2221900620653,27.7201127148927,28.21803536772,28.7159580205474,
29.2138806733747,29.7118033262021,30.2097259790294,30.7076486318568,31.2055712846841,
31.7034939375114,32.2014165903388,32.6993392431661,33.1972618959935,33.6951845488208,
34.1931072016482,34.6910298544755,35.1889525073029,35.6868751601302,36.1847978129576,
36.6827204657849,37.1806431186123,37.6785657714396,38.176488424267,38.6744110770943,
39.1723337299217,39.670256382749,40.1681790355763,40.6661016884037,41.164024341231,
41.6619469940584,42.1598696468857,42.6577922997131,43.1557149525404,43.6536376053678,
44.1515602581951,44.6494829110225,45.1474055638498,45.6453282166772,46.1432508695045,
46.6411735223319,47.1390961751592,47.6370188279866,48.1349414808139,48.6328641336412,
49.1307867864686,49.6287094392959,50.1266320921233,50.6245547449506,51.122477397778,
51.6204000506053,52.1183227034327,52.61624535626,53.1141680090874,53.6120906619147,
54.1100133147421,54.6079359675694,55.1058586203968,55.6037812732241,56.1017039260515,
56.5996265788788,57.0975492317061,57.5954718845335,58.0933945373608,58.5913171901882,
59.0892398430155,59.5871624958429,60.0850851486702,60.5830078014976,61.0809304543249,
61.5788531071523,62.0767757599796,62.574698412807,63.0726210656343,63.5705437184617,
64.068466371289,64.5663890241163,65.0643116769437,65.562234329771,66.0601569825984,
66.5580796354257,67.0560022882531,67.5539249410804,68.0518475939078,68.5497702467351,
69.0476928995625,69.5456155523898,70.0435382052172,70.5414608580445,71.0393835108719,
71.5373061636992,72.0352288165266,72.5331514693539,73.0310741221813,73.5289967750086,
74.0269194278359,74.5248420806633,75.0227647334906,75.520687386318,76.0186100391453,
76.5165326919727,77.0144553448,77.5123779976274,78.0103006504547,78.5082233032821,
79.0061459561094,79.5040686089368,80.0019912617641,80.4999139145914,80.9978365674188,
81.4957592202462,81.9936818730735,82.4916045259008,82.9895271787282,83.4874498315555,
83.9853724843829,84.4832951372102,84.9812177900376,85.4791404428649,85.9770630956923,
86.4749857485196,86.972908401347,87.4708310541743,87.9687537070017,88.466676359829,
88.9645990126564,89.4625216654837,89.960444318311,90.4583669711384,90.9562896239657,
91.4542122767931,91.9521349296204,92.4500575824478,92.9479802352751,93.4459028881025,
93.9438255409298,94.4417481937572,94.9396708465845,95.4375934994119,95.9355161522392,
96.4334388050665,96.9313614578939,97.4292841107213,97.9272067635486,98.4251294163759,
98.9230520692033,99.4209747220306,99.918897374858,100.416820027685,100.914742680513,
101.41266533334,101.910587986167,102.408510638995,102.906433291822,103.404355944649,
103.902278597477,104.400201250304,104.898123903131,105.396046555959,105.893969208786,
106.391891861613,106.889814514441,107.387737167268,107.885659820096,108.383582472923,
108.88150512575,109.379427778578,109.877350431405,110.375273084232,110.87319573706,
111.371118389887,111.869041042714,112.366963695542,112.864886348369,113.362809001196,
113.860731654024,114.358654306851,114.856576959678,115.354499612506,115.852422265333,
116.35034491816,116.848267570988,117.346190223815,117.844112876642,118.34203552947,
118.839958182297,119.337880835125,119.835803487952,120.333726140779,120.831648793607,
121.329571446434,121.827494099261,122.325416752089,122.823339404916,123.321262057743,
123.819184710571,124.317107363398,124.815030016225,125.312952669053,125.81087532188,
126.308797974707,126.806720627535,127.304643280362,127.802565933189),
 .UNSPECIFIED.);
#279=B_SPLINE_SURFACE_WITH_KNOTS('',3,3,((#58334,#58335,#58336,#58337,#58338,
#58339,#58340,#58341,#58342,#58343,#58344,#58345,#58346,#58347,#58348,#58349,
#58350,#58351,#58352,#58353,#58354,#58355,#58356,#58357,#58358,#58359,#58360,
#58361,#58362,#58363,#58364,#58365,#58366,#58367,#58368,#58369,#58370,#58371,
#58372,#58373,#58374,#58375,#58376,#58377,#58378,#58379,#58380,#58381,#58382,
#58383,#58384,#58385,#58386,#58387,#58388,#58389,#58390,#58391,#58392,#58393,
#58394,#58395,#58396,#58397,#58398,#58399,#58400,#58401,#58402,#58403,#58404,
#58405,#58406,#58407,#58408,#58409,#58410,#58411,#58412,#58413,#58414,#58415,
#58416,#58417,#58418,#58419,#58420,#58421,#58422,#58423,#58424,#58425,#58426,
#58427,#58428,#58429,#58430,#58431,#58432,#58433,#58434,#58435,#58436,#58437,
#58438,#58439,#58440,#58441,#58442,#58443,#58444,#58445,#58446,#58447,#58448,
#58449,#58450,#58451,#58452,#58453,#58454,#58455,#58456,#58457,#58458,#58459,
#58460,#58461,#58462,#58463,#58464,#58465,#58466,#58467,#58468,#58469,#58470,
#58471,#58472,#58473,#58474,#58475,#58476,#58477,#58478,#58479,#58480,#58481,
#58482,#58483,#58484,#58485,#58486,#58487,#58488,#58489,#58490,#58491,#58492,
#58493,#58494,#58495,#58496,#58497,#58498,#58499,#58500,#58501,#58502,#58503,
#58504,#58505,#58506,#58507,#58508,#58509,#58510,#58511,#58512,#58513,#58514,
#58515,#58516,#58517,#58518,#58519,#58520,#58521,#58522,#58523,#58524,#58525,
#58526,#58527,#58528,#58529,#58530,#58531,#58532,#58533,#58534,#58535,#58536,
#58537,#58538,#58539,#58540,#58541,#58542,#58543,#58544,#58545,#58546,#58547,
#58548,#58549,#58550,#58551,#58552,#58553,#58554,#58555,#58556,#58557,#58558,
#58559,#58560,#58561,#58562,#58563,#58564,#58565,#58566,#58567,#58568,#58569,
#58570,#58571,#58572,#58573,#58574,#58575,#58576),(#58577,#58578,#58579,
#58580,#58581,#58582,#58583,#58584,#58585,#58586,#58587,#58588,#58589,#58590,
#58591,#58592,#58593,#58594,#58595,#58596,#58597,#58598,#58599,#58600,#58601,
#58602,#58603,#58604,#58605,#58606,#58607,#58608,#58609,#58610,#58611,#58612,
#58613,#58614,#58615,#58616,#58617,#58618,#58619,#58620,#58621,#58622,#58623,
#58624,#58625,#58626,#58627,#58628,#58629,#58630,#58631,#58632,#58633,#58634,
#58635,#58636,#58637,#58638,#58639,#58640,#58641,#58642,#58643,#58644,#58645,
#58646,#58647,#58648,#58649,#58650,#58651,#58652,#58653,#58654,#58655,#58656,
#58657,#58658,#58659,#58660,#58661,#58662,#58663,#58664,#58665,#58666,#58667,
#58668,#58669,#58670,#58671,#58672,#58673,#58674,#58675,#58676,#58677,#58678,
#58679,#58680,#58681,#58682,#58683,#58684,#58685,#58686,#58687,#58688,#58689,
#58690,#58691,#58692,#58693,#58694,#58695,#58696,#58697,#58698,#58699,#58700,
#58701,#58702,#58703,#58704,#58705,#58706,#58707,#58708,#58709,#58710,#58711,
#58712,#58713,#58714,#58715,#58716,#58717,#58718,#58719,#58720,#58721,#58722,
#58723,#58724,#58725,#58726,#58727,#58728,#58729,#58730,#58731,#58732,#58733,
#58734,#58735,#58736,#58737,#58738,#58739,#58740,#58741,#58742,#58743,#58744,
#58745,#58746,#58747,#58748,#58749,#58750,#58751,#58752,#58753,#58754,#58755,
#58756,#58757,#58758,#58759,#58760,#58761,#58762,#58763,#58764,#58765,#58766,
#58767,#58768,#58769,#58770,#58771,#58772,#58773,#58774,#58775,#58776,#58777,
#58778,#58779,#58780,#58781,#58782,#58783,#58784,#58785,#58786,#58787,#58788,
#58789,#58790,#58791,#58792,#58793,#58794,#58795,#58796,#58797,#58798,#58799,
#58800,#58801,#58802,#58803,#58804,#58805,#58806,#58807,#58808,#58809,#58810,
#58811,#58812,#58813,#58814,#58815,#58816,#58817,#58818,#58819),(#58820,
#58821,#58822,#58823,#58824,#58825,#58826,#58827,#58828,#58829,#58830,#58831,
#58832,#58833,#58834,#58835,#58836,#58837,#58838,#58839,#58840,#58841,#58842,
#58843,#58844,#58845,#58846,#58847,#58848,#58849,#58850,#58851,#58852,#58853,
#58854,#58855,#58856,#58857,#58858,#58859,#58860,#58861,#58862,#58863,#58864,
#58865,#58866,#58867,#58868,#58869,#58870,#58871,#58872,#58873,#58874,#58875,
#58876,#58877,#58878,#58879,#58880,#58881,#58882,#58883,#58884,#58885,#58886,
#58887,#58888,#58889,#58890,#58891,#58892,#58893,#58894,#58895,#58896,#58897,
#58898,#58899,#58900,#58901,#58902,#58903,#58904,#58905,#58906,#58907,#58908,
#58909,#58910,#58911,#58912,#58913,#58914,#58915,#58916,#58917,#58918,#58919,
#58920,#58921,#58922,#58923,#58924,#58925,#58926,#58927,#58928,#58929,#58930,
#58931,#58932,#58933,#58934,#58935,#58936,#58937,#58938,#58939,#58940,#58941,
#58942,#58943,#58944,#58945,#58946,#58947,#58948,#58949,#58950,#58951,#58952,
#58953,#58954,#58955,#58956,#58957,#58958,#58959,#58960,#58961,#58962,#58963,
#58964,#58965,#58966,#58967,#58968,#58969,#58970,#58971,#58972,#58973,#58974,
#58975,#58976,#58977,#58978,#58979,#58980,#58981,#58982,#58983,#58984,#58985,
#58986,#58987,#58988,#58989,#58990,#58991,#58992,#58993,#58994,#58995,#58996,
#58997,#58998,#58999,#59000,#59001,#59002,#59003,#59004,#59005,#59006,#59007,
#59008,#59009,#59010,#59011,#59012,#59013,#59014,#59015,#59016,#59017,#59018,
#59019,#59020,#59021,#59022,#59023,#59024,#59025,#59026,#59027,#59028,#59029,
#59030,#59031,#59032,#59033,#59034,#59035,#59036,#59037,#59038,#59039,#59040,
#59041,#59042,#59043,#59044,#59045,#59046,#59047,#59048,#59049,#59050,#59051,
#59052,#59053,#59054,#59055,#59056,#59057,#59058,#59059,#59060,#59061,#59062),
(#59063,#59064,#59065,#59066,#59067,#59068,#59069,#59070,#59071,#59072,
#59073,#59074,#59075,#59076,#59077,#59078,#59079,#59080,#59081,#59082,#59083,
#59084,#59085,#59086,#59087,#59088,#59089,#59090,#59091,#59092,#59093,#59094,
#59095,#59096,#59097,#59098,#59099,#59100,#59101,#59102,#59103,#59104,#59105,
#59106,#59107,#59108,#59109,#59110,#59111,#59112,#59113,#59114,#59115,#59116,
#59117,#59118,#59119,#59120,#59121,#59122,#59123,#59124,#59125,#59126,#59127,
#59128,#59129,#59130,#59131,#59132,#59133,#59134,#59135,#59136,#59137,#59138,
#59139,#59140,#59141,#59142,#59143,#59144,#59145,#59146,#59147,#59148,#59149,
#59150,#59151,#59152,#59153,#59154,#59155,#59156,#59157,#59158,#59159,#59160,
#59161,#59162,#59163,#59164,#59165,#59166,#59167,#59168,#59169,#59170,#59171,
#59172,#59173,#59174,#59175,#59176,#59177,#59178,#59179,#59180,#59181,#59182,
#59183,#59184,#59185,#59186,#59187,#59188,#59189,#59190,#59191,#59192,#59193,
#59194,#59195,#59196,#59197,#59198,#59199,#59200,#59201,#59202,#59203,#59204,
#59205,#59206,#59207,#59208,#59209,#59210,#59211,#59212,#59213,#59214,#59215,
#59216,#59217,#59218,#59219,#59220,#59221,#59222,#59223,#59224,#59225,#59226,
#59227,#59228,#59229,#59230,#59231,#59232,#59233,#59234,#59235,#59236,#59237,
#59238,#59239,#59240,#59241,#59242,#59243,#59244,#59245,#59246,#59247,#59248,
#59249,#59250,#59251,#59252,#59253,#59254,#59255,#59256,#59257,#59258,#59259,
#59260,#59261,#59262,#59263,#59264,#59265,#59266,#59267,#59268,#59269,#59270,
#59271,#59272,#59273,#59274,#59275,#59276,#59277,#59278,#59279,#59280,#59281,
#59282,#59283,#59284,#59285,#59286,#59287,#59288,#59289,#59290,#59291,#59292,
#59293,#59294,#59295,#59296,#59297,#59298,#59299,#59300,#59301,#59302,#59303,
#59304,#59305)),.UNSPECIFIED.,.F.,.F.,.F.,(4,4),(4,1,1,1,1,1,1,1,1,1,1,
1,1,1,1,1,1,1,1,1,1,1,1,1,1,1,1,1,1,1,1,1,1,1,1,1,1,1,1,1,1,1,1,1,1,1,1,
1,1,1,1,1,1,1,1,1,1,1,1,1,1,1,1,1,1,1,1,1,1,1,1,1,1,1,1,1,1,1,1,1,1,1,1,
1,1,1,1,1,1,1,1,1,1,1,1,1,1,1,1,1,1,1,1,1,1,1,1,1,1,1,1,1,1,1,1,1,1,1,1,
1,1,1,1,1,1,1,1,1,1,1,1,1,1,1,1,1,1,1,1,1,1,1,1,1,1,1,1,1,1,1,1,1,1,1,1,
1,1,1,1,1,1,1,1,1,1,1,1,1,1,1,1,1,1,1,1,1,1,1,1,1,1,1,1,1,1,1,1,1,1,1,1,
1,1,1,1,1,1,1,1,1,1,1,1,1,1,1,1,1,1,1,1,1,1,1,1,1,1,1,1,1,1,1,1,1,1,1,1,
1,1,1,1,1,1,1,1,1,1,1,1,1,4),(0.,0.132097741590586),(11.6150328478182,12.1129555006455,
12.6108781534729,13.1088008063002,13.6067234591276,14.1046461119549,14.6025687647823,
15.1004914176096,15.5984140704369,16.0963367232643,16.5942593760916,17.092182028919,
17.5901046817463,18.0880273345737,18.585949987401,19.0838726402284,19.5817952930557,
20.0797179458831,20.5776405987104,21.0755632515378,21.5734859043651,22.0714085571925,
22.5693312100198,23.0672538628472,23.5651765156745,24.0630991685018,24.5610218213292,
25.0589444741565,25.5568671269839,26.0547897798112,26.5527124326386,27.0506350854659,
27.5485577382933,28.0464803911206,28.544403043948,29.0423256967753,29.5402483496027,
30.03817100243,30.5360936552574,31.0340163080847,31.5319389609121,32.0298616137394,
32.5277842665667,33.0257069193941,33.5236295722214,34.0215522250488,34.5194748778761,
35.0173975307035,35.5153201835308,36.0132428363582,36.5111654891855,37.0090881420129,
37.5070107948402,38.0049334476676,38.5028561004949,39.0007787533223,39.4987014061496,
39.9966240589769,40.4945467118043,40.9924693646316,41.490392017459,41.9883146702863,
42.4862373231137,42.984159975941,43.4820826287684,43.9800052815957,44.4779279344231,
44.9758505872504,45.4737732400778,45.9716958929051,46.4696185457325,46.9675411985598,
47.4654638513871,47.9633865042145,48.4613091570418,48.9592318098692,49.4571544626965,
49.9550771155239,50.4529997683512,50.9509224211786,51.4488450740059,51.9467677268333,
52.4446903796606,52.942613032488,53.4405356853153,53.9384583381427,54.43638099097,
54.9343036437973,55.4322262966247,55.930148949452,56.4280716022794,56.9259942551067,
57.4239169079341,57.9218395607614,58.4197622135888,58.9176848664161,59.4156075192435,
59.9135301720708,60.4114528248982,60.9093754777255,61.4072981305529,61.9052207833802,
62.4031434362076,62.9010660890349,63.3989887418622,63.8969113946896,64.3948340475169,
64.8927567003443,65.3906793531716,65.888602005999,66.3865246588263,66.8844473116537,
67.382369964481,67.8802926173084,68.3782152701357,68.8761379229631,69.3740605757904,
69.8719832286178,70.3699058814451,70.8678285342725,71.3657511870998,71.8636738399271,
72.3615964927545,72.8595191455818,73.3574417984092,73.8553644512365,74.3532871040639,
74.8512097568912,75.3491324097186,75.8470550625459,76.3449777153733,76.8429003682006,
77.340823021028,77.8387456738553,78.3366683266827,78.83459097951,79.3325136323374,
79.8304362851647,80.328358937992,80.8262815908194,81.3242042436467,81.8221268964741,
82.3200495493014,82.8179722021288,83.3158948549561,83.8138175077835,84.3117401606108,
84.8096628134382,85.3075854662655,85.8055081190928,86.3034307719202,86.8013534247476,
87.2992760775749,87.7971987304022,88.2951213832296,88.7930440360569,89.2909666888843,
89.7888893417116,90.286811994539,90.7847346473663,91.2826573001937,91.780579953021,
92.2785026058484,92.7764252586757,93.2743479115031,93.7722705643304,94.2701932171578,
94.7681158699851,95.2660385228125,95.7639611756398,96.2618838284671,96.7598064812945,
97.2577291341218,97.7556517869492,98.2535744397765,98.7514970926039,99.2494197454312,
99.7473423982586,100.245265051086,100.743187703913,101.241110356741,101.739033009568,
102.236955662395,102.734878315223,103.23280096805,103.730723620877,104.228646273705,
104.726568926532,105.224491579359,105.722414232187,106.220336885014,106.718259537841,
107.216182190669,107.714104843496,108.212027496323,108.709950149151,109.207872801978,
109.705795454805,110.203718107633,110.70164076046,111.199563413288,111.697486066115,
112.195408718942,112.69333137177,113.191254024597,113.689176677424,114.187099330252,
114.685021983079,115.182944635906,115.680867288734,116.178789941561,116.676712594388,
117.174635247216,117.672557900043,118.17048055287,118.668403205698,119.166325858525,
119.664248511352,120.16217116418,120.660093817007,121.158016469834,121.655939122662,
122.153861775489,122.651784428317,123.149707081144,123.647629733971,124.145552386799,
124.643475039626,125.141397692453,125.639320345281,126.137242998108,126.635165650935,
127.133088303763,127.63101095659,128.128933609417,128.626856262245,129.124778915072,
129.622701567899,130.120624220727,130.618546873554,131.116469526381),
 .UNSPECIFIED.);
#280=B_SPLINE_SURFACE_WITH_KNOTS('',3,3,((#59484,#59485,#59486,#59487,#59488,
#59489,#59490,#59491,#59492,#59493,#59494,#59495,#59496,#59497,#59498,#59499,
#59500,#59501,#59502,#59503,#59504,#59505,#59506,#59507,#59508,#59509,#59510,
#59511,#59512,#59513,#59514,#59515,#59516,#59517,#59518,#59519,#59520,#59521,
#59522,#59523,#59524,#59525,#59526,#59527,#59528,#59529),(#59530,#59531,
#59532,#59533,#59534,#59535,#59536,#59537,#59538,#59539,#59540,#59541,#59542,
#59543,#59544,#59545,#59546,#59547,#59548,#59549,#59550,#59551,#59552,#59553,
#59554,#59555,#59556,#59557,#59558,#59559,#59560,#59561,#59562,#59563,#59564,
#59565,#59566,#59567,#59568,#59569,#59570,#59571,#59572,#59573,#59574,#59575),
(#59576,#59577,#59578,#59579,#59580,#59581,#59582,#59583,#59584,#59585,
#59586,#59587,#59588,#59589,#59590,#59591,#59592,#59593,#59594,#59595,#59596,
#59597,#59598,#59599,#59600,#59601,#59602,#59603,#59604,#59605,#59606,#59607,
#59608,#59609,#59610,#59611,#59612,#59613,#59614,#59615,#59616,#59617,#59618,
#59619,#59620,#59621),(#59622,#59623,#59624,#59625,#59626,#59627,#59628,
#59629,#59630,#59631,#59632,#59633,#59634,#59635,#59636,#59637,#59638,#59639,
#59640,#59641,#59642,#59643,#59644,#59645,#59646,#59647,#59648,#59649,#59650,
#59651,#59652,#59653,#59654,#59655,#59656,#59657,#59658,#59659,#59660,#59661,
#59662,#59663,#59664,#59665,#59666,#59667)),.UNSPECIFIED.,.F.,.T.,.F.,(4,
4),(4,1,1,1,1,1,1,1,1,1,1,1,1,1,1,1,1,1,1,1,1,1,1,1,1,1,1,1,1,1,1,1,1,1,
1,1,1,1,1,1,1,1,1,4),(0.,1.),(0.,0.434952646357303,0.869905292714605,1.08738161589326,
1.30485793907191,1.73981058542921,2.17476323178651,2.39223955496516,2.50097771655449,
2.55534679734915,2.60971587814382,3.04466852450112,3.15340668609044,3.47962117085842,
3.51586722472153,3.55211327858464,3.62460538631086,3.76958960176329,4.05955803266816,
4.34952646357303,4.6394948944779,4.92946332538276,5.21943175628763,5.5094001871925,
5.72687651037115,5.79936861809737,6.37930547990711,6.66927391081198,6.95924234171684,
7.24921077262171,7.53917920352658,7.82914763443145,8.11911606533632,8.26410028078875,
8.69905292714605,8.98902135805092,9.27898978895579,9.85892665076553,10.4388635125753,
10.8738161589326,10.9825543205219,11.3087688052899,11.7437214516472,12.1786740980045),
 .UNSPECIFIED.);
#281=B_SPLINE_SURFACE_WITH_KNOTS('',3,3,((#59965,#59966,#59967,#59968,#59969,
#59970,#59971,#59972,#59973,#59974,#59975,#59976,#59977,#59978,#59979,#59980,
#59981,#59982,#59983,#59984,#59985,#59986,#59987,#59988,#59989,#59990,#59991,
#59992,#59993,#59994,#59995,#59996,#59997,#59998,#59999,#60000,#60001,#60002,
#60003,#60004,#60005,#60006,#60007,#60008,#60009,#60010,#60011,#60012,#60013,
#60014,#60015,#60016,#60017,#60018),(#60019,#60020,#60021,#60022,#60023,
#60024,#60025,#60026,#60027,#60028,#60029,#60030,#60031,#60032,#60033,#60034,
#60035,#60036,#60037,#60038,#60039,#60040,#60041,#60042,#60043,#60044,#60045,
#60046,#60047,#60048,#60049,#60050,#60051,#60052,#60053,#60054,#60055,#60056,
#60057,#60058,#60059,#60060,#60061,#60062,#60063,#60064,#60065,#60066,#60067,
#60068,#60069,#60070,#60071,#60072),(#60073,#60074,#60075,#60076,#60077,
#60078,#60079,#60080,#60081,#60082,#60083,#60084,#60085,#60086,#60087,#60088,
#60089,#60090,#60091,#60092,#60093,#60094,#60095,#60096,#60097,#60098,#60099,
#60100,#60101,#60102,#60103,#60104,#60105,#60106,#60107,#60108,#60109,#60110,
#60111,#60112,#60113,#60114,#60115,#60116,#60117,#60118,#60119,#60120,#60121,
#60122,#60123,#60124,#60125,#60126),(#60127,#60128,#60129,#60130,#60131,
#60132,#60133,#60134,#60135,#60136,#60137,#60138,#60139,#60140,#60141,#60142,
#60143,#60144,#60145,#60146,#60147,#60148,#60149,#60150,#60151,#60152,#60153,
#60154,#60155,#60156,#60157,#60158,#60159,#60160,#60161,#60162,#60163,#60164,
#60165,#60166,#60167,#60168,#60169,#60170,#60171,#60172,#60173,#60174,#60175,
#60176,#60177,#60178,#60179,#60180)),.UNSPECIFIED.,.F.,.T.,.F.,(4,4),(4,
1,1,1,1,1,1,1,1,1,1,1,1,1,1,1,1,1,1,1,1,1,1,1,1,1,1,1,1,1,1,1,1,1,1,1,1,
1,1,1,1,1,1,1,1,1,1,1,1,1,1,4),(0.,1.),(0.,0.434952646357303,0.869905292714606,
1.08738161589326,1.30485793907191,1.73981058542921,1.84854874701854,2.17476323178651,
2.39223955496517,2.50097771655449,2.51456998675316,2.55534679734915,2.58253133774649,
2.60971587814382,2.88156128211713,3.04466852450112,3.47962117085842,3.51586722472153,
3.52492873818731,3.55211327858464,3.62460538631086,3.76958960176329,3.87832776335262,
4.05955803266816,4.34952646357303,4.6394948944779,4.85697121765655,4.92946332538276,
5.21943175628763,5.5094001871925,5.79936861809737,6.01684494127602,6.08933704900224,
6.37930547990711,6.95924234171684,7.03173444944306,7.24921077262171,7.53917920352658,
7.82914763443145,8.11911606533632,8.55406871169362,8.69905292714606,8.98902135805092,
9.27898978895579,9.64145032758688,9.85892665076553,10.4388635125753,10.8738161589326,
10.9825543205219,11.3087688052899,11.7437214516472,12.1786740980045),
 .UNSPECIFIED.);
#282=B_SPLINE_SURFACE_WITH_KNOTS('',3,3,((#60230,#60231,#60232,#60233,#60234,
#60235,#60236,#60237,#60238,#60239,#60240,#60241,#60242,#60243,#60244),
(#60245,#60246,#60247,#60248,#60249,#60250,#60251,#60252,#60253,#60254,
#60255,#60256,#60257,#60258,#60259),(#60260,#60261,#60262,#60263,#60264,
#60265,#60266,#60267,#60268,#60269,#60270,#60271,#60272,#60273,#60274),
(#60275,#60276,#60277,#60278,#60279,#60280,#60281,#60282,#60283,#60284,
#60285,#60286,#60287,#60288,#60289)),.UNSPECIFIED.,.F.,.F.,.F.,(4,4),(4,
1,1,1,1,1,1,1,2,2,4),(0.,1.),(0.442064469509103,0.769855887687593,1.09764730586608,
1.26154301495533,1.42543872404457,1.58933443313382,1.75323014222306,1.91712585131231,
2.08102156040155,2.14351932926336,2.6484237026181),.UNSPECIFIED.);
#283=B_SPLINE_SURFACE_WITH_KNOTS('',3,3,((#60302,#60303,#60304,#60305,#60306,
#60307,#60308,#60309,#60310,#60311,#60312,#60313,#60314,#60315),(#60316,
#60317,#60318,#60319,#60320,#60321,#60322,#60323,#60324,#60325,#60326,#60327,
#60328,#60329),(#60330,#60331,#60332,#60333,#60334,#60335,#60336,#60337,
#60338,#60339,#60340,#60341,#60342,#60343),(#60344,#60345,#60346,#60347,
#60348,#60349,#60350,#60351,#60352,#60353,#60354,#60355,#60356,#60357)),
 .UNSPECIFIED.,.F.,.F.,.F.,(4,4),(4,1,1,1,1,1,1,2,2,4),(0.,1.),(3.53272900796379,
3.8604875262342,4.18824604450462,4.35212530363983,4.51600456277503,4.72085363669404,
4.84376308104545,5.17152159931586,5.23401936817767,5.73877023945777),
 .UNSPECIFIED.);
#284=B_SPLINE_SURFACE_WITH_KNOTS('',3,3,((#60370,#60371,#60372,#60373,#60374,
#60375,#60376,#60377,#60378,#60379,#60380,#60381,#60382,#60383,#60384,#60385,
#60386,#60387,#60388,#60389,#60390,#60391,#60392,#60393),(#60394,#60395,
#60396,#60397,#60398,#60399,#60400,#60401,#60402,#60403,#60404,#60405,#60406,
#60407,#60408,#60409,#60410,#60411,#60412,#60413,#60414,#60415,#60416,#60417),
(#60418,#60419,#60420,#60421,#60422,#60423,#60424,#60425,#60426,#60427,
#60428,#60429,#60430,#60431,#60432,#60433,#60434,#60435,#60436,#60437,#60438,
#60439,#60440,#60441),(#60442,#60443,#60444,#60445,#60446,#60447,#60448,
#60449,#60450,#60451,#60452,#60453,#60454,#60455,#60456,#60457,#60458,#60459,
#60460,#60461,#60462,#60463,#60464,#60465)),.UNSPECIFIED.,.F.,.T.,.F.,(4,
4),(4,1,1,1,1,2,2,1,2,1,1,1,1,1,1,1,1,1,4),(0.,1.),(-3.74583112016425,-3.27642035446956,
-3.15906766304589,-2.80700958877487,-2.33759882308018,-1.86818805738549,
-1.79629199573878,-1.50783982646145,-1.21938765718412,-0.911365009587737,
-0.757353685789545,-0.603342361991352,-0.295319714394966,-0.141308390596773,
0.0127029332014201,0.320725580797806,0.628748228394192,0.936770875990578,
1.24479352358696),.UNSPECIFIED.);
#285=B_SPLINE_SURFACE_WITH_KNOTS('',3,3,((#60599,#60600,#60601,#60602,#60603,
#60604,#60605,#60606,#60607,#60608,#60609,#60610,#60611,#60612,#60613,#60614,
#60615,#60616,#60617,#60618,#60619,#60620,#60621,#60622,#60623,#60624,#60625,
#60626,#60627,#60628,#60629,#60630,#60631,#60632,#60633,#60634,#60635,#60636,
#60637,#60638,#60639,#60640,#60641,#60642,#60643,#60644,#60645,#60646,#60647,
#60648,#60649,#60650,#60651,#60652,#60653,#60654,#60655,#60656),(#60657,
#60658,#60659,#60660,#60661,#60662,#60663,#60664,#60665,#60666,#60667,#60668,
#60669,#60670,#60671,#60672,#60673,#60674,#60675,#60676,#60677,#60678,#60679,
#60680,#60681,#60682,#60683,#60684,#60685,#60686,#60687,#60688,#60689,#60690,
#60691,#60692,#60693,#60694,#60695,#60696,#60697,#60698,#60699,#60700,#60701,
#60702,#60703,#60704,#60705,#60706,#60707,#60708,#60709,#60710,#60711,#60712,
#60713,#60714),(#60715,#60716,#60717,#60718,#60719,#60720,#60721,#60722,
#60723,#60724,#60725,#60726,#60727,#60728,#60729,#60730,#60731,#60732,#60733,
#60734,#60735,#60736,#60737,#60738,#60739,#60740,#60741,#60742,#60743,#60744,
#60745,#60746,#60747,#60748,#60749,#60750,#60751,#60752,#60753,#60754,#60755,
#60756,#60757,#60758,#60759,#60760,#60761,#60762,#60763,#60764,#60765,#60766,
#60767,#60768,#60769,#60770,#60771,#60772),(#60773,#60774,#60775,#60776,
#60777,#60778,#60779,#60780,#60781,#60782,#60783,#60784,#60785,#60786,#60787,
#60788,#60789,#60790,#60791,#60792,#60793,#60794,#60795,#60796,#60797,#60798,
#60799,#60800,#60801,#60802,#60803,#60804,#60805,#60806,#60807,#60808,#60809,
#60810,#60811,#60812,#60813,#60814,#60815,#60816,#60817,#60818,#60819,#60820,
#60821,#60822,#60823,#60824,#60825,#60826,#60827,#60828,#60829,#60830)),
 .UNSPECIFIED.,.F.,.T.,.F.,(4,4),(4,1,1,1,1,1,1,1,1,1,1,1,1,1,1,1,1,1,1,
1,1,1,1,1,1,1,1,1,1,1,1,1,1,1,1,1,1,1,1,1,1,1,1,1,1,1,1,1,1,1,1,1,1,1,1,
4),(0.,1.),(0.,0.173419326361772,0.346838652723544,0.520257979085315,0.693677305447087,
0.867096631808859,0.953806294989745,0.997161126580188,1.04051595817063,
1.38735461089417,1.41625783195447,1.44516105301476,1.50296749513536,1.61858037937654,
1.73419326361772,1.8498061478589,2.08103191634126,2.10993513740156,2.13883835846185,
2.19664480058244,2.25445124270303,2.28335446376333,2.31225768482362,2.54348345330599,
2.57238667436628,2.60128989542658,2.65909633754717,2.77470922178835,2.94812854815012,
3.12154787451189,3.20825753769278,3.29496720087366,3.38167686405455,3.39251557195216,
3.40335427984977,3.42503169564499,3.4358704035426,3.44670911144021,3.45754781933783,
3.46296717328663,3.46838652723544,3.64180585359721,3.81522517995898,3.82606388785659,
3.8369025957542,3.85858001154942,3.90193484313987,3.98864450632075,4.07535416950164,
4.16206383268252,4.33548315904429,4.35716057483952,4.37883799063474,4.42219282222518,
4.50890248540607,4.85574113812961),.UNSPECIFIED.);
#286=B_SPLINE_SURFACE_WITH_KNOTS('',3,3,((#63397,#63398,#63399,#63400,#63401,
#63402,#63403,#63404,#63405,#63406,#63407,#63408,#63409,#63410,#63411,#63412,
#63413,#63414,#63415,#63416,#63417,#63418,#63419,#63420,#63421,#63422,#63423,
#63424,#63425,#63426,#63427,#63428,#63429,#63430,#63431,#63432,#63433,#63434,
#63435,#63436),(#63437,#63438,#63439,#63440,#63441,#63442,#63443,#63444,
#63445,#63446,#63447,#63448,#63449,#63450,#63451,#63452,#63453,#63454,#63455,
#63456,#63457,#63458,#63459,#63460,#63461,#63462,#63463,#63464,#63465,#63466,
#63467,#63468,#63469,#63470,#63471,#63472,#63473,#63474,#63475,#63476),
(#63477,#63478,#63479,#63480,#63481,#63482,#63483,#63484,#63485,#63486,
#63487,#63488,#63489,#63490,#63491,#63492,#63493,#63494,#63495,#63496,#63497,
#63498,#63499,#63500,#63501,#63502,#63503,#63504,#63505,#63506,#63507,#63508,
#63509,#63510,#63511,#63512,#63513,#63514,#63515,#63516),(#63517,#63518,
#63519,#63520,#63521,#63522,#63523,#63524,#63525,#63526,#63527,#63528,#63529,
#63530,#63531,#63532,#63533,#63534,#63535,#63536,#63537,#63538,#63539,#63540,
#63541,#63542,#63543,#63544,#63545,#63546,#63547,#63548,#63549,#63550,#63551,
#63552,#63553,#63554,#63555,#63556)),.UNSPECIFIED.,.F.,.T.,.F.,(4,4),(4,
1,1,1,1,1,1,1,1,1,1,1,1,1,1,1,1,1,1,1,1,1,1,1,1,1,1,1,1,1,1,1,1,1,1,1,1,
4),(0.,1.),(0.,0.176188248237271,0.352376496474541,0.528564744711812,0.704752992949082,
0.880941241186353,0.969035365304988,1.01308242736431,1.03510595839396,1.05712948942362,
1.40950598589816,1.42418833991794,1.43887069393771,1.46823540197725,1.52696481805635,
1.64442365021453,1.76188248237271,1.87934131453089,2.11425897884725,2.17298839492634,
2.23171781100543,2.34917664316361,2.58409430747997,2.64282372355906,2.81901197179633,
2.93647080395451,3.05392963611269,3.17138846827087,3.28884730042905,3.52376496474541,
3.64122379690359,3.75868262906177,3.99360029337813,4.22851795769449,4.40470620593176,
4.58089445416904,4.75708270240631,4.93327095064358),.UNSPECIFIED.);
#287=B_SPLINE_SURFACE_WITH_KNOTS('',2,1,((#65478,#65479),(#65480,#65481),
(#65482,#65483)),.UNSPECIFIED.,.F.,.F.,.F.,(3,3),(2,2),(-1.,0.),(0.,0.4),
 .UNSPECIFIED.);
#288=B_SPLINE_SURFACE_WITH_KNOTS('',2,1,((#65489,#65490),(#65491,#65492),
(#65493,#65494)),.UNSPECIFIED.,.F.,.F.,.F.,(3,3),(2,2),(-1.,0.),(0.,0.4),
 .UNSPECIFIED.);
#289=B_SPLINE_SURFACE_WITH_KNOTS('',2,1,((#65504,#65505),(#65506,#65507),
(#65508,#65509)),.UNSPECIFIED.,.F.,.F.,.F.,(3,3),(2,2),(-1.,0.),(0.,0.4),
 .UNSPECIFIED.);
#290=B_SPLINE_SURFACE_WITH_KNOTS('',2,1,((#65515,#65516),(#65517,#65518),
(#65519,#65520)),.UNSPECIFIED.,.F.,.F.,.F.,(3,3),(2,2),(-1.,0.),(0.,0.4),
 .UNSPECIFIED.);
#291=B_SPLINE_SURFACE_WITH_KNOTS('',2,1,((#65570,#65571),(#65572,#65573),
(#65574,#65575)),.UNSPECIFIED.,.F.,.F.,.F.,(3,3),(2,2),(-1.,0.),(0.,0.4),
 .UNSPECIFIED.);
#292=B_SPLINE_SURFACE_WITH_KNOTS('',2,1,((#65588,#65589),(#65590,#65591),
(#65592,#65593)),.UNSPECIFIED.,.F.,.F.,.F.,(3,3),(2,2),(-1.,0.),(0.,0.4),
 .UNSPECIFIED.);
#293=B_SPLINE_SURFACE_WITH_KNOTS('',2,1,((#65603,#65604),(#65605,#65606),
(#65607,#65608)),.UNSPECIFIED.,.F.,.F.,.F.,(3,3),(2,2),(-1.,0.),(0.,0.4),
 .UNSPECIFIED.);
#294=B_SPLINE_SURFACE_WITH_KNOTS('',2,1,((#65618,#65619),(#65620,#65621),
(#65622,#65623)),.UNSPECIFIED.,.F.,.F.,.F.,(3,3),(2,2),(-1.,0.),(0.,0.4),
 .UNSPECIFIED.);
#295=B_SPLINE_SURFACE_WITH_KNOTS('',2,1,((#65633,#65634),(#65635,#65636),
(#65637,#65638)),.UNSPECIFIED.,.F.,.F.,.F.,(3,3),(2,2),(-1.,0.),(0.,0.4),
 .UNSPECIFIED.);
#296=B_SPLINE_SURFACE_WITH_KNOTS('',2,1,((#65648,#65649),(#65650,#65651),
(#65652,#65653)),.UNSPECIFIED.,.F.,.F.,.F.,(3,3),(2,2),(-1.,0.),(0.,0.4),
 .UNSPECIFIED.);
#297=B_SPLINE_SURFACE_WITH_KNOTS('',2,1,((#65663,#65664),(#65665,#65666),
(#65667,#65668)),.UNSPECIFIED.,.F.,.F.,.F.,(3,3),(2,2),(-1.,0.),(0.,0.4),
 .UNSPECIFIED.);
#298=B_SPLINE_SURFACE_WITH_KNOTS('',2,1,((#65678,#65679),(#65680,#65681),
(#65682,#65683)),.UNSPECIFIED.,.F.,.F.,.F.,(3,3),(2,2),(-1.,0.),(0.,0.4),
 .UNSPECIFIED.);
#299=B_SPLINE_SURFACE_WITH_KNOTS('',2,1,((#65690,#65691),(#65692,#65693),
(#65694,#65695)),.UNSPECIFIED.,.F.,.F.,.F.,(3,3),(2,2),(-1.,0.),(0.,0.4),
 .UNSPECIFIED.);
#300=B_SPLINE_SURFACE_WITH_KNOTS('',2,1,((#65703,#65704),(#65705,#65706),
(#65707,#65708)),.UNSPECIFIED.,.F.,.F.,.F.,(3,3),(2,2),(-1.,0.),(0.,0.4),
 .UNSPECIFIED.);
#301=B_SPLINE_SURFACE_WITH_KNOTS('',2,1,((#65714,#65715),(#65716,#65717),
(#65718,#65719)),.UNSPECIFIED.,.F.,.F.,.F.,(3,3),(2,2),(-1.,0.),(0.,0.4),
 .UNSPECIFIED.);
#302=B_SPLINE_SURFACE_WITH_KNOTS('',2,1,((#65725,#65726),(#65727,#65728),
(#65729,#65730)),.UNSPECIFIED.,.F.,.F.,.F.,(3,3),(2,2),(-1.,0.),(0.,0.4),
 .UNSPECIFIED.);
#303=B_SPLINE_SURFACE_WITH_KNOTS('',2,1,((#65736,#65737),(#65738,#65739),
(#65740,#65741)),.UNSPECIFIED.,.F.,.F.,.F.,(3,3),(2,2),(-1.,0.),(0.,0.4),
 .UNSPECIFIED.);
#304=B_SPLINE_SURFACE_WITH_KNOTS('',2,1,((#65747,#65748),(#65749,#65750),
(#65751,#65752)),.UNSPECIFIED.,.F.,.F.,.F.,(3,3),(2,2),(-1.,0.),(0.,0.4),
 .UNSPECIFIED.);
#305=B_SPLINE_SURFACE_WITH_KNOTS('',2,1,((#65758,#65759),(#65760,#65761),
(#65762,#65763)),.UNSPECIFIED.,.F.,.F.,.F.,(3,3),(2,2),(-1.,0.),(0.,0.4),
 .UNSPECIFIED.);
#306=B_SPLINE_SURFACE_WITH_KNOTS('',2,1,((#65769,#65770),(#65771,#65772),
(#65773,#65774)),.UNSPECIFIED.,.F.,.F.,.F.,(3,3),(2,2),(-1.,0.),(0.,0.4),
 .UNSPECIFIED.);
#307=B_SPLINE_SURFACE_WITH_KNOTS('',2,1,((#65780,#65781),(#65782,#65783),
(#65784,#65785)),.UNSPECIFIED.,.F.,.F.,.F.,(3,3),(2,2),(-1.,0.),(0.,0.4),
 .UNSPECIFIED.);
#308=B_SPLINE_SURFACE_WITH_KNOTS('',2,1,((#65791,#65792),(#65793,#65794),
(#65795,#65796)),.UNSPECIFIED.,.F.,.F.,.F.,(3,3),(2,2),(-1.,0.),(0.,0.4),
 .UNSPECIFIED.);
#309=B_SPLINE_SURFACE_WITH_KNOTS('',2,1,((#67768,#67769),(#67770,#67771),
(#67772,#67773)),.UNSPECIFIED.,.F.,.F.,.F.,(3,3),(2,2),(0.,1.),(0.,0.04),
 .UNSPECIFIED.);
#310=B_SPLINE_SURFACE_WITH_KNOTS('',2,1,((#67786,#67787),(#67788,#67789),
(#67790,#67791)),.UNSPECIFIED.,.F.,.F.,.F.,(3,3),(2,2),(0.,1.),(0.,0.04),
 .UNSPECIFIED.);
#311=B_SPLINE_SURFACE_WITH_KNOTS('',2,1,((#67801,#67802),(#67803,#67804),
(#67805,#67806)),.UNSPECIFIED.,.F.,.F.,.F.,(3,3),(2,2),(0.,1.),(0.,0.04),
 .UNSPECIFIED.);
#312=B_SPLINE_SURFACE_WITH_KNOTS('',2,1,((#67816,#67817),(#67818,#67819),
(#67820,#67821)),.UNSPECIFIED.,.F.,.F.,.F.,(3,3),(2,2),(0.,1.),(0.,0.04),
 .UNSPECIFIED.);
#313=B_SPLINE_SURFACE_WITH_KNOTS('',2,1,((#67831,#67832),(#67833,#67834),
(#67835,#67836)),.UNSPECIFIED.,.F.,.F.,.F.,(3,3),(2,2),(0.,1.),(0.,0.04),
 .UNSPECIFIED.);
#314=B_SPLINE_SURFACE_WITH_KNOTS('',2,1,((#67846,#67847),(#67848,#67849),
(#67850,#67851)),.UNSPECIFIED.,.F.,.F.,.F.,(3,3),(2,2),(0.,1.),(0.,0.04),
 .UNSPECIFIED.);
#315=B_SPLINE_SURFACE_WITH_KNOTS('',2,1,((#67861,#67862),(#67863,#67864),
(#67865,#67866)),.UNSPECIFIED.,.F.,.F.,.F.,(3,3),(2,2),(0.,1.),(0.,0.04),
 .UNSPECIFIED.);
#316=B_SPLINE_SURFACE_WITH_KNOTS('',2,1,((#67876,#67877),(#67878,#67879),
(#67880,#67881)),.UNSPECIFIED.,.F.,.F.,.F.,(3,3),(2,2),(0.,1.),(0.,0.04),
 .UNSPECIFIED.);
#317=B_SPLINE_SURFACE_WITH_KNOTS('',2,1,((#67888,#67889),(#67890,#67891),
(#67892,#67893)),.UNSPECIFIED.,.F.,.F.,.F.,(3,3),(2,2),(0.,1.),(0.,0.04),
 .UNSPECIFIED.);
#318=B_SPLINE_SURFACE_WITH_KNOTS('',2,1,((#67906,#67907),(#67908,#67909),
(#67910,#67911)),.UNSPECIFIED.,.F.,.F.,.F.,(3,3),(2,2),(0.,1.),(0.,0.04),
 .UNSPECIFIED.);
#319=B_SPLINE_SURFACE_WITH_KNOTS('',2,1,((#67921,#67922),(#67923,#67924),
(#67925,#67926)),.UNSPECIFIED.,.F.,.F.,.F.,(3,3),(2,2),(0.,1.),(0.,0.04),
 .UNSPECIFIED.);
#320=B_SPLINE_SURFACE_WITH_KNOTS('',2,1,((#67936,#67937),(#67938,#67939),
(#67940,#67941)),.UNSPECIFIED.,.F.,.F.,.F.,(3,3),(2,2),(0.,1.),(0.,0.04),
 .UNSPECIFIED.);
#321=B_SPLINE_SURFACE_WITH_KNOTS('',2,1,((#67951,#67952),(#67953,#67954),
(#67955,#67956)),.UNSPECIFIED.,.F.,.F.,.F.,(3,3),(2,2),(0.,1.),(0.,0.04),
 .UNSPECIFIED.);
#322=B_SPLINE_SURFACE_WITH_KNOTS('',2,1,((#67966,#67967),(#67968,#67969),
(#67970,#67971)),.UNSPECIFIED.,.F.,.F.,.F.,(3,3),(2,2),(0.,1.),(0.,0.04),
 .UNSPECIFIED.);
#323=B_SPLINE_SURFACE_WITH_KNOTS('',2,1,((#67981,#67982),(#67983,#67984),
(#67985,#67986)),.UNSPECIFIED.,.F.,.F.,.F.,(3,3),(2,2),(0.,1.),(0.,0.04),
 .UNSPECIFIED.);
#324=B_SPLINE_SURFACE_WITH_KNOTS('',2,1,((#67996,#67997),(#67998,#67999),
(#68000,#68001)),.UNSPECIFIED.,.F.,.F.,.F.,(3,3),(2,2),(0.,1.),(0.,0.04),
 .UNSPECIFIED.);
#325=B_SPLINE_SURFACE_WITH_KNOTS('',2,1,((#68011,#68012),(#68013,#68014),
(#68015,#68016)),.UNSPECIFIED.,.F.,.F.,.F.,(3,3),(2,2),(0.,1.),(0.,0.04),
 .UNSPECIFIED.);
#326=B_SPLINE_SURFACE_WITH_KNOTS('',2,1,((#68023,#68024),(#68025,#68026),
(#68027,#68028)),.UNSPECIFIED.,.F.,.F.,.F.,(3,3),(2,2),(0.,1.),(0.,0.04),
 .UNSPECIFIED.);
#327=B_SPLINE_SURFACE_WITH_KNOTS('',2,1,((#68041,#68042),(#68043,#68044),
(#68045,#68046)),.UNSPECIFIED.,.F.,.F.,.F.,(3,3),(2,2),(0.,1.),(0.,0.04),
 .UNSPECIFIED.);
#328=B_SPLINE_SURFACE_WITH_KNOTS('',2,1,((#68056,#68057),(#68058,#68059),
(#68060,#68061)),.UNSPECIFIED.,.F.,.F.,.F.,(3,3),(2,2),(0.,1.),(0.,0.04),
 .UNSPECIFIED.);
#329=B_SPLINE_SURFACE_WITH_KNOTS('',2,1,((#68071,#68072),(#68073,#68074),
(#68075,#68076)),.UNSPECIFIED.,.F.,.F.,.F.,(3,3),(2,2),(0.,1.),(0.,0.04),
 .UNSPECIFIED.);
#330=B_SPLINE_SURFACE_WITH_KNOTS('',2,1,((#68086,#68087),(#68088,#68089),
(#68090,#68091)),.UNSPECIFIED.,.F.,.F.,.F.,(3,3),(2,2),(0.,1.),(0.,0.04),
 .UNSPECIFIED.);
#331=B_SPLINE_SURFACE_WITH_KNOTS('',2,1,((#68101,#68102),(#68103,#68104),
(#68105,#68106)),.UNSPECIFIED.,.F.,.F.,.F.,(3,3),(2,2),(0.,1.),(0.,0.04),
 .UNSPECIFIED.);
#332=B_SPLINE_SURFACE_WITH_KNOTS('',2,1,((#68116,#68117),(#68118,#68119),
(#68120,#68121)),.UNSPECIFIED.,.F.,.F.,.F.,(3,3),(2,2),(0.,1.),(0.,0.04),
 .UNSPECIFIED.);
#333=B_SPLINE_SURFACE_WITH_KNOTS('',2,1,((#68131,#68132),(#68133,#68134),
(#68135,#68136)),.UNSPECIFIED.,.F.,.F.,.F.,(3,3),(2,2),(0.,1.),(0.,0.04),
 .UNSPECIFIED.);
#334=B_SPLINE_SURFACE_WITH_KNOTS('',2,1,((#68146,#68147),(#68148,#68149),
(#68150,#68151)),.UNSPECIFIED.,.F.,.F.,.F.,(3,3),(2,2),(0.,1.),(0.,0.04),
 .UNSPECIFIED.);
#335=B_SPLINE_SURFACE_WITH_KNOTS('',2,1,((#68161,#68162),(#68163,#68164),
(#68165,#68166)),.UNSPECIFIED.,.F.,.F.,.F.,(3,3),(2,2),(0.,1.),(0.,0.04),
 .UNSPECIFIED.);
#336=B_SPLINE_SURFACE_WITH_KNOTS('',2,1,((#68176,#68177),(#68178,#68179),
(#68180,#68181)),.UNSPECIFIED.,.F.,.F.,.F.,(3,3),(2,2),(0.,1.),(0.,0.04),
 .UNSPECIFIED.);
#337=B_SPLINE_SURFACE_WITH_KNOTS('',2,1,((#68191,#68192),(#68193,#68194),
(#68195,#68196)),.UNSPECIFIED.,.F.,.F.,.F.,(3,3),(2,2),(0.,1.),(0.,0.04),
 .UNSPECIFIED.);
#338=B_SPLINE_SURFACE_WITH_KNOTS('',2,1,((#68206,#68207),(#68208,#68209),
(#68210,#68211)),.UNSPECIFIED.,.F.,.F.,.F.,(3,3),(2,2),(0.,1.),(0.,0.04),
 .UNSPECIFIED.);
#339=B_SPLINE_SURFACE_WITH_KNOTS('',2,1,((#68221,#68222),(#68223,#68224),
(#68225,#68226)),.UNSPECIFIED.,.F.,.F.,.F.,(3,3),(2,2),(0.,1.),(0.,0.04),
 .UNSPECIFIED.);
#340=B_SPLINE_SURFACE_WITH_KNOTS('',2,1,((#68236,#68237),(#68238,#68239),
(#68240,#68241)),.UNSPECIFIED.,.F.,.F.,.F.,(3,3),(2,2),(0.,1.),(0.,0.04),
 .UNSPECIFIED.);
#341=B_SPLINE_SURFACE_WITH_KNOTS('',2,1,((#68251,#68252),(#68253,#68254),
(#68255,#68256)),.UNSPECIFIED.,.F.,.F.,.F.,(3,3),(2,2),(0.,1.),(0.,0.04),
 .UNSPECIFIED.);
#342=B_SPLINE_SURFACE_WITH_KNOTS('',2,1,((#68289,#68290),(#68291,#68292),
(#68293,#68294)),.UNSPECIFIED.,.F.,.F.,.F.,(3,3),(2,2),(0.,1.),(0.,0.04),
 .UNSPECIFIED.);
#343=B_SPLINE_SURFACE_WITH_KNOTS('',2,1,((#68307,#68308),(#68309,#68310),
(#68311,#68312)),.UNSPECIFIED.,.F.,.F.,.F.,(3,3),(2,2),(0.,1.),(0.,0.04),
 .UNSPECIFIED.);
#344=B_SPLINE_SURFACE_WITH_KNOTS('',2,1,((#68322,#68323),(#68324,#68325),
(#68326,#68327)),.UNSPECIFIED.,.F.,.F.,.F.,(3,3),(2,2),(0.,1.),(0.,0.04),
 .UNSPECIFIED.);
#345=B_SPLINE_SURFACE_WITH_KNOTS('',2,1,((#68337,#68338),(#68339,#68340),
(#68341,#68342)),.UNSPECIFIED.,.F.,.F.,.F.,(3,3),(2,2),(0.,1.),(0.,0.04),
 .UNSPECIFIED.);
#346=B_SPLINE_SURFACE_WITH_KNOTS('',2,1,((#68352,#68353),(#68354,#68355),
(#68356,#68357)),.UNSPECIFIED.,.F.,.F.,.F.,(3,3),(2,2),(0.,1.),(0.,0.04),
 .UNSPECIFIED.);
#347=B_SPLINE_SURFACE_WITH_KNOTS('',2,1,((#68367,#68368),(#68369,#68370),
(#68371,#68372)),.UNSPECIFIED.,.F.,.F.,.F.,(3,3),(2,2),(0.,1.),(0.,0.04),
 .UNSPECIFIED.);
#348=B_SPLINE_SURFACE_WITH_KNOTS('',2,1,((#68382,#68383),(#68384,#68385),
(#68386,#68387)),.UNSPECIFIED.,.F.,.F.,.F.,(3,3),(2,2),(0.,1.),(0.,0.04),
 .UNSPECIFIED.);
#349=B_SPLINE_SURFACE_WITH_KNOTS('',2,1,((#68397,#68398),(#68399,#68400),
(#68401,#68402)),.UNSPECIFIED.,.F.,.F.,.F.,(3,3),(2,2),(0.,1.),(0.,0.04),
 .UNSPECIFIED.);
#350=B_SPLINE_SURFACE_WITH_KNOTS('',2,1,((#68409,#68410),(#68411,#68412),
(#68413,#68414)),.UNSPECIFIED.,.F.,.F.,.F.,(3,3),(2,2),(0.,1.),(0.,0.04),
 .UNSPECIFIED.);
#351=B_SPLINE_SURFACE_WITH_KNOTS('',2,1,((#68427,#68428),(#68429,#68430),
(#68431,#68432)),.UNSPECIFIED.,.F.,.F.,.F.,(3,3),(2,2),(0.,1.),(0.,0.04),
 .UNSPECIFIED.);
#352=B_SPLINE_SURFACE_WITH_KNOTS('',2,1,((#68442,#68443),(#68444,#68445),
(#68446,#68447)),.UNSPECIFIED.,.F.,.F.,.F.,(3,3),(2,2),(0.,1.),(0.,0.04),
 .UNSPECIFIED.);
#353=B_SPLINE_SURFACE_WITH_KNOTS('',2,1,((#68457,#68458),(#68459,#68460),
(#68461,#68462)),.UNSPECIFIED.,.F.,.F.,.F.,(3,3),(2,2),(0.,1.),(0.,0.04),
 .UNSPECIFIED.);
#354=B_SPLINE_SURFACE_WITH_KNOTS('',2,1,((#68472,#68473),(#68474,#68475),
(#68476,#68477)),.UNSPECIFIED.,.F.,.F.,.F.,(3,3),(2,2),(0.,1.),(0.,0.04),
 .UNSPECIFIED.);
#355=B_SPLINE_SURFACE_WITH_KNOTS('',2,1,((#68487,#68488),(#68489,#68490),
(#68491,#68492)),.UNSPECIFIED.,.F.,.F.,.F.,(3,3),(2,2),(0.,1.),(0.,0.04),
 .UNSPECIFIED.);
#356=B_SPLINE_SURFACE_WITH_KNOTS('',2,1,((#68502,#68503),(#68504,#68505),
(#68506,#68507)),.UNSPECIFIED.,.F.,.F.,.F.,(3,3),(2,2),(0.,1.),(0.,0.04),
 .UNSPECIFIED.);
#357=B_SPLINE_SURFACE_WITH_KNOTS('',2,1,((#68517,#68518),(#68519,#68520),
(#68521,#68522)),.UNSPECIFIED.,.F.,.F.,.F.,(3,3),(2,2),(0.,1.),(0.,0.04),
 .UNSPECIFIED.);
#358=B_SPLINE_SURFACE_WITH_KNOTS('',2,1,((#68532,#68533),(#68534,#68535),
(#68536,#68537)),.UNSPECIFIED.,.F.,.F.,.F.,(3,3),(2,2),(0.,1.),(0.,0.04),
 .UNSPECIFIED.);
#359=B_SPLINE_SURFACE_WITH_KNOTS('',2,1,((#68544,#68545),(#68546,#68547),
(#68548,#68549)),.UNSPECIFIED.,.F.,.F.,.F.,(3,3),(2,2),(0.,1.),(0.,0.04),
 .UNSPECIFIED.);
#360=B_SPLINE_SURFACE_WITH_KNOTS('',2,1,((#68562,#68563),(#68564,#68565),
(#68566,#68567)),.UNSPECIFIED.,.F.,.F.,.F.,(3,3),(2,2),(0.,1.),(0.,0.04),
 .UNSPECIFIED.);
#361=B_SPLINE_SURFACE_WITH_KNOTS('',2,1,((#68577,#68578),(#68579,#68580),
(#68581,#68582)),.UNSPECIFIED.,.F.,.F.,.F.,(3,3),(2,2),(0.,1.),(0.,0.04),
 .UNSPECIFIED.);
#362=B_SPLINE_SURFACE_WITH_KNOTS('',2,1,((#68592,#68593),(#68594,#68595),
(#68596,#68597)),.UNSPECIFIED.,.F.,.F.,.F.,(3,3),(2,2),(0.,1.),(0.,0.04),
 .UNSPECIFIED.);
#363=B_SPLINE_SURFACE_WITH_KNOTS('',2,1,((#68607,#68608),(#68609,#68610),
(#68611,#68612)),.UNSPECIFIED.,.F.,.F.,.F.,(3,3),(2,2),(0.,1.),(0.,0.04),
 .UNSPECIFIED.);
#364=B_SPLINE_SURFACE_WITH_KNOTS('',2,1,((#68622,#68623),(#68624,#68625),
(#68626,#68627)),.UNSPECIFIED.,.F.,.F.,.F.,(3,3),(2,2),(0.,1.),(0.,0.04),
 .UNSPECIFIED.);
#365=B_SPLINE_SURFACE_WITH_KNOTS('',2,1,((#68637,#68638),(#68639,#68640),
(#68641,#68642)),.UNSPECIFIED.,.F.,.F.,.F.,(3,3),(2,2),(0.,1.),(0.,0.04),
 .UNSPECIFIED.);
#366=B_SPLINE_SURFACE_WITH_KNOTS('',2,1,((#68652,#68653),(#68654,#68655),
(#68656,#68657)),.UNSPECIFIED.,.F.,.F.,.F.,(3,3),(2,2),(0.,1.),(0.,0.04),
 .UNSPECIFIED.);
#367=B_SPLINE_SURFACE_WITH_KNOTS('',2,1,((#68667,#68668),(#68669,#68670),
(#68671,#68672)),.UNSPECIFIED.,.F.,.F.,.F.,(3,3),(2,2),(0.,1.),(0.,0.04),
 .UNSPECIFIED.);
#368=B_SPLINE_SURFACE_WITH_KNOTS('',2,1,((#68682,#68683),(#68684,#68685),
(#68686,#68687)),.UNSPECIFIED.,.F.,.F.,.F.,(3,3),(2,2),(0.,1.),(0.,0.04),
 .UNSPECIFIED.);
#369=B_SPLINE_SURFACE_WITH_KNOTS('',2,1,((#68697,#68698),(#68699,#68700),
(#68701,#68702)),.UNSPECIFIED.,.F.,.F.,.F.,(3,3),(2,2),(0.,1.),(0.,0.04),
 .UNSPECIFIED.);
#370=B_SPLINE_SURFACE_WITH_KNOTS('',2,1,((#68712,#68713),(#68714,#68715),
(#68716,#68717)),.UNSPECIFIED.,.F.,.F.,.F.,(3,3),(2,2),(0.,1.),(0.,0.04),
 .UNSPECIFIED.);
#371=B_SPLINE_SURFACE_WITH_KNOTS('',2,1,((#68727,#68728),(#68729,#68730),
(#68731,#68732)),.UNSPECIFIED.,.F.,.F.,.F.,(3,3),(2,2),(0.,1.),(0.,0.04),
 .UNSPECIFIED.);
#372=B_SPLINE_SURFACE_WITH_KNOTS('',2,1,((#68742,#68743),(#68744,#68745),
(#68746,#68747)),.UNSPECIFIED.,.F.,.F.,.F.,(3,3),(2,2),(0.,1.),(0.,0.04),
 .UNSPECIFIED.);
#373=B_SPLINE_SURFACE_WITH_KNOTS('',2,1,((#68757,#68758),(#68759,#68760),
(#68761,#68762)),.UNSPECIFIED.,.F.,.F.,.F.,(3,3),(2,2),(0.,1.),(0.,0.04),
 .UNSPECIFIED.);
#374=B_SPLINE_SURFACE_WITH_KNOTS('',2,1,((#68772,#68773),(#68774,#68775),
(#68776,#68777)),.UNSPECIFIED.,.F.,.F.,.F.,(3,3),(2,2),(0.,1.),(0.,0.04),
 .UNSPECIFIED.);
#375=B_SPLINE_SURFACE_WITH_KNOTS('',3,3,((#68946,#68947,#68948,#68949,#68950,
#68951,#68952,#68953,#68954,#68955,#68956,#68957,#68958,#68959,#68960,#68961,
#68962,#68963,#68964,#68965,#68966,#68967,#68968,#68969,#68970,#68971,#68972,
#68973,#68974,#68975,#68976,#68977,#68978,#68979,#68980,#68981,#68982,#68983,
#68984,#68985,#68986,#68987,#68988,#68989,#68990,#68991,#68992,#68993,#68994,
#68995,#68996,#68997,#68998,#68999,#69000,#69001,#69002,#69003,#69004,#69005,
#69006,#69007,#69008,#69009,#69010,#69011,#69012,#69013,#69014,#69015,#69016,
#69017,#69018,#69019,#69020,#69021,#69022,#69023,#69024,#69025,#69026,#69027,
#69028,#69029,#69030,#69031,#69032,#69033,#69034,#69035,#69036,#69037,#69038,
#69039,#69040,#69041,#69042,#69043,#69044,#69045,#69046,#69047,#69048,#69049,
#69050,#69051,#69052,#69053,#69054,#69055,#69056,#69057,#69058,#69059,#69060,
#69061,#69062,#69063,#69064,#69065,#69066,#69067,#69068,#69069,#69070,#69071,
#69072,#69073,#69074,#69075,#69076,#69077,#69078,#69079,#69080,#69081,#69082,
#69083,#69084,#69085,#69086,#69087,#69088,#69089,#69090,#69091,#69092,#69093,
#69094,#69095,#69096,#69097,#69098,#69099,#69100,#69101,#69102,#69103,#69104,
#69105,#69106,#69107,#69108,#69109,#69110,#69111,#69112,#69113,#69114,#69115,
#69116,#69117,#69118,#69119,#69120,#69121,#69122,#69123,#69124,#69125,#69126,
#69127,#69128,#69129,#69130,#69131,#69132),(#69133,#69134,#69135,#69136,
#69137,#69138,#69139,#69140,#69141,#69142,#69143,#69144,#69145,#69146,#69147,
#69148,#69149,#69150,#69151,#69152,#69153,#69154,#69155,#69156,#69157,#69158,
#69159,#69160,#69161,#69162,#69163,#69164,#69165,#69166,#69167,#69168,#69169,
#69170,#69171,#69172,#69173,#69174,#69175,#69176,#69177,#69178,#69179,#69180,
#69181,#69182,#69183,#69184,#69185,#69186,#69187,#69188,#69189,#69190,#69191,
#69192,#69193,#69194,#69195,#69196,#69197,#69198,#69199,#69200,#69201,#69202,
#69203,#69204,#69205,#69206,#69207,#69208,#69209,#69210,#69211,#69212,#69213,
#69214,#69215,#69216,#69217,#69218,#69219,#69220,#69221,#69222,#69223,#69224,
#69225,#69226,#69227,#69228,#69229,#69230,#69231,#69232,#69233,#69234,#69235,
#69236,#69237,#69238,#69239,#69240,#69241,#69242,#69243,#69244,#69245,#69246,
#69247,#69248,#69249,#69250,#69251,#69252,#69253,#69254,#69255,#69256,#69257,
#69258,#69259,#69260,#69261,#69262,#69263,#69264,#69265,#69266,#69267,#69268,
#69269,#69270,#69271,#69272,#69273,#69274,#69275,#69276,#69277,#69278,#69279,
#69280,#69281,#69282,#69283,#69284,#69285,#69286,#69287,#69288,#69289,#69290,
#69291,#69292,#69293,#69294,#69295,#69296,#69297,#69298,#69299,#69300,#69301,
#69302,#69303,#69304,#69305,#69306,#69307,#69308,#69309,#69310,#69311,#69312,
#69313,#69314,#69315,#69316,#69317,#69318,#69319),(#69320,#69321,#69322,
#69323,#69324,#69325,#69326,#69327,#69328,#69329,#69330,#69331,#69332,#69333,
#69334,#69335,#69336,#69337,#69338,#69339,#69340,#69341,#69342,#69343,#69344,
#69345,#69346,#69347,#69348,#69349,#69350,#69351,#69352,#69353,#69354,#69355,
#69356,#69357,#69358,#69359,#69360,#69361,#69362,#69363,#69364,#69365,#69366,
#69367,#69368,#69369,#69370,#69371,#69372,#69373,#69374,#69375,#69376,#69377,
#69378,#69379,#69380,#69381,#69382,#69383,#69384,#69385,#69386,#69387,#69388,
#69389,#69390,#69391,#69392,#69393,#69394,#69395,#69396,#69397,#69398,#69399,
#69400,#69401,#69402,#69403,#69404,#69405,#69406,#69407,#69408,#69409,#69410,
#69411,#69412,#69413,#69414,#69415,#69416,#69417,#69418,#69419,#69420,#69421,
#69422,#69423,#69424,#69425,#69426,#69427,#69428,#69429,#69430,#69431,#69432,
#69433,#69434,#69435,#69436,#69437,#69438,#69439,#69440,#69441,#69442,#69443,
#69444,#69445,#69446,#69447,#69448,#69449,#69450,#69451,#69452,#69453,#69454,
#69455,#69456,#69457,#69458,#69459,#69460,#69461,#69462,#69463,#69464,#69465,
#69466,#69467,#69468,#69469,#69470,#69471,#69472,#69473,#69474,#69475,#69476,
#69477,#69478,#69479,#69480,#69481,#69482,#69483,#69484,#69485,#69486,#69487,
#69488,#69489,#69490,#69491,#69492,#69493,#69494,#69495,#69496,#69497,#69498,
#69499,#69500,#69501,#69502,#69503,#69504,#69505,#69506),(#69507,#69508,
#69509,#69510,#69511,#69512,#69513,#69514,#69515,#69516,#69517,#69518,#69519,
#69520,#69521,#69522,#69523,#69524,#69525,#69526,#69527,#69528,#69529,#69530,
#69531,#69532,#69533,#69534,#69535,#69536,#69537,#69538,#69539,#69540,#69541,
#69542,#69543,#69544,#69545,#69546,#69547,#69548,#69549,#69550,#69551,#69552,
#69553,#69554,#69555,#69556,#69557,#69558,#69559,#69560,#69561,#69562,#69563,
#69564,#69565,#69566,#69567,#69568,#69569,#69570,#69571,#69572,#69573,#69574,
#69575,#69576,#69577,#69578,#69579,#69580,#69581,#69582,#69583,#69584,#69585,
#69586,#69587,#69588,#69589,#69590,#69591,#69592,#69593,#69594,#69595,#69596,
#69597,#69598,#69599,#69600,#69601,#69602,#69603,#69604,#69605,#69606,#69607,
#69608,#69609,#69610,#69611,#69612,#69613,#69614,#69615,#69616,#69617,#69618,
#69619,#69620,#69621,#69622,#69623,#69624,#69625,#69626,#69627,#69628,#69629,
#69630,#69631,#69632,#69633,#69634,#69635,#69636,#69637,#69638,#69639,#69640,
#69641,#69642,#69643,#69644,#69645,#69646,#69647,#69648,#69649,#69650,#69651,
#69652,#69653,#69654,#69655,#69656,#69657,#69658,#69659,#69660,#69661,#69662,
#69663,#69664,#69665,#69666,#69667,#69668,#69669,#69670,#69671,#69672,#69673,
#69674,#69675,#69676,#69677,#69678,#69679,#69680,#69681,#69682,#69683,#69684,
#69685,#69686,#69687,#69688,#69689,#69690,#69691,#69692,#69693)),
 .UNSPECIFIED.,.F.,.F.,.F.,(4,4),(4,1,1,1,1,1,1,1,1,1,1,1,1,1,1,1,1,1,1,
1,1,1,1,1,1,1,1,1,1,1,1,1,1,1,1,1,1,1,1,1,1,1,1,1,1,1,1,1,1,1,1,1,1,1,1,
1,1,1,1,1,1,1,1,1,1,1,1,1,1,1,1,1,1,1,1,1,1,1,1,1,1,1,1,1,1,1,1,1,1,1,1,
1,1,1,1,1,1,1,1,1,1,1,1,1,1,1,1,1,1,1,1,1,1,1,1,1,1,1,1,1,1,1,1,1,1,1,1,
1,1,1,1,1,1,1,1,1,1,1,1,1,1,1,1,1,1,1,1,1,1,1,1,1,1,1,1,1,1,1,1,1,1,1,1,
1,1,1,1,1,1,1,1,1,1,1,1,1,1,1,1,1,1,1,1,1,4),(0.,0.132097741590586),(8.30112925462619,
8.79882392626099,9.29651859789579,9.79421326953059,10.2919079411654,10.7896026128002,
11.287297284435,11.7849919560698,12.2826866277046,12.7803812993394,13.2780759709742,
13.775770642609,14.2734653142438,14.7711599858786,15.2688546575134,15.7665493291482,
16.264244000783,16.7619386724178,17.2596333440526,17.7573280156874,18.2550226873222,
18.752717358957,19.2504120305918,19.7481067022266,20.2458013738614,20.7434960454962,
21.241190717131,21.7388853887658,22.2365800604006,22.7342747320354,23.2319694036702,
23.7296640753051,24.2273587469399,24.7250534185747,25.2227480902095,25.7204427618443,
26.2181374334791,26.7158321051139,27.2135267767487,27.7112214483835,28.2089161200183,
28.7066107916531,29.2043054632879,29.7020001349227,30.1996948065575,30.6973894781923,
31.1950841498271,31.6927788214619,32.1904734930967,32.6881681647315,33.1858628363663,
33.6835575080011,34.1812521796359,34.6789468512707,35.1766415229055,35.6743361945403,
36.1720308661751,36.6697255378099,37.1674202094447,37.6651148810795,38.1628095527143,
38.6605042243491,39.1581988959839,39.6558935676187,40.1535882392535,40.6512829108883,
41.1489775825231,41.6466722541579,42.1443669257927,42.6420615974275,43.1397562690623,
43.6374509406971,44.1351456123319,44.6328402839667,45.1305349556015,45.6282296272363,
46.1259242988711,46.6236189705059,47.1213136421407,47.6190083137756,48.1167029854104,
48.6143976570452,49.11209232868,49.6097870003148,50.1074816719496,50.6051763435844,
51.1028710152192,51.600565686854,52.0982603584888,52.5959550301236,53.0936497017584,
53.5913443733932,54.089039045028,54.5867337166628,55.0844283882976,55.5821230599324,
56.0798177315672,56.577512403202,57.0752070748368,57.5729017464716,58.0705964181064,
58.5682910897412,59.065985761376,59.5636804330108,60.0613751046456,60.5590697762804,
61.0567644479152,61.55445911955,62.0521537911848,62.5498484628196,63.0475431344544,
63.5452378060892,64.042932477724,64.5406271493588,65.0383218209936,65.5360164926284,
66.0337111642632,66.531405835898,67.0291005075328,67.5267951791676,68.0244898508024,
68.5221845224372,69.019879194072,69.5175738657069,70.0152685373416,70.5129632089764,
71.0106578806112,71.5083525522461,72.0060472238809,72.5037418955157,73.0014365671505,
73.4991312387853,73.9968259104201,74.4945205820549,74.9922152536897,75.4899099253245,
75.9876045969593,76.4852992685941,76.9829939402289,77.4806886118637,77.9783832834985,
78.4760779551333,78.9737726267681,79.4714672984029,79.9691619700377,80.4668566416725,
80.9645513133073,81.4622459849421,81.9599406565769,82.4576353282117,82.9553299998465,
83.4530246714813,83.9507193431161,84.4484140147509,84.9461086863857,85.4438033580205,
85.9414980296553,86.4391927012901,86.9368873729249,87.4345820445597,87.9322767161945,
88.4299713878293,88.9276660594641,89.4253607310989,89.9230554027337,90.4207500743685,
90.9184447460033,91.4161394176381,91.9138340892729,92.4115287609077,92.9092234325425,
93.4069181041774,93.9046127758121,94.4023074474469,94.9000021190817,95.3976967907166,
95.8953914623514,96.3930861339862,96.890780805621,97.3884754772558,97.8861701488906,
98.3838648205254,98.8815594921602,99.379254163795,99.8769488354298),
 .UNSPECIFIED.);
#376=B_SPLINE_SURFACE_WITH_KNOTS('',3,3,((#69884,#69885,#69886,#69887,#69888,
#69889,#69890,#69891,#69892,#69893,#69894,#69895,#69896,#69897,#69898,#69899,
#69900,#69901,#69902,#69903,#69904,#69905,#69906,#69907,#69908,#69909,#69910,
#69911,#69912,#69913,#69914,#69915,#69916,#69917,#69918,#69919,#69920,#69921,
#69922,#69923,#69924,#69925,#69926,#69927,#69928,#69929,#69930,#69931,#69932,
#69933,#69934,#69935,#69936,#69937,#69938,#69939,#69940,#69941,#69942,#69943,
#69944,#69945,#69946,#69947,#69948,#69949,#69950,#69951,#69952,#69953,#69954,
#69955,#69956,#69957,#69958,#69959,#69960,#69961,#69962,#69963,#69964,#69965,
#69966,#69967,#69968,#69969,#69970,#69971,#69972,#69973,#69974,#69975,#69976,
#69977,#69978,#69979,#69980,#69981,#69982,#69983,#69984,#69985,#69986,#69987,
#69988,#69989,#69990,#69991,#69992,#69993,#69994,#69995,#69996,#69997,#69998,
#69999,#70000,#70001,#70002,#70003,#70004,#70005,#70006,#70007,#70008,#70009,
#70010,#70011,#70012,#70013,#70014,#70015,#70016,#70017,#70018,#70019,#70020,
#70021,#70022,#70023,#70024,#70025,#70026,#70027,#70028,#70029,#70030,#70031,
#70032,#70033,#70034,#70035,#70036,#70037,#70038,#70039,#70040,#70041,#70042,
#70043,#70044,#70045,#70046,#70047,#70048,#70049,#70050,#70051,#70052,#70053,
#70054,#70055,#70056,#70057,#70058,#70059,#70060,#70061,#70062,#70063,#70064,
#70065,#70066,#70067,#70068,#70069,#70070),(#70071,#70072,#70073,#70074,
#70075,#70076,#70077,#70078,#70079,#70080,#70081,#70082,#70083,#70084,#70085,
#70086,#70087,#70088,#70089,#70090,#70091,#70092,#70093,#70094,#70095,#70096,
#70097,#70098,#70099,#70100,#70101,#70102,#70103,#70104,#70105,#70106,#70107,
#70108,#70109,#70110,#70111,#70112,#70113,#70114,#70115,#70116,#70117,#70118,
#70119,#70120,#70121,#70122,#70123,#70124,#70125,#70126,#70127,#70128,#70129,
#70130,#70131,#70132,#70133,#70134,#70135,#70136,#70137,#70138,#70139,#70140,
#70141,#70142,#70143,#70144,#70145,#70146,#70147,#70148,#70149,#70150,#70151,
#70152,#70153,#70154,#70155,#70156,#70157,#70158,#70159,#70160,#70161,#70162,
#70163,#70164,#70165,#70166,#70167,#70168,#70169,#70170,#70171,#70172,#70173,
#70174,#70175,#70176,#70177,#70178,#70179,#70180,#70181,#70182,#70183,#70184,
#70185,#70186,#70187,#70188,#70189,#70190,#70191,#70192,#70193,#70194,#70195,
#70196,#70197,#70198,#70199,#70200,#70201,#70202,#70203,#70204,#70205,#70206,
#70207,#70208,#70209,#70210,#70211,#70212,#70213,#70214,#70215,#70216,#70217,
#70218,#70219,#70220,#70221,#70222,#70223,#70224,#70225,#70226,#70227,#70228,
#70229,#70230,#70231,#70232,#70233,#70234,#70235,#70236,#70237,#70238,#70239,
#70240,#70241,#70242,#70243,#70244,#70245,#70246,#70247,#70248,#70249,#70250,
#70251,#70252,#70253,#70254,#70255,#70256,#70257),(#70258,#70259,#70260,
#70261,#70262,#70263,#70264,#70265,#70266,#70267,#70268,#70269,#70270,#70271,
#70272,#70273,#70274,#70275,#70276,#70277,#70278,#70279,#70280,#70281,#70282,
#70283,#70284,#70285,#70286,#70287,#70288,#70289,#70290,#70291,#70292,#70293,
#70294,#70295,#70296,#70297,#70298,#70299,#70300,#70301,#70302,#70303,#70304,
#70305,#70306,#70307,#70308,#70309,#70310,#70311,#70312,#70313,#70314,#70315,
#70316,#70317,#70318,#70319,#70320,#70321,#70322,#70323,#70324,#70325,#70326,
#70327,#70328,#70329,#70330,#70331,#70332,#70333,#70334,#70335,#70336,#70337,
#70338,#70339,#70340,#70341,#70342,#70343,#70344,#70345,#70346,#70347,#70348,
#70349,#70350,#70351,#70352,#70353,#70354,#70355,#70356,#70357,#70358,#70359,
#70360,#70361,#70362,#70363,#70364,#70365,#70366,#70367,#70368,#70369,#70370,
#70371,#70372,#70373,#70374,#70375,#70376,#70377,#70378,#70379,#70380,#70381,
#70382,#70383,#70384,#70385,#70386,#70387,#70388,#70389,#70390,#70391,#70392,
#70393,#70394,#70395,#70396,#70397,#70398,#70399,#70400,#70401,#70402,#70403,
#70404,#70405,#70406,#70407,#70408,#70409,#70410,#70411,#70412,#70413,#70414,
#70415,#70416,#70417,#70418,#70419,#70420,#70421,#70422,#70423,#70424,#70425,
#70426,#70427,#70428,#70429,#70430,#70431,#70432,#70433,#70434,#70435,#70436,
#70437,#70438,#70439,#70440,#70441,#70442,#70443,#70444),(#70445,#70446,
#70447,#70448,#70449,#70450,#70451,#70452,#70453,#70454,#70455,#70456,#70457,
#70458,#70459,#70460,#70461,#70462,#70463,#70464,#70465,#70466,#70467,#70468,
#70469,#70470,#70471,#70472,#70473,#70474,#70475,#70476,#70477,#70478,#70479,
#70480,#70481,#70482,#70483,#70484,#70485,#70486,#70487,#70488,#70489,#70490,
#70491,#70492,#70493,#70494,#70495,#70496,#70497,#70498,#70499,#70500,#70501,
#70502,#70503,#70504,#70505,#70506,#70507,#70508,#70509,#70510,#70511,#70512,
#70513,#70514,#70515,#70516,#70517,#70518,#70519,#70520,#70521,#70522,#70523,
#70524,#70525,#70526,#70527,#70528,#70529,#70530,#70531,#70532,#70533,#70534,
#70535,#70536,#70537,#70538,#70539,#70540,#70541,#70542,#70543,#70544,#70545,
#70546,#70547,#70548,#70549,#70550,#70551,#70552,#70553,#70554,#70555,#70556,
#70557,#70558,#70559,#70560,#70561,#70562,#70563,#70564,#70565,#70566,#70567,
#70568,#70569,#70570,#70571,#70572,#70573,#70574,#70575,#70576,#70577,#70578,
#70579,#70580,#70581,#70582,#70583,#70584,#70585,#70586,#70587,#70588,#70589,
#70590,#70591,#70592,#70593,#70594,#70595,#70596,#70597,#70598,#70599,#70600,
#70601,#70602,#70603,#70604,#70605,#70606,#70607,#70608,#70609,#70610,#70611,
#70612,#70613,#70614,#70615,#70616,#70617,#70618,#70619,#70620,#70621,#70622,
#70623,#70624,#70625,#70626,#70627,#70628,#70629,#70630,#70631)),
 .UNSPECIFIED.,.F.,.F.,.F.,(4,4),(4,1,1,1,1,1,1,1,1,1,1,1,1,1,1,1,1,1,1,
1,1,1,1,1,1,1,1,1,1,1,1,1,1,1,1,1,1,1,1,1,1,1,1,1,1,1,1,1,1,1,1,1,1,1,1,
1,1,1,1,1,1,1,1,1,1,1,1,1,1,1,1,1,1,1,1,1,1,1,1,1,1,1,1,1,1,1,1,1,1,1,1,
1,1,1,1,1,1,1,1,1,1,1,1,1,1,1,1,1,1,1,1,1,1,1,1,1,1,1,1,1,1,1,1,1,1,1,1,
1,1,1,1,1,1,1,1,1,1,1,1,1,1,1,1,1,1,1,1,1,1,1,1,1,1,1,1,1,1,1,1,1,1,1,1,
1,1,1,1,1,1,1,1,1,1,1,1,1,1,1,1,1,1,1,1,1,4),(0.,0.132097741590586),(11.6150328478182,
12.112727519453,12.6104221910878,13.1081168627226,13.6058115343574,14.1035062059922,
14.601200877627,15.0988955492618,15.5965902208966,16.0942848925314,16.5919795641662,
17.089674235801,17.5873689074358,18.0850635790706,18.5827582507054,19.0804529223402,
19.5781475939751,20.0758422656099,20.5735369372447,21.0712316088795,21.5689262805143,
22.0666209521491,22.5643156237839,23.0620102954187,23.5597049670535,24.0573996386883,
24.5550943103231,25.0527889819579,25.5504836535927,26.0481783252275,26.5458729968623,
27.0435676684971,27.5412623401319,28.0389570117667,28.5366516834015,29.0343463550363,
29.5320410266711,30.0297356983059,30.5274303699407,31.0251250415755,31.5228197132103,
32.0205143848451,32.5182090564799,33.0159037281147,33.5135983997495,34.0112930713843,
34.5089877430191,35.0066824146539,35.5043770862887,36.0020717579235,36.4997664295583,
36.9974611011931,37.4951557728279,37.9928504444627,38.4905451160975,38.9882397877323,
39.4859344593671,39.9836291310019,40.4813238026367,40.9790184742715,41.4767131459063,
41.9744078175411,42.472102489176,42.9697971608108,43.4674918324456,43.9651865040804,
44.4628811757152,44.96057584735,45.4582705189848,45.9559651906196,46.4536598622544,
46.9513545338892,47.449049205524,47.9467438771588,48.4444385487936,48.9421332204284,
49.4398278920632,49.937522563698,50.4352172353328,50.9329119069676,51.4306065786024,
51.9283012502372,52.425995921872,52.9236905935068,53.4213852651416,53.9190799367764,
54.4167746084112,54.914469280046,55.4121639516808,55.9098586233156,56.4075532949504,
56.9052479665852,57.40294263822,57.9006373098548,58.3983319814896,58.8960266531244,
59.3937213247592,59.891415996394,60.3891106680288,60.8868053396636,61.3845000112984,
61.8821946829332,62.379889354568,62.8775840262028,63.3752786978376,63.8729733694724,
64.3706680411072,64.868362712742,65.3660573843768,65.8637520560116,66.3614467276465,
66.8591413992813,67.3568360709161,67.8545307425508,68.3522254141857,68.8499200858205,
69.3476147574553,69.8453094290901,70.3430041007249,70.8406987723597,71.3383934439945,
71.8360881156293,72.3337827872641,72.8314774588989,73.3291721305337,73.8268668021685,
74.3245614738033,74.8222561454381,75.3199508170729,75.8176454887077,76.3153401603425,
76.8130348319773,77.3107295036121,77.8084241752469,78.3061188468817,78.8038135185165,
79.3015081901513,79.7992028617861,80.2968975334209,80.7945922050557,81.2922868766905,
81.7899815483253,82.2876762199601,82.7853708915949,83.2830655632297,83.7807602348645,
84.2784549064993,84.7761495781341,85.2738442497689,85.7715389214037,86.2692335930385,
86.7669282646733,87.2646229363081,87.7623176079429,88.2600122795777,88.7577069512125,
89.2554016228473,89.7530962944821,90.250790966117,90.7484856377518,91.2461803093866,
91.7438749810213,92.2415696526562,92.739264324291,93.2369589959258,93.7346536675606,
94.2323483391954,94.7300430108302,95.227737682465,95.7254323540998,96.2231270257346,
96.7208216973694,97.2185163690042,97.716211040639,98.2139057122738,98.7116003839086,
99.2092950555434,99.7069897271782,100.204684398813,100.702379070448,101.200073742083,
101.697768413717,102.195463085352,102.693157756987,103.190852428622),
 .UNSPECIFIED.);
#377=SHAPE_REPRESENTATION_RELATIONSHIP('SRR','None',#70818,#392);
#378=SHAPE_REPRESENTATION_RELATIONSHIP('SRR','None',#70819,#393);
#379=SHAPE_REPRESENTATION_RELATIONSHIP('SRR','None',#70820,#394);
#380=SHAPE_REPRESENTATION_RELATIONSHIP('SRR','None',#70821,#395);
#381=SHAPE_REPRESENTATION_RELATIONSHIP('SRR','None',#70822,#396);
#382=SHAPE_REPRESENTATION_RELATIONSHIP('SRR','None',#70823,#397);
#383=SHAPE_REPRESENTATION_RELATIONSHIP('SRR','None',#70824,#398);
#384=SHAPE_REPRESENTATION_RELATIONSHIP('SRR','None',#70825,#399);
#385=SHAPE_REPRESENTATION_RELATIONSHIP('SRR','None',#70826,#400);
#386=SHAPE_REPRESENTATION_RELATIONSHIP('SRR','None',#70827,#401);
#387=SHAPE_REPRESENTATION_RELATIONSHIP('SRR','None',#70828,#402);
#388=SHAPE_REPRESENTATION_RELATIONSHIP('SRR','None',#70829,#403);
#389=SHAPE_REPRESENTATION_RELATIONSHIP('SRR','None',#70830,#404);
#390=SHAPE_REPRESENTATION_RELATIONSHIP('SRR','None',#70831,#405);
#391=SHAPE_REPRESENTATION_RELATIONSHIP('SRR','None',#70832,#406);
#392=ADVANCED_BREP_SHAPE_REPRESENTATION('',(#467),#70742);
#393=ADVANCED_BREP_SHAPE_REPRESENTATION('',(#468),#70743);
#394=ADVANCED_BREP_SHAPE_REPRESENTATION('',(#469),#70744);
#395=ADVANCED_BREP_SHAPE_REPRESENTATION('',(#470),#70745);
#396=ADVANCED_BREP_SHAPE_REPRESENTATION('',(#471),#70746);
#397=ADVANCED_BREP_SHAPE_REPRESENTATION('',(#472),#70747);
#398=ADVANCED_BREP_SHAPE_REPRESENTATION('',(#473),#70748);
#399=ADVANCED_BREP_SHAPE_REPRESENTATION('',(#474),#70749);
#400=ADVANCED_BREP_SHAPE_REPRESENTATION('',(#475),#70750);
#401=ADVANCED_BREP_SHAPE_REPRESENTATION('',(#476),#70751);
#402=ADVANCED_BREP_SHAPE_REPRESENTATION('',(#477),#70752);
#403=ADVANCED_BREP_SHAPE_REPRESENTATION('',(#478),#70753);
#404=ADVANCED_BREP_SHAPE_REPRESENTATION('',(#479),#70754);
#405=ADVANCED_BREP_SHAPE_REPRESENTATION('',(#480),#70755);
#406=ADVANCED_BREP_SHAPE_REPRESENTATION('',(#481),#70756);
#407=STYLED_ITEM('',(#71047),#467);
#408=STYLED_ITEM('',(#71061),#468);
#409=STYLED_ITEM('',(#71033),#469);
#410=STYLED_ITEM('',(#71047),#470);
#411=STYLED_ITEM('',(#71033),#471);
#412=STYLED_ITEM('',(#71054),#472);
#413=STYLED_ITEM('',(#71040),#473);
#414=STYLED_ITEM('',(#71054),#474);
#415=STYLED_ITEM('',(#71054),#475);
#416=STYLED_ITEM('',(#71054),#476);
#417=STYLED_ITEM('',(#71033),#477);
#418=STYLED_ITEM('',(#71033),#478);
#419=STYLED_ITEM('',(#71040),#479);
#420=STYLED_ITEM('',(#71026),#26633);
#421=STYLED_ITEM('',(#71026),#26634);
#422=STYLED_ITEM('',(#71026),#26635);
#423=STYLED_ITEM('',(#71026),#26636);
#424=STYLED_ITEM('',(#71026),#26637);
#425=STYLED_ITEM('',(#71026),#26638);
#426=STYLED_ITEM('',(#71026),#26639);
#427=STYLED_ITEM('',(#71026),#26640);
#428=STYLED_ITEM('',(#71026),#26641);
#429=STYLED_ITEM('',(#71026),#26642);
#430=STYLED_ITEM('',(#71026),#26643);
#431=STYLED_ITEM('',(#71026),#26644);
#432=STYLED_ITEM('',(#71026),#26645);
#433=STYLED_ITEM('',(#71026),#26646);
#434=STYLED_ITEM('',(#71026),#26647);
#435=STYLED_ITEM('',(#71026),#26648);
#436=STYLED_ITEM('',(#71026),#26649);
#437=STYLED_ITEM('',(#71026),#26650);
#438=STYLED_ITEM('',(#71026),#26651);
#439=STYLED_ITEM('',(#71026),#26652);
#440=STYLED_ITEM('',(#71026),#26653);
#441=STYLED_ITEM('',(#71026),#26654);
#442=STYLED_ITEM('',(#71026),#26655);
#443=STYLED_ITEM('',(#71026),#26656);
#444=STYLED_ITEM('',(#71026),#26657);
#445=STYLED_ITEM('',(#71026),#26658);
#446=STYLED_ITEM('',(#71026),#26659);
#447=STYLED_ITEM('',(#71026),#26660);
#448=STYLED_ITEM('',(#71026),#26661);
#449=STYLED_ITEM('',(#71026),#26662);
#450=STYLED_ITEM('',(#71026),#26663);
#451=STYLED_ITEM('',(#71026),#26664);
#452=STYLED_ITEM('',(#71026),#26665);
#453=STYLED_ITEM('',(#71026),#26666);
#454=STYLED_ITEM('',(#71026),#26667);
#455=STYLED_ITEM('',(#71026),#26668);
#456=STYLED_ITEM('',(#71026),#26669);
#457=STYLED_ITEM('',(#71026),#26670);
#458=STYLED_ITEM('',(#71026),#26671);
#459=STYLED_ITEM('',(#71026),#26672);
#460=STYLED_ITEM('',(#71026),#26673);
#461=STYLED_ITEM('',(#71026),#26674);
#462=STYLED_ITEM('',(#71026),#26675);
#463=STYLED_ITEM('',(#71026),#26676);
#464=STYLED_ITEM('',(#71026),#26677);
#465=STYLED_ITEM('',(#71026),#480);
#466=STYLED_ITEM('',(#71054),#481);
#467=MANIFOLD_SOLID_BREP('Pinion shaft',#26872);
#468=MANIFOLD_SOLID_BREP('Lever',#26873);
#469=MANIFOLD_SOLID_BREP('Anvil',#26874);
#470=MANIFOLD_SOLID_BREP('Pin',#26875);
#471=MANIFOLD_SOLID_BREP('Handwheel',#26876);
#472=MANIFOLD_SOLID_BREP('Set screw',#26877);
#473=MANIFOLD_SOLID_BREP('Gib',#26878);
#474=MANIFOLD_SOLID_BREP('Set screw',#26879);
#475=MANIFOLD_SOLID_BREP('Nut',#26880);
#476=MANIFOLD_SOLID_BREP('Set screw',#26881);
#477=MANIFOLD_SOLID_BREP('Hub',#26882);
#478=MANIFOLD_SOLID_BREP('Ram',#26883);
#479=MANIFOLD_SOLID_BREP('Knob',#26884);
#480=MANIFOLD_SOLID_BREP('Frame',#26885);
#481=MANIFOLD_SOLID_BREP('Bolt',#26886);
#482=(
BOUNDED_SURFACE()
B_SPLINE_SURFACE(5,1,((#37442,#37443),(#37444,#37445),(#37446,#37447),(#37448,
#37449),(#37450,#37451),(#37452,#37453),(#37454,#37455),(#37456,#37457),
(#37458,#37459),(#37460,#37461),(#37462,#37463),(#37464,#37465),(#37466,
#37467),(#37468,#37469),(#37470,#37471),(#37472,#37473),(#37474,#37475),
(#37476,#37477),(#37478,#37479),(#37480,#37481),(#37482,#37483),(#37484,
#37485),(#37486,#37487),(#37488,#37489),(#37490,#37491),(#37492,#37493),
(#37494,#37495),(#37496,#37497),(#37498,#37499),(#37500,#37501),(#37502,
#37503),(#37504,#37505),(#37506,#37507),(#37508,#37509),(#37510,#37511)),
 .UNSPECIFIED.,.F.,.F.,.F.)
B_SPLINE_SURFACE_WITH_KNOTS((6,1,1,1,1,1,1,1,1,1,1,1,1,1,1,1,1,1,1,1,1,
1,1,1,1,1,1,1,1,1,6),(2,2),(-1.,-0.966666666666667,-0.933333333333333,-0.9,
-0.866666666666667,-0.833333333333333,-0.8,-0.766666666666667,-0.733333333333333,
-0.7,-0.666666666666667,-0.633333333333333,-0.6,-0.566666666666667,-0.533333333333333,
-0.5,-0.466666666666667,-0.433333333333333,-0.4,-0.366666666666667,-0.333333333333333,
-0.3,-0.266666666666667,-0.233333333333333,-0.2,-0.166666666666667,-0.133333333333333,
-0.1,-0.0666666666666667,-0.0333333333333333,0.),(-5.,5.),.UNSPECIFIED.)
GEOMETRIC_REPRESENTATION_ITEM()
RATIONAL_B_SPLINE_SURFACE(((1.,1.),(1.,1.),(1.,1.),(1.,1.),(1.,1.),(1.,
1.),(1.,1.),(1.,1.),(1.,1.),(1.,1.),(1.,1.),(1.,1.),(1.,1.),(1.,1.),(1.,
1.),(1.,1.),(1.,1.),(1.,1.),(1.,1.),(1.,1.),(1.,1.),(1.,1.),(1.,1.),(1.,
1.),(1.,1.),(1.,1.),(1.,1.),(1.,1.),(1.,1.),(1.,1.),(1.,1.),(1.,1.),(1.,
1.),(1.,1.),(1.,1.)))
REPRESENTATION_ITEM('')
SURFACE()
);
#483=(
BOUNDED_SURFACE()
B_SPLINE_SURFACE(5,1,((#37523,#37524),(#37525,#37526),(#37527,#37528),(#37529,
#37530),(#37531,#37532),(#37533,#37534),(#37535,#37536),(#37537,#37538),
(#37539,#37540),(#37541,#37542),(#37543,#37544),(#37545,#37546),(#37547,
#37548),(#37549,#37550),(#37551,#37552),(#37553,#37554),(#37555,#37556),
(#37557,#37558),(#37559,#37560),(#37561,#37562),(#37563,#37564),(#37565,
#37566),(#37567,#37568),(#37569,#37570),(#37571,#37572),(#37573,#37574),
(#37575,#37576),(#37577,#37578),(#37579,#37580),(#37581,#37582),(#37583,
#37584),(#37585,#37586),(#37587,#37588),(#37589,#37590),(#37591,#37592)),
 .UNSPECIFIED.,.F.,.F.,.F.)
B_SPLINE_SURFACE_WITH_KNOTS((6,1,1,1,1,1,1,1,1,1,1,1,1,1,1,1,1,1,1,1,1,
1,1,1,1,1,1,1,1,1,6),(2,2),(0.,0.0333333333333333,0.0666666666666667,0.1,
0.133333333333333,0.166666666666667,0.2,0.233333333333333,0.266666666666667,
0.3,0.333333333333333,0.366666666666667,0.4,0.433333333333333,0.466666666666667,
0.5,0.533333333333333,0.566666666666667,0.6,0.633333333333333,0.666666666666667,
0.7,0.733333333333333,0.766666666666667,0.8,0.833333333333333,0.866666666666667,
0.9,0.933333333333333,0.966666666666667,1.),(-5.,5.),.UNSPECIFIED.)
GEOMETRIC_REPRESENTATION_ITEM()
RATIONAL_B_SPLINE_SURFACE(((1.,1.),(1.,1.),(1.,1.),(1.,1.),(1.,1.),(1.,
1.),(1.,1.),(1.,1.),(1.,1.),(1.,1.),(1.,1.),(1.,1.),(1.,1.),(1.,1.),(1.,
1.),(1.,1.),(1.,1.),(1.,1.),(1.,1.),(1.,1.),(1.,1.),(1.,1.),(1.,1.),(1.,
1.),(1.,1.),(1.,1.),(1.,1.),(1.,1.),(1.,1.),(1.,1.),(1.,1.),(1.,1.),(1.,
1.),(1.,1.),(1.,1.)))
REPRESENTATION_ITEM('')
SURFACE()
);
#484=(
BOUNDED_SURFACE()
B_SPLINE_SURFACE(5,1,((#37601,#37602),(#37603,#37604),(#37605,#37606),(#37607,
#37608),(#37609,#37610),(#37611,#37612),(#37613,#37614),(#37615,#37616),
(#37617,#37618),(#37619,#37620),(#37621,#37622),(#37623,#37624),(#37625,
#37626),(#37627,#37628),(#37629,#37630),(#37631,#37632),(#37633,#37634),
(#37635,#37636),(#37637,#37638),(#37639,#37640),(#37641,#37642),(#37643,
#37644),(#37645,#37646),(#37647,#37648),(#37649,#37650),(#37651,#37652),
(#37653,#37654),(#37655,#37656),(#37657,#37658),(#37659,#37660),(#37661,
#37662),(#37663,#37664),(#37665,#37666),(#37667,#37668),(#37669,#37670)),
 .UNSPECIFIED.,.F.,.F.,.F.)
B_SPLINE_SURFACE_WITH_KNOTS((6,1,1,1,1,1,1,1,1,1,1,1,1,1,1,1,1,1,1,1,1,
1,1,1,1,1,1,1,1,1,6),(2,2),(-1.,-0.966666666666667,-0.933333333333333,-0.9,
-0.866666666666667,-0.833333333333333,-0.8,-0.766666666666667,-0.733333333333333,
-0.7,-0.666666666666667,-0.633333333333333,-0.6,-0.566666666666667,-0.533333333333333,
-0.5,-0.466666666666667,-0.433333333333333,-0.4,-0.366666666666667,-0.333333333333333,
-0.3,-0.266666666666667,-0.233333333333333,-0.2,-0.166666666666667,-0.133333333333333,
-0.1,-0.0666666666666667,-0.0333333333333333,0.),(-5.,5.),.UNSPECIFIED.)
GEOMETRIC_REPRESENTATION_ITEM()
RATIONAL_B_SPLINE_SURFACE(((1.,1.),(1.,1.),(1.,1.),(1.,1.),(1.,1.),(1.,
1.),(1.,1.),(1.,1.),(1.,1.),(1.,1.),(1.,1.),(1.,1.),(1.,1.),(1.,1.),(1.,
1.),(1.,1.),(1.,1.),(1.,1.),(1.,1.),(1.,1.),(1.,1.),(1.,1.),(1.,1.),(1.,
1.),(1.,1.),(1.,1.),(1.,1.),(1.,1.),(1.,1.),(1.,1.),(1.,1.),(1.,1.),(1.,
1.),(1.,1.),(1.,1.)))
REPRESENTATION_ITEM('')
SURFACE()
);
#485=(
BOUNDED_SURFACE()
B_SPLINE_SURFACE(5,1,((#37682,#37683),(#37684,#37685),(#37686,#37687),(#37688,
#37689),(#37690,#37691),(#37692,#37693),(#37694,#37695),(#37696,#37697),
(#37698,#37699),(#37700,#37701),(#37702,#37703),(#37704,#37705),(#37706,
#37707),(#37708,#37709),(#37710,#37711),(#37712,#37713),(#37714,#37715),
(#37716,#37717),(#37718,#37719),(#37720,#37721),(#37722,#37723),(#37724,
#37725),(#37726,#37727),(#37728,#37729),(#37730,#37731),(#37732,#37733),
(#37734,#37735),(#37736,#37737),(#37738,#37739),(#37740,#37741),(#37742,
#37743),(#37744,#37745),(#37746,#37747),(#37748,#37749),(#37750,#37751)),
 .UNSPECIFIED.,.F.,.F.,.F.)
B_SPLINE_SURFACE_WITH_KNOTS((6,1,1,1,1,1,1,1,1,1,1,1,1,1,1,1,1,1,1,1,1,
1,1,1,1,1,1,1,1,1,6),(2,2),(0.,0.0333333333333333,0.0666666666666667,0.1,
0.133333333333333,0.166666666666667,0.2,0.233333333333333,0.266666666666667,
0.3,0.333333333333333,0.366666666666667,0.4,0.433333333333333,0.466666666666667,
0.5,0.533333333333333,0.566666666666667,0.6,0.633333333333333,0.666666666666667,
0.7,0.733333333333333,0.766666666666667,0.8,0.833333333333333,0.866666666666667,
0.9,0.933333333333333,0.966666666666667,1.),(-5.,5.),.UNSPECIFIED.)
GEOMETRIC_REPRESENTATION_ITEM()
RATIONAL_B_SPLINE_SURFACE(((1.,1.),(1.,1.),(1.,1.),(1.,1.),(1.,1.),(1.,
1.),(1.,1.),(1.,1.),(1.,1.),(1.,1.),(1.,1.),(1.,1.),(1.,1.),(1.,1.),(1.,
1.),(1.,1.),(1.,1.),(1.,1.),(1.,1.),(1.,1.),(1.,1.),(1.,1.),(1.,1.),(1.,
1.),(1.,1.),(1.,1.),(1.,1.),(1.,1.),(1.,1.),(1.,1.),(1.,1.),(1.,1.),(1.,
1.),(1.,1.),(1.,1.)))
REPRESENTATION_ITEM('')
SURFACE()
);
#486=(
BOUNDED_SURFACE()
B_SPLINE_SURFACE(5,1,((#37760,#37761),(#37762,#37763),(#37764,#37765),(#37766,
#37767),(#37768,#37769),(#37770,#37771),(#37772,#37773),(#37774,#37775),
(#37776,#37777),(#37778,#37779),(#37780,#37781),(#37782,#37783),(#37784,
#37785),(#37786,#37787),(#37788,#37789),(#37790,#37791),(#37792,#37793),
(#37794,#37795),(#37796,#37797),(#37798,#37799),(#37800,#37801),(#37802,
#37803),(#37804,#37805),(#37806,#37807),(#37808,#37809),(#37810,#37811),
(#37812,#37813),(#37814,#37815),(#37816,#37817),(#37818,#37819),(#37820,
#37821),(#37822,#37823),(#37824,#37825),(#37826,#37827),(#37828,#37829)),
 .UNSPECIFIED.,.F.,.F.,.F.)
B_SPLINE_SURFACE_WITH_KNOTS((6,1,1,1,1,1,1,1,1,1,1,1,1,1,1,1,1,1,1,1,1,
1,1,1,1,1,1,1,1,1,6),(2,2),(-1.,-0.966666666666667,-0.933333333333333,-0.9,
-0.866666666666667,-0.833333333333333,-0.8,-0.766666666666667,-0.733333333333333,
-0.7,-0.666666666666667,-0.633333333333333,-0.6,-0.566666666666667,-0.533333333333333,
-0.5,-0.466666666666667,-0.433333333333333,-0.4,-0.366666666666667,-0.333333333333333,
-0.3,-0.266666666666667,-0.233333333333333,-0.2,-0.166666666666667,-0.133333333333333,
-0.1,-0.0666666666666667,-0.0333333333333333,0.),(-5.,5.),.UNSPECIFIED.)
GEOMETRIC_REPRESENTATION_ITEM()
RATIONAL_B_SPLINE_SURFACE(((1.,1.),(1.,1.),(1.,1.),(1.,1.),(1.,1.),(1.,
1.),(1.,1.),(1.,1.),(1.,1.),(1.,1.),(1.,1.),(1.,1.),(1.,1.),(1.,1.),(1.,
1.),(1.,1.),(1.,1.),(1.,1.),(1.,1.),(1.,1.),(1.,1.),(1.,1.),(1.,1.),(1.,
1.),(1.,1.),(1.,1.),(1.,1.),(1.,1.),(1.,1.),(1.,1.),(1.,1.),(1.,1.),(1.,
1.),(1.,1.),(1.,1.)))
REPRESENTATION_ITEM('')
SURFACE()
);
#487=(
BOUNDED_SURFACE()
B_SPLINE_SURFACE(5,1,((#37841,#37842),(#37843,#37844),(#37845,#37846),(#37847,
#37848),(#37849,#37850),(#37851,#37852),(#37853,#37854),(#37855,#37856),
(#37857,#37858),(#37859,#37860),(#37861,#37862),(#37863,#37864),(#37865,
#37866),(#37867,#37868),(#37869,#37870),(#37871,#37872),(#37873,#37874),
(#37875,#37876),(#37877,#37878),(#37879,#37880),(#37881,#37882),(#37883,
#37884),(#37885,#37886),(#37887,#37888),(#37889,#37890),(#37891,#37892),
(#37893,#37894),(#37895,#37896),(#37897,#37898),(#37899,#37900),(#37901,
#37902),(#37903,#37904),(#37905,#37906),(#37907,#37908),(#37909,#37910)),
 .UNSPECIFIED.,.F.,.F.,.F.)
B_SPLINE_SURFACE_WITH_KNOTS((6,1,1,1,1,1,1,1,1,1,1,1,1,1,1,1,1,1,1,1,1,
1,1,1,1,1,1,1,1,1,6),(2,2),(0.,0.0333333333333333,0.0666666666666667,0.1,
0.133333333333333,0.166666666666667,0.2,0.233333333333333,0.266666666666667,
0.3,0.333333333333333,0.366666666666667,0.4,0.433333333333333,0.466666666666667,
0.5,0.533333333333333,0.566666666666667,0.6,0.633333333333333,0.666666666666667,
0.7,0.733333333333333,0.766666666666667,0.8,0.833333333333333,0.866666666666667,
0.9,0.933333333333333,0.966666666666667,1.),(-5.,5.),.UNSPECIFIED.)
GEOMETRIC_REPRESENTATION_ITEM()
RATIONAL_B_SPLINE_SURFACE(((1.,1.),(1.,1.),(1.,1.),(1.,1.),(1.,1.),(1.,
1.),(1.,1.),(1.,1.),(1.,1.),(1.,1.),(1.,1.),(1.,1.),(1.,1.),(1.,1.),(1.,
1.),(1.,1.),(1.,1.),(1.,1.),(1.,1.),(1.,1.),(1.,1.),(1.,1.),(1.,1.),(1.,
1.),(1.,1.),(1.,1.),(1.,1.),(1.,1.),(1.,1.),(1.,1.),(1.,1.),(1.,1.),(1.,
1.),(1.,1.),(1.,1.)))
REPRESENTATION_ITEM('')
SURFACE()
);
#488=(
BOUNDED_SURFACE()
B_SPLINE_SURFACE(5,1,((#37919,#37920),(#37921,#37922),(#37923,#37924),(#37925,
#37926),(#37927,#37928),(#37929,#37930),(#37931,#37932),(#37933,#37934),
(#37935,#37936),(#37937,#37938),(#37939,#37940),(#37941,#37942),(#37943,
#37944),(#37945,#37946),(#37947,#37948),(#37949,#37950),(#37951,#37952),
(#37953,#37954),(#37955,#37956),(#37957,#37958),(#37959,#37960),(#37961,
#37962),(#37963,#37964),(#37965,#37966),(#37967,#37968),(#37969,#37970),
(#37971,#37972),(#37973,#37974),(#37975,#37976),(#37977,#37978),(#37979,
#37980),(#37981,#37982),(#37983,#37984),(#37985,#37986),(#37987,#37988)),
 .UNSPECIFIED.,.F.,.F.,.F.)
B_SPLINE_SURFACE_WITH_KNOTS((6,1,1,1,1,1,1,1,1,1,1,1,1,1,1,1,1,1,1,1,1,
1,1,1,1,1,1,1,1,1,6),(2,2),(-1.,-0.966666666666667,-0.933333333333333,-0.9,
-0.866666666666667,-0.833333333333333,-0.8,-0.766666666666667,-0.733333333333333,
-0.7,-0.666666666666667,-0.633333333333333,-0.6,-0.566666666666667,-0.533333333333333,
-0.5,-0.466666666666667,-0.433333333333333,-0.4,-0.366666666666667,-0.333333333333333,
-0.3,-0.266666666666667,-0.233333333333333,-0.2,-0.166666666666667,-0.133333333333333,
-0.1,-0.0666666666666667,-0.0333333333333333,0.),(-5.,5.),.UNSPECIFIED.)
GEOMETRIC_REPRESENTATION_ITEM()
RATIONAL_B_SPLINE_SURFACE(((1.,1.),(1.,1.),(1.,1.),(1.,1.),(1.,1.),(1.,
1.),(1.,1.),(1.,1.),(1.,1.),(1.,1.),(1.,1.),(1.,1.),(1.,1.),(1.,1.),(1.,
1.),(1.,1.),(1.,1.),(1.,1.),(1.,1.),(1.,1.),(1.,1.),(1.,1.),(1.,1.),(1.,
1.),(1.,1.),(1.,1.),(1.,1.),(1.,1.),(1.,1.),(1.,1.),(1.,1.),(1.,1.),(1.,
1.),(1.,1.),(1.,1.)))
REPRESENTATION_ITEM('')
SURFACE()
);
#489=(
BOUNDED_SURFACE()
B_SPLINE_SURFACE(5,1,((#38000,#38001),(#38002,#38003),(#38004,#38005),(#38006,
#38007),(#38008,#38009),(#38010,#38011),(#38012,#38013),(#38014,#38015),
(#38016,#38017),(#38018,#38019),(#38020,#38021),(#38022,#38023),(#38024,
#38025),(#38026,#38027),(#38028,#38029),(#38030,#38031),(#38032,#38033),
(#38034,#38035),(#38036,#38037),(#38038,#38039),(#38040,#38041),(#38042,
#38043),(#38044,#38045),(#38046,#38047),(#38048,#38049),(#38050,#38051),
(#38052,#38053),(#38054,#38055),(#38056,#38057),(#38058,#38059),(#38060,
#38061),(#38062,#38063),(#38064,#38065),(#38066,#38067),(#38068,#38069)),
 .UNSPECIFIED.,.F.,.F.,.F.)
B_SPLINE_SURFACE_WITH_KNOTS((6,1,1,1,1,1,1,1,1,1,1,1,1,1,1,1,1,1,1,1,1,
1,1,1,1,1,1,1,1,1,6),(2,2),(0.,0.0333333333333333,0.0666666666666667,0.1,
0.133333333333333,0.166666666666667,0.2,0.233333333333333,0.266666666666667,
0.3,0.333333333333333,0.366666666666667,0.4,0.433333333333333,0.466666666666667,
0.5,0.533333333333333,0.566666666666667,0.6,0.633333333333333,0.666666666666667,
0.7,0.733333333333333,0.766666666666667,0.8,0.833333333333333,0.866666666666667,
0.9,0.933333333333333,0.966666666666667,1.),(-5.,5.),.UNSPECIFIED.)
GEOMETRIC_REPRESENTATION_ITEM()
RATIONAL_B_SPLINE_SURFACE(((1.,1.),(1.,1.),(1.,1.),(1.,1.),(1.,1.),(1.,
1.),(1.,1.),(1.,1.),(1.,1.),(1.,1.),(1.,1.),(1.,1.),(1.,1.),(1.,1.),(1.,
1.),(1.,1.),(1.,1.),(1.,1.),(1.,1.),(1.,1.),(1.,1.),(1.,1.),(1.,1.),(1.,
1.),(1.,1.),(1.,1.),(1.,1.),(1.,1.),(1.,1.),(1.,1.),(1.,1.),(1.,1.),(1.,
1.),(1.,1.),(1.,1.)))
REPRESENTATION_ITEM('')
SURFACE()
);
#490=(
BOUNDED_SURFACE()
B_SPLINE_SURFACE(5,1,((#38078,#38079),(#38080,#38081),(#38082,#38083),(#38084,
#38085),(#38086,#38087),(#38088,#38089),(#38090,#38091),(#38092,#38093),
(#38094,#38095),(#38096,#38097),(#38098,#38099),(#38100,#38101),(#38102,
#38103),(#38104,#38105),(#38106,#38107),(#38108,#38109),(#38110,#38111),
(#38112,#38113),(#38114,#38115),(#38116,#38117),(#38118,#38119),(#38120,
#38121),(#38122,#38123),(#38124,#38125),(#38126,#38127),(#38128,#38129),
(#38130,#38131),(#38132,#38133),(#38134,#38135),(#38136,#38137),(#38138,
#38139),(#38140,#38141),(#38142,#38143),(#38144,#38145),(#38146,#38147)),
 .UNSPECIFIED.,.F.,.F.,.F.)
B_SPLINE_SURFACE_WITH_KNOTS((6,1,1,1,1,1,1,1,1,1,1,1,1,1,1,1,1,1,1,1,1,
1,1,1,1,1,1,1,1,1,6),(2,2),(-1.,-0.966666666666667,-0.933333333333333,-0.9,
-0.866666666666667,-0.833333333333333,-0.8,-0.766666666666667,-0.733333333333333,
-0.7,-0.666666666666667,-0.633333333333333,-0.6,-0.566666666666667,-0.533333333333333,
-0.5,-0.466666666666667,-0.433333333333333,-0.4,-0.366666666666667,-0.333333333333333,
-0.3,-0.266666666666667,-0.233333333333333,-0.2,-0.166666666666667,-0.133333333333333,
-0.1,-0.0666666666666667,-0.0333333333333333,0.),(-5.,5.),.UNSPECIFIED.)
GEOMETRIC_REPRESENTATION_ITEM()
RATIONAL_B_SPLINE_SURFACE(((1.,1.),(1.,1.),(1.,1.),(1.,1.),(1.,1.),(1.,
1.),(1.,1.),(1.,1.),(1.,1.),(1.,1.),(1.,1.),(1.,1.),(1.,1.),(1.,1.),(1.,
1.),(1.,1.),(1.,1.),(1.,1.),(1.,1.),(1.,1.),(1.,1.),(1.,1.),(1.,1.),(1.,
1.),(1.,1.),(1.,1.),(1.,1.),(1.,1.),(1.,1.),(1.,1.),(1.,1.),(1.,1.),(1.,
1.),(1.,1.),(1.,1.)))
REPRESENTATION_ITEM('')
SURFACE()
);
#491=(
BOUNDED_SURFACE()
B_SPLINE_SURFACE(5,1,((#38159,#38160),(#38161,#38162),(#38163,#38164),(#38165,
#38166),(#38167,#38168),(#38169,#38170),(#38171,#38172),(#38173,#38174),
(#38175,#38176),(#38177,#38178),(#38179,#38180),(#38181,#38182),(#38183,
#38184),(#38185,#38186),(#38187,#38188),(#38189,#38190),(#38191,#38192),
(#38193,#38194),(#38195,#38196),(#38197,#38198),(#38199,#38200),(#38201,
#38202),(#38203,#38204),(#38205,#38206),(#38207,#38208),(#38209,#38210),
(#38211,#38212),(#38213,#38214),(#38215,#38216),(#38217,#38218),(#38219,
#38220),(#38221,#38222),(#38223,#38224),(#38225,#38226),(#38227,#38228)),
 .UNSPECIFIED.,.F.,.F.,.F.)
B_SPLINE_SURFACE_WITH_KNOTS((6,1,1,1,1,1,1,1,1,1,1,1,1,1,1,1,1,1,1,1,1,
1,1,1,1,1,1,1,1,1,6),(2,2),(0.,0.0333333333333333,0.0666666666666667,0.1,
0.133333333333333,0.166666666666667,0.2,0.233333333333333,0.266666666666667,
0.3,0.333333333333333,0.366666666666667,0.4,0.433333333333333,0.466666666666667,
0.5,0.533333333333333,0.566666666666667,0.6,0.633333333333333,0.666666666666667,
0.7,0.733333333333333,0.766666666666667,0.8,0.833333333333333,0.866666666666667,
0.9,0.933333333333333,0.966666666666667,1.),(-5.,5.),.UNSPECIFIED.)
GEOMETRIC_REPRESENTATION_ITEM()
RATIONAL_B_SPLINE_SURFACE(((1.,1.),(1.,1.),(1.,1.),(1.,1.),(1.,1.),(1.,
1.),(1.,1.),(1.,1.),(1.,1.),(1.,1.),(1.,1.),(1.,1.),(1.,1.),(1.,1.),(1.,
1.),(1.,1.),(1.,1.),(1.,1.),(1.,1.),(1.,1.),(1.,1.),(1.,1.),(1.,1.),(1.,
1.),(1.,1.),(1.,1.),(1.,1.),(1.,1.),(1.,1.),(1.,1.),(1.,1.),(1.,1.),(1.,
1.),(1.,1.),(1.,1.)))
REPRESENTATION_ITEM('')
SURFACE()
);
#492=(
BOUNDED_SURFACE()
B_SPLINE_SURFACE(5,1,((#38237,#38238),(#38239,#38240),(#38241,#38242),(#38243,
#38244),(#38245,#38246),(#38247,#38248),(#38249,#38250),(#38251,#38252),
(#38253,#38254),(#38255,#38256),(#38257,#38258),(#38259,#38260),(#38261,
#38262),(#38263,#38264),(#38265,#38266),(#38267,#38268),(#38269,#38270),
(#38271,#38272),(#38273,#38274),(#38275,#38276),(#38277,#38278),(#38279,
#38280),(#38281,#38282),(#38283,#38284),(#38285,#38286),(#38287,#38288),
(#38289,#38290),(#38291,#38292),(#38293,#38294),(#38295,#38296),(#38297,
#38298),(#38299,#38300),(#38301,#38302),(#38303,#38304),(#38305,#38306)),
 .UNSPECIFIED.,.F.,.F.,.F.)
B_SPLINE_SURFACE_WITH_KNOTS((6,1,1,1,1,1,1,1,1,1,1,1,1,1,1,1,1,1,1,1,1,
1,1,1,1,1,1,1,1,1,6),(2,2),(-1.,-0.966666666666667,-0.933333333333333,-0.9,
-0.866666666666667,-0.833333333333333,-0.8,-0.766666666666667,-0.733333333333333,
-0.7,-0.666666666666667,-0.633333333333333,-0.6,-0.566666666666667,-0.533333333333333,
-0.5,-0.466666666666667,-0.433333333333333,-0.4,-0.366666666666667,-0.333333333333333,
-0.3,-0.266666666666667,-0.233333333333333,-0.2,-0.166666666666667,-0.133333333333333,
-0.1,-0.0666666666666667,-0.0333333333333333,0.),(-5.,5.),.UNSPECIFIED.)
GEOMETRIC_REPRESENTATION_ITEM()
RATIONAL_B_SPLINE_SURFACE(((1.,1.),(1.,1.),(1.,1.),(1.,1.),(1.,1.),(1.,
1.),(1.,1.),(1.,1.),(1.,1.),(1.,1.),(1.,1.),(1.,1.),(1.,1.),(1.,1.),(1.,
1.),(1.,1.),(1.,1.),(1.,1.),(1.,1.),(1.,1.),(1.,1.),(1.,1.),(1.,1.),(1.,
1.),(1.,1.),(1.,1.),(1.,1.),(1.,1.),(1.,1.),(1.,1.),(1.,1.),(1.,1.),(1.,
1.),(1.,1.),(1.,1.)))
REPRESENTATION_ITEM('')
SURFACE()
);
#493=(
BOUNDED_SURFACE()
B_SPLINE_SURFACE(5,1,((#38318,#38319),(#38320,#38321),(#38322,#38323),(#38324,
#38325),(#38326,#38327),(#38328,#38329),(#38330,#38331),(#38332,#38333),
(#38334,#38335),(#38336,#38337),(#38338,#38339),(#38340,#38341),(#38342,
#38343),(#38344,#38345),(#38346,#38347),(#38348,#38349),(#38350,#38351),
(#38352,#38353),(#38354,#38355),(#38356,#38357),(#38358,#38359),(#38360,
#38361),(#38362,#38363),(#38364,#38365),(#38366,#38367),(#38368,#38369),
(#38370,#38371),(#38372,#38373),(#38374,#38375),(#38376,#38377),(#38378,
#38379),(#38380,#38381),(#38382,#38383),(#38384,#38385),(#38386,#38387)),
 .UNSPECIFIED.,.F.,.F.,.F.)
B_SPLINE_SURFACE_WITH_KNOTS((6,1,1,1,1,1,1,1,1,1,1,1,1,1,1,1,1,1,1,1,1,
1,1,1,1,1,1,1,1,1,6),(2,2),(0.,0.0333333333333333,0.0666666666666667,0.1,
0.133333333333333,0.166666666666667,0.2,0.233333333333333,0.266666666666667,
0.3,0.333333333333333,0.366666666666667,0.4,0.433333333333333,0.466666666666667,
0.5,0.533333333333333,0.566666666666667,0.6,0.633333333333333,0.666666666666667,
0.7,0.733333333333333,0.766666666666667,0.8,0.833333333333333,0.866666666666667,
0.9,0.933333333333333,0.966666666666667,1.),(-5.,5.),.UNSPECIFIED.)
GEOMETRIC_REPRESENTATION_ITEM()
RATIONAL_B_SPLINE_SURFACE(((1.,1.),(1.,1.),(1.,1.),(1.,1.),(1.,1.),(1.,
1.),(1.,1.),(1.,1.),(1.,1.),(1.,1.),(1.,1.),(1.,1.),(1.,1.),(1.,1.),(1.,
1.),(1.,1.),(1.,1.),(1.,1.),(1.,1.),(1.,1.),(1.,1.),(1.,1.),(1.,1.),(1.,
1.),(1.,1.),(1.,1.),(1.,1.),(1.,1.),(1.,1.),(1.,1.),(1.,1.),(1.,1.),(1.,
1.),(1.,1.),(1.,1.)))
REPRESENTATION_ITEM('')
SURFACE()
);
#494=(
BOUNDED_SURFACE()
B_SPLINE_SURFACE(5,1,((#38396,#38397),(#38398,#38399),(#38400,#38401),(#38402,
#38403),(#38404,#38405),(#38406,#38407),(#38408,#38409),(#38410,#38411),
(#38412,#38413),(#38414,#38415),(#38416,#38417),(#38418,#38419),(#38420,
#38421),(#38422,#38423),(#38424,#38425),(#38426,#38427),(#38428,#38429),
(#38430,#38431),(#38432,#38433),(#38434,#38435),(#38436,#38437),(#38438,
#38439),(#38440,#38441),(#38442,#38443),(#38444,#38445),(#38446,#38447),
(#38448,#38449),(#38450,#38451),(#38452,#38453),(#38454,#38455),(#38456,
#38457),(#38458,#38459),(#38460,#38461),(#38462,#38463),(#38464,#38465)),
 .UNSPECIFIED.,.F.,.F.,.F.)
B_SPLINE_SURFACE_WITH_KNOTS((6,1,1,1,1,1,1,1,1,1,1,1,1,1,1,1,1,1,1,1,1,
1,1,1,1,1,1,1,1,1,6),(2,2),(-1.,-0.966666666666667,-0.933333333333333,-0.9,
-0.866666666666667,-0.833333333333333,-0.8,-0.766666666666667,-0.733333333333333,
-0.7,-0.666666666666667,-0.633333333333333,-0.6,-0.566666666666667,-0.533333333333333,
-0.5,-0.466666666666667,-0.433333333333333,-0.4,-0.366666666666667,-0.333333333333333,
-0.3,-0.266666666666667,-0.233333333333333,-0.2,-0.166666666666667,-0.133333333333333,
-0.1,-0.0666666666666667,-0.0333333333333333,0.),(-5.,5.),.UNSPECIFIED.)
GEOMETRIC_REPRESENTATION_ITEM()
RATIONAL_B_SPLINE_SURFACE(((1.,1.),(1.,1.),(1.,1.),(1.,1.),(1.,1.),(1.,
1.),(1.,1.),(1.,1.),(1.,1.),(1.,1.),(1.,1.),(1.,1.),(1.,1.),(1.,1.),(1.,
1.),(1.,1.),(1.,1.),(1.,1.),(1.,1.),(1.,1.),(1.,1.),(1.,1.),(1.,1.),(1.,
1.),(1.,1.),(1.,1.),(1.,1.),(1.,1.),(1.,1.),(1.,1.),(1.,1.),(1.,1.),(1.,
1.),(1.,1.),(1.,1.)))
REPRESENTATION_ITEM('')
SURFACE()
);
#495=(
BOUNDED_SURFACE()
B_SPLINE_SURFACE(5,1,((#38477,#38478),(#38479,#38480),(#38481,#38482),(#38483,
#38484),(#38485,#38486),(#38487,#38488),(#38489,#38490),(#38491,#38492),
(#38493,#38494),(#38495,#38496),(#38497,#38498),(#38499,#38500),(#38501,
#38502),(#38503,#38504),(#38505,#38506),(#38507,#38508),(#38509,#38510),
(#38511,#38512),(#38513,#38514),(#38515,#38516),(#38517,#38518),(#38519,
#38520),(#38521,#38522),(#38523,#38524),(#38525,#38526),(#38527,#38528),
(#38529,#38530),(#38531,#38532),(#38533,#38534),(#38535,#38536),(#38537,
#38538),(#38539,#38540),(#38541,#38542),(#38543,#38544),(#38545,#38546)),
 .UNSPECIFIED.,.F.,.F.,.F.)
B_SPLINE_SURFACE_WITH_KNOTS((6,1,1,1,1,1,1,1,1,1,1,1,1,1,1,1,1,1,1,1,1,
1,1,1,1,1,1,1,1,1,6),(2,2),(0.,0.0333333333333333,0.0666666666666667,0.1,
0.133333333333333,0.166666666666667,0.2,0.233333333333333,0.266666666666667,
0.3,0.333333333333333,0.366666666666667,0.4,0.433333333333333,0.466666666666667,
0.5,0.533333333333333,0.566666666666667,0.6,0.633333333333333,0.666666666666667,
0.7,0.733333333333333,0.766666666666667,0.8,0.833333333333333,0.866666666666667,
0.9,0.933333333333333,0.966666666666667,1.),(-5.,5.),.UNSPECIFIED.)
GEOMETRIC_REPRESENTATION_ITEM()
RATIONAL_B_SPLINE_SURFACE(((1.,1.),(1.,1.),(1.,1.),(1.,1.),(1.,1.),(1.,
1.),(1.,1.),(1.,1.),(1.,1.),(1.,1.),(1.,1.),(1.,1.),(1.,1.),(1.,1.),(1.,
1.),(1.,1.),(1.,1.),(1.,1.),(1.,1.),(1.,1.),(1.,1.),(1.,1.),(1.,1.),(1.,
1.),(1.,1.),(1.,1.),(1.,1.),(1.,1.),(1.,1.),(1.,1.),(1.,1.),(1.,1.),(1.,
1.),(1.,1.),(1.,1.)))
REPRESENTATION_ITEM('')
SURFACE()
);
#496=(
BOUNDED_SURFACE()
B_SPLINE_SURFACE(5,1,((#38555,#38556),(#38557,#38558),(#38559,#38560),(#38561,
#38562),(#38563,#38564),(#38565,#38566),(#38567,#38568),(#38569,#38570),
(#38571,#38572),(#38573,#38574),(#38575,#38576),(#38577,#38578),(#38579,
#38580),(#38581,#38582),(#38583,#38584),(#38585,#38586),(#38587,#38588),
(#38589,#38590),(#38591,#38592),(#38593,#38594),(#38595,#38596),(#38597,
#38598),(#38599,#38600),(#38601,#38602),(#38603,#38604),(#38605,#38606),
(#38607,#38608),(#38609,#38610),(#38611,#38612),(#38613,#38614),(#38615,
#38616),(#38617,#38618),(#38619,#38620),(#38621,#38622),(#38623,#38624)),
 .UNSPECIFIED.,.F.,.F.,.F.)
B_SPLINE_SURFACE_WITH_KNOTS((6,1,1,1,1,1,1,1,1,1,1,1,1,1,1,1,1,1,1,1,1,
1,1,1,1,1,1,1,1,1,6),(2,2),(-1.,-0.966666666666667,-0.933333333333333,-0.9,
-0.866666666666667,-0.833333333333333,-0.8,-0.766666666666667,-0.733333333333333,
-0.7,-0.666666666666667,-0.633333333333333,-0.6,-0.566666666666667,-0.533333333333333,
-0.5,-0.466666666666667,-0.433333333333333,-0.4,-0.366666666666667,-0.333333333333333,
-0.3,-0.266666666666667,-0.233333333333333,-0.2,-0.166666666666667,-0.133333333333333,
-0.1,-0.0666666666666667,-0.0333333333333333,0.),(-5.,5.),.UNSPECIFIED.)
GEOMETRIC_REPRESENTATION_ITEM()
RATIONAL_B_SPLINE_SURFACE(((1.,1.),(1.,1.),(1.,1.),(1.,1.),(1.,1.),(1.,
1.),(1.,1.),(1.,1.),(1.,1.),(1.,1.),(1.,1.),(1.,1.),(1.,1.),(1.,1.),(1.,
1.),(1.,1.),(1.,1.),(1.,1.),(1.,1.),(1.,1.),(1.,1.),(1.,1.),(1.,1.),(1.,
1.),(1.,1.),(1.,1.),(1.,1.),(1.,1.),(1.,1.),(1.,1.),(1.,1.),(1.,1.),(1.,
1.),(1.,1.),(1.,1.)))
REPRESENTATION_ITEM('')
SURFACE()
);
#497=(
BOUNDED_SURFACE()
B_SPLINE_SURFACE(5,1,((#38636,#38637),(#38638,#38639),(#38640,#38641),(#38642,
#38643),(#38644,#38645),(#38646,#38647),(#38648,#38649),(#38650,#38651),
(#38652,#38653),(#38654,#38655),(#38656,#38657),(#38658,#38659),(#38660,
#38661),(#38662,#38663),(#38664,#38665),(#38666,#38667),(#38668,#38669),
(#38670,#38671),(#38672,#38673),(#38674,#38675),(#38676,#38677),(#38678,
#38679),(#38680,#38681),(#38682,#38683),(#38684,#38685),(#38686,#38687),
(#38688,#38689),(#38690,#38691),(#38692,#38693),(#38694,#38695),(#38696,
#38697),(#38698,#38699),(#38700,#38701),(#38702,#38703),(#38704,#38705)),
 .UNSPECIFIED.,.F.,.F.,.F.)
B_SPLINE_SURFACE_WITH_KNOTS((6,1,1,1,1,1,1,1,1,1,1,1,1,1,1,1,1,1,1,1,1,
1,1,1,1,1,1,1,1,1,6),(2,2),(0.,0.0333333333333333,0.0666666666666667,0.1,
0.133333333333333,0.166666666666667,0.2,0.233333333333333,0.266666666666667,
0.3,0.333333333333333,0.366666666666667,0.4,0.433333333333333,0.466666666666667,
0.5,0.533333333333333,0.566666666666667,0.6,0.633333333333333,0.666666666666667,
0.7,0.733333333333333,0.766666666666667,0.8,0.833333333333333,0.866666666666667,
0.9,0.933333333333333,0.966666666666667,1.),(-5.,5.),.UNSPECIFIED.)
GEOMETRIC_REPRESENTATION_ITEM()
RATIONAL_B_SPLINE_SURFACE(((1.,1.),(1.,1.),(1.,1.),(1.,1.),(1.,1.),(1.,
1.),(1.,1.),(1.,1.),(1.,1.),(1.,1.),(1.,1.),(1.,1.),(1.,1.),(1.,1.),(1.,
1.),(1.,1.),(1.,1.),(1.,1.),(1.,1.),(1.,1.),(1.,1.),(1.,1.),(1.,1.),(1.,
1.),(1.,1.),(1.,1.),(1.,1.),(1.,1.),(1.,1.),(1.,1.),(1.,1.),(1.,1.),(1.,
1.),(1.,1.),(1.,1.)))
REPRESENTATION_ITEM('')
SURFACE()
);
#498=(
BOUNDED_SURFACE()
B_SPLINE_SURFACE(5,1,((#38714,#38715),(#38716,#38717),(#38718,#38719),(#38720,
#38721),(#38722,#38723),(#38724,#38725),(#38726,#38727),(#38728,#38729),
(#38730,#38731),(#38732,#38733),(#38734,#38735),(#38736,#38737),(#38738,
#38739),(#38740,#38741),(#38742,#38743),(#38744,#38745),(#38746,#38747),
(#38748,#38749),(#38750,#38751),(#38752,#38753),(#38754,#38755),(#38756,
#38757),(#38758,#38759),(#38760,#38761),(#38762,#38763),(#38764,#38765),
(#38766,#38767),(#38768,#38769),(#38770,#38771),(#38772,#38773),(#38774,
#38775),(#38776,#38777),(#38778,#38779),(#38780,#38781),(#38782,#38783)),
 .UNSPECIFIED.,.F.,.F.,.F.)
B_SPLINE_SURFACE_WITH_KNOTS((6,1,1,1,1,1,1,1,1,1,1,1,1,1,1,1,1,1,1,1,1,
1,1,1,1,1,1,1,1,1,6),(2,2),(-1.,-0.966666666666667,-0.933333333333333,-0.9,
-0.866666666666667,-0.833333333333333,-0.8,-0.766666666666667,-0.733333333333333,
-0.7,-0.666666666666667,-0.633333333333333,-0.6,-0.566666666666667,-0.533333333333333,
-0.5,-0.466666666666667,-0.433333333333333,-0.4,-0.366666666666667,-0.333333333333333,
-0.3,-0.266666666666667,-0.233333333333333,-0.2,-0.166666666666667,-0.133333333333333,
-0.1,-0.0666666666666667,-0.0333333333333333,0.),(-5.,5.),.UNSPECIFIED.)
GEOMETRIC_REPRESENTATION_ITEM()
RATIONAL_B_SPLINE_SURFACE(((1.,1.),(1.,1.),(1.,1.),(1.,1.),(1.,1.),(1.,
1.),(1.,1.),(1.,1.),(1.,1.),(1.,1.),(1.,1.),(1.,1.),(1.,1.),(1.,1.),(1.,
1.),(1.,1.),(1.,1.),(1.,1.),(1.,1.),(1.,1.),(1.,1.),(1.,1.),(1.,1.),(1.,
1.),(1.,1.),(1.,1.),(1.,1.),(1.,1.),(1.,1.),(1.,1.),(1.,1.),(1.,1.),(1.,
1.),(1.,1.),(1.,1.)))
REPRESENTATION_ITEM('')
SURFACE()
);
#499=(
BOUNDED_SURFACE()
B_SPLINE_SURFACE(5,1,((#38795,#38796),(#38797,#38798),(#38799,#38800),(#38801,
#38802),(#38803,#38804),(#38805,#38806),(#38807,#38808),(#38809,#38810),
(#38811,#38812),(#38813,#38814),(#38815,#38816),(#38817,#38818),(#38819,
#38820),(#38821,#38822),(#38823,#38824),(#38825,#38826),(#38827,#38828),
(#38829,#38830),(#38831,#38832),(#38833,#38834),(#38835,#38836),(#38837,
#38838),(#38839,#38840),(#38841,#38842),(#38843,#38844),(#38845,#38846),
(#38847,#38848),(#38849,#38850),(#38851,#38852),(#38853,#38854),(#38855,
#38856),(#38857,#38858),(#38859,#38860),(#38861,#38862),(#38863,#38864)),
 .UNSPECIFIED.,.F.,.F.,.F.)
B_SPLINE_SURFACE_WITH_KNOTS((6,1,1,1,1,1,1,1,1,1,1,1,1,1,1,1,1,1,1,1,1,
1,1,1,1,1,1,1,1,1,6),(2,2),(0.,0.0333333333333333,0.0666666666666667,0.1,
0.133333333333333,0.166666666666667,0.2,0.233333333333333,0.266666666666667,
0.3,0.333333333333333,0.366666666666667,0.4,0.433333333333333,0.466666666666667,
0.5,0.533333333333333,0.566666666666667,0.6,0.633333333333333,0.666666666666667,
0.7,0.733333333333333,0.766666666666667,0.8,0.833333333333333,0.866666666666667,
0.9,0.933333333333333,0.966666666666667,1.),(-5.,5.),.UNSPECIFIED.)
GEOMETRIC_REPRESENTATION_ITEM()
RATIONAL_B_SPLINE_SURFACE(((1.,1.),(1.,1.),(1.,1.),(1.,1.),(1.,1.),(1.,
1.),(1.,1.),(1.,1.),(1.,1.),(1.,1.),(1.,1.),(1.,1.),(1.,1.),(1.,1.),(1.,
1.),(1.,1.),(1.,1.),(1.,1.),(1.,1.),(1.,1.),(1.,1.),(1.,1.),(1.,1.),(1.,
1.),(1.,1.),(1.,1.),(1.,1.),(1.,1.),(1.,1.),(1.,1.),(1.,1.),(1.,1.),(1.,
1.),(1.,1.),(1.,1.)))
REPRESENTATION_ITEM('')
SURFACE()
);
#500=(
BOUNDED_SURFACE()
B_SPLINE_SURFACE(5,1,((#38873,#38874),(#38875,#38876),(#38877,#38878),(#38879,
#38880),(#38881,#38882),(#38883,#38884),(#38885,#38886),(#38887,#38888),
(#38889,#38890),(#38891,#38892),(#38893,#38894),(#38895,#38896),(#38897,
#38898),(#38899,#38900),(#38901,#38902),(#38903,#38904),(#38905,#38906),
(#38907,#38908),(#38909,#38910),(#38911,#38912),(#38913,#38914),(#38915,
#38916),(#38917,#38918),(#38919,#38920),(#38921,#38922),(#38923,#38924),
(#38925,#38926),(#38927,#38928),(#38929,#38930),(#38931,#38932),(#38933,
#38934),(#38935,#38936),(#38937,#38938),(#38939,#38940),(#38941,#38942)),
 .UNSPECIFIED.,.F.,.F.,.F.)
B_SPLINE_SURFACE_WITH_KNOTS((6,1,1,1,1,1,1,1,1,1,1,1,1,1,1,1,1,1,1,1,1,
1,1,1,1,1,1,1,1,1,6),(2,2),(-1.,-0.966666666666667,-0.933333333333333,-0.9,
-0.866666666666667,-0.833333333333333,-0.8,-0.766666666666667,-0.733333333333333,
-0.7,-0.666666666666667,-0.633333333333333,-0.6,-0.566666666666667,-0.533333333333333,
-0.5,-0.466666666666667,-0.433333333333333,-0.4,-0.366666666666667,-0.333333333333333,
-0.3,-0.266666666666667,-0.233333333333333,-0.2,-0.166666666666667,-0.133333333333333,
-0.1,-0.0666666666666667,-0.0333333333333333,0.),(-5.,5.),.UNSPECIFIED.)
GEOMETRIC_REPRESENTATION_ITEM()
RATIONAL_B_SPLINE_SURFACE(((1.,1.),(1.,1.),(1.,1.),(1.,1.),(1.,1.),(1.,
1.),(1.,1.),(1.,1.),(1.,1.),(1.,1.),(1.,1.),(1.,1.),(1.,1.),(1.,1.),(1.,
1.),(1.,1.),(1.,1.),(1.,1.),(1.,1.),(1.,1.),(1.,1.),(1.,1.),(1.,1.),(1.,
1.),(1.,1.),(1.,1.),(1.,1.),(1.,1.),(1.,1.),(1.,1.),(1.,1.),(1.,1.),(1.,
1.),(1.,1.),(1.,1.)))
REPRESENTATION_ITEM('')
SURFACE()
);
#501=(
BOUNDED_SURFACE()
B_SPLINE_SURFACE(5,1,((#38954,#38955),(#38956,#38957),(#38958,#38959),(#38960,
#38961),(#38962,#38963),(#38964,#38965),(#38966,#38967),(#38968,#38969),
(#38970,#38971),(#38972,#38973),(#38974,#38975),(#38976,#38977),(#38978,
#38979),(#38980,#38981),(#38982,#38983),(#38984,#38985),(#38986,#38987),
(#38988,#38989),(#38990,#38991),(#38992,#38993),(#38994,#38995),(#38996,
#38997),(#38998,#38999),(#39000,#39001),(#39002,#39003),(#39004,#39005),
(#39006,#39007),(#39008,#39009),(#39010,#39011),(#39012,#39013),(#39014,
#39015),(#39016,#39017),(#39018,#39019),(#39020,#39021),(#39022,#39023)),
 .UNSPECIFIED.,.F.,.F.,.F.)
B_SPLINE_SURFACE_WITH_KNOTS((6,1,1,1,1,1,1,1,1,1,1,1,1,1,1,1,1,1,1,1,1,
1,1,1,1,1,1,1,1,1,6),(2,2),(0.,0.0333333333333333,0.0666666666666667,0.1,
0.133333333333333,0.166666666666667,0.2,0.233333333333333,0.266666666666667,
0.3,0.333333333333333,0.366666666666667,0.4,0.433333333333333,0.466666666666667,
0.5,0.533333333333333,0.566666666666667,0.6,0.633333333333333,0.666666666666667,
0.7,0.733333333333333,0.766666666666667,0.8,0.833333333333333,0.866666666666667,
0.9,0.933333333333333,0.966666666666667,1.),(-5.,5.),.UNSPECIFIED.)
GEOMETRIC_REPRESENTATION_ITEM()
RATIONAL_B_SPLINE_SURFACE(((1.,1.),(1.,1.),(1.,1.),(1.,1.),(1.,1.),(1.,
1.),(1.,1.),(1.,1.),(1.,1.),(1.,1.),(1.,1.),(1.,1.),(1.,1.),(1.,1.),(1.,
1.),(1.,1.),(1.,1.),(1.,1.),(1.,1.),(1.,1.),(1.,1.),(1.,1.),(1.,1.),(1.,
1.),(1.,1.),(1.,1.),(1.,1.),(1.,1.),(1.,1.),(1.,1.),(1.,1.),(1.,1.),(1.,
1.),(1.,1.),(1.,1.)))
REPRESENTATION_ITEM('')
SURFACE()
);
#502=(
BOUNDED_SURFACE()
B_SPLINE_SURFACE(5,1,((#39032,#39033),(#39034,#39035),(#39036,#39037),(#39038,
#39039),(#39040,#39041),(#39042,#39043),(#39044,#39045),(#39046,#39047),
(#39048,#39049),(#39050,#39051),(#39052,#39053),(#39054,#39055),(#39056,
#39057),(#39058,#39059),(#39060,#39061),(#39062,#39063),(#39064,#39065),
(#39066,#39067),(#39068,#39069),(#39070,#39071),(#39072,#39073),(#39074,
#39075),(#39076,#39077),(#39078,#39079),(#39080,#39081),(#39082,#39083),
(#39084,#39085),(#39086,#39087),(#39088,#39089),(#39090,#39091),(#39092,
#39093),(#39094,#39095),(#39096,#39097),(#39098,#39099),(#39100,#39101)),
 .UNSPECIFIED.,.F.,.F.,.F.)
B_SPLINE_SURFACE_WITH_KNOTS((6,1,1,1,1,1,1,1,1,1,1,1,1,1,1,1,1,1,1,1,1,
1,1,1,1,1,1,1,1,1,6),(2,2),(-1.,-0.966666666666667,-0.933333333333333,-0.9,
-0.866666666666667,-0.833333333333333,-0.8,-0.766666666666667,-0.733333333333333,
-0.7,-0.666666666666667,-0.633333333333333,-0.6,-0.566666666666667,-0.533333333333333,
-0.5,-0.466666666666667,-0.433333333333333,-0.4,-0.366666666666667,-0.333333333333333,
-0.3,-0.266666666666667,-0.233333333333333,-0.2,-0.166666666666667,-0.133333333333333,
-0.1,-0.0666666666666667,-0.0333333333333333,0.),(-5.,5.),.UNSPECIFIED.)
GEOMETRIC_REPRESENTATION_ITEM()
RATIONAL_B_SPLINE_SURFACE(((1.,1.),(1.,1.),(1.,1.),(1.,1.),(1.,1.),(1.,
1.),(1.,1.),(1.,1.),(1.,1.),(1.,1.),(1.,1.),(1.,1.),(1.,1.),(1.,1.),(1.,
1.),(1.,1.),(1.,1.),(1.,1.),(1.,1.),(1.,1.),(1.,1.),(1.,1.),(1.,1.),(1.,
1.),(1.,1.),(1.,1.),(1.,1.),(1.,1.),(1.,1.),(1.,1.),(1.,1.),(1.,1.),(1.,
1.),(1.,1.),(1.,1.)))
REPRESENTATION_ITEM('')
SURFACE()
);
#503=(
BOUNDED_SURFACE()
B_SPLINE_SURFACE(5,1,((#39113,#39114),(#39115,#39116),(#39117,#39118),(#39119,
#39120),(#39121,#39122),(#39123,#39124),(#39125,#39126),(#39127,#39128),
(#39129,#39130),(#39131,#39132),(#39133,#39134),(#39135,#39136),(#39137,
#39138),(#39139,#39140),(#39141,#39142),(#39143,#39144),(#39145,#39146),
(#39147,#39148),(#39149,#39150),(#39151,#39152),(#39153,#39154),(#39155,
#39156),(#39157,#39158),(#39159,#39160),(#39161,#39162),(#39163,#39164),
(#39165,#39166),(#39167,#39168),(#39169,#39170),(#39171,#39172),(#39173,
#39174),(#39175,#39176),(#39177,#39178),(#39179,#39180),(#39181,#39182)),
 .UNSPECIFIED.,.F.,.F.,.F.)
B_SPLINE_SURFACE_WITH_KNOTS((6,1,1,1,1,1,1,1,1,1,1,1,1,1,1,1,1,1,1,1,1,
1,1,1,1,1,1,1,1,1,6),(2,2),(0.,0.0333333333333333,0.0666666666666667,0.1,
0.133333333333333,0.166666666666667,0.2,0.233333333333333,0.266666666666667,
0.3,0.333333333333333,0.366666666666667,0.4,0.433333333333333,0.466666666666667,
0.5,0.533333333333333,0.566666666666667,0.6,0.633333333333333,0.666666666666667,
0.7,0.733333333333333,0.766666666666667,0.8,0.833333333333333,0.866666666666667,
0.9,0.933333333333333,0.966666666666667,1.),(-5.,5.),.UNSPECIFIED.)
GEOMETRIC_REPRESENTATION_ITEM()
RATIONAL_B_SPLINE_SURFACE(((1.,1.),(1.,1.),(1.,1.),(1.,1.),(1.,1.),(1.,
1.),(1.,1.),(1.,1.),(1.,1.),(1.,1.),(1.,1.),(1.,1.),(1.,1.),(1.,1.),(1.,
1.),(1.,1.),(1.,1.),(1.,1.),(1.,1.),(1.,1.),(1.,1.),(1.,1.),(1.,1.),(1.,
1.),(1.,1.),(1.,1.),(1.,1.),(1.,1.),(1.,1.),(1.,1.),(1.,1.),(1.,1.),(1.,
1.),(1.,1.),(1.,1.)))
REPRESENTATION_ITEM('')
SURFACE()
);
#504=(
BOUNDED_SURFACE()
B_SPLINE_SURFACE(5,1,((#39191,#39192),(#39193,#39194),(#39195,#39196),(#39197,
#39198),(#39199,#39200),(#39201,#39202),(#39203,#39204),(#39205,#39206),
(#39207,#39208),(#39209,#39210),(#39211,#39212),(#39213,#39214),(#39215,
#39216),(#39217,#39218),(#39219,#39220),(#39221,#39222),(#39223,#39224),
(#39225,#39226),(#39227,#39228),(#39229,#39230),(#39231,#39232),(#39233,
#39234),(#39235,#39236),(#39237,#39238),(#39239,#39240),(#39241,#39242),
(#39243,#39244),(#39245,#39246),(#39247,#39248),(#39249,#39250),(#39251,
#39252),(#39253,#39254),(#39255,#39256),(#39257,#39258),(#39259,#39260)),
 .UNSPECIFIED.,.F.,.F.,.F.)
B_SPLINE_SURFACE_WITH_KNOTS((6,1,1,1,1,1,1,1,1,1,1,1,1,1,1,1,1,1,1,1,1,
1,1,1,1,1,1,1,1,1,6),(2,2),(-1.,-0.966666666666667,-0.933333333333333,-0.9,
-0.866666666666667,-0.833333333333333,-0.8,-0.766666666666667,-0.733333333333333,
-0.7,-0.666666666666667,-0.633333333333333,-0.6,-0.566666666666667,-0.533333333333333,
-0.5,-0.466666666666667,-0.433333333333333,-0.4,-0.366666666666667,-0.333333333333333,
-0.3,-0.266666666666667,-0.233333333333333,-0.2,-0.166666666666667,-0.133333333333333,
-0.1,-0.0666666666666667,-0.0333333333333333,0.),(-5.,5.),.UNSPECIFIED.)
GEOMETRIC_REPRESENTATION_ITEM()
RATIONAL_B_SPLINE_SURFACE(((1.,1.),(1.,1.),(1.,1.),(1.,1.),(1.,1.),(1.,
1.),(1.,1.),(1.,1.),(1.,1.),(1.,1.),(1.,1.),(1.,1.),(1.,1.),(1.,1.),(1.,
1.),(1.,1.),(1.,1.),(1.,1.),(1.,1.),(1.,1.),(1.,1.),(1.,1.),(1.,1.),(1.,
1.),(1.,1.),(1.,1.),(1.,1.),(1.,1.),(1.,1.),(1.,1.),(1.,1.),(1.,1.),(1.,
1.),(1.,1.),(1.,1.)))
REPRESENTATION_ITEM('')
SURFACE()
);
#505=(
BOUNDED_SURFACE()
B_SPLINE_SURFACE(5,1,((#39272,#39273),(#39274,#39275),(#39276,#39277),(#39278,
#39279),(#39280,#39281),(#39282,#39283),(#39284,#39285),(#39286,#39287),
(#39288,#39289),(#39290,#39291),(#39292,#39293),(#39294,#39295),(#39296,
#39297),(#39298,#39299),(#39300,#39301),(#39302,#39303),(#39304,#39305),
(#39306,#39307),(#39308,#39309),(#39310,#39311),(#39312,#39313),(#39314,
#39315),(#39316,#39317),(#39318,#39319),(#39320,#39321),(#39322,#39323),
(#39324,#39325),(#39326,#39327),(#39328,#39329),(#39330,#39331),(#39332,
#39333),(#39334,#39335),(#39336,#39337),(#39338,#39339),(#39340,#39341)),
 .UNSPECIFIED.,.F.,.F.,.F.)
B_SPLINE_SURFACE_WITH_KNOTS((6,1,1,1,1,1,1,1,1,1,1,1,1,1,1,1,1,1,1,1,1,
1,1,1,1,1,1,1,1,1,6),(2,2),(0.,0.0333333333333333,0.0666666666666667,0.1,
0.133333333333333,0.166666666666667,0.2,0.233333333333333,0.266666666666667,
0.3,0.333333333333333,0.366666666666667,0.4,0.433333333333333,0.466666666666667,
0.5,0.533333333333333,0.566666666666667,0.6,0.633333333333333,0.666666666666667,
0.7,0.733333333333333,0.766666666666667,0.8,0.833333333333333,0.866666666666667,
0.9,0.933333333333333,0.966666666666667,1.),(-5.,5.),.UNSPECIFIED.)
GEOMETRIC_REPRESENTATION_ITEM()
RATIONAL_B_SPLINE_SURFACE(((1.,1.),(1.,1.),(1.,1.),(1.,1.),(1.,1.),(1.,
1.),(1.,1.),(1.,1.),(1.,1.),(1.,1.),(1.,1.),(1.,1.),(1.,1.),(1.,1.),(1.,
1.),(1.,1.),(1.,1.),(1.,1.),(1.,1.),(1.,1.),(1.,1.),(1.,1.),(1.,1.),(1.,
1.),(1.,1.),(1.,1.),(1.,1.),(1.,1.),(1.,1.),(1.,1.),(1.,1.),(1.,1.),(1.,
1.),(1.,1.),(1.,1.)))
REPRESENTATION_ITEM('')
SURFACE()
);
#506=(
BOUNDED_SURFACE()
B_SPLINE_SURFACE(5,1,((#39350,#39351),(#39352,#39353),(#39354,#39355),(#39356,
#39357),(#39358,#39359),(#39360,#39361),(#39362,#39363),(#39364,#39365),
(#39366,#39367),(#39368,#39369),(#39370,#39371),(#39372,#39373),(#39374,
#39375),(#39376,#39377),(#39378,#39379),(#39380,#39381),(#39382,#39383),
(#39384,#39385),(#39386,#39387),(#39388,#39389),(#39390,#39391),(#39392,
#39393),(#39394,#39395),(#39396,#39397),(#39398,#39399),(#39400,#39401),
(#39402,#39403),(#39404,#39405),(#39406,#39407),(#39408,#39409),(#39410,
#39411),(#39412,#39413),(#39414,#39415),(#39416,#39417),(#39418,#39419)),
 .UNSPECIFIED.,.F.,.F.,.F.)
B_SPLINE_SURFACE_WITH_KNOTS((6,1,1,1,1,1,1,1,1,1,1,1,1,1,1,1,1,1,1,1,1,
1,1,1,1,1,1,1,1,1,6),(2,2),(-1.,-0.966666666666667,-0.933333333333333,-0.9,
-0.866666666666667,-0.833333333333333,-0.8,-0.766666666666667,-0.733333333333333,
-0.7,-0.666666666666667,-0.633333333333333,-0.6,-0.566666666666667,-0.533333333333333,
-0.5,-0.466666666666667,-0.433333333333333,-0.4,-0.366666666666667,-0.333333333333333,
-0.3,-0.266666666666667,-0.233333333333333,-0.2,-0.166666666666667,-0.133333333333333,
-0.1,-0.0666666666666667,-0.0333333333333333,0.),(-5.,5.),.UNSPECIFIED.)
GEOMETRIC_REPRESENTATION_ITEM()
RATIONAL_B_SPLINE_SURFACE(((1.,1.),(1.,1.),(1.,1.),(1.,1.),(1.,1.),(1.,
1.),(1.,1.),(1.,1.),(1.,1.),(1.,1.),(1.,1.),(1.,1.),(1.,1.),(1.,1.),(1.,
1.),(1.,1.),(1.,1.),(1.,1.),(1.,1.),(1.,1.),(1.,1.),(1.,1.),(1.,1.),(1.,
1.),(1.,1.),(1.,1.),(1.,1.),(1.,1.),(1.,1.),(1.,1.),(1.,1.),(1.,1.),(1.,
1.),(1.,1.),(1.,1.)))
REPRESENTATION_ITEM('')
SURFACE()
);
#507=(
BOUNDED_SURFACE()
B_SPLINE_SURFACE(5,1,((#39431,#39432),(#39433,#39434),(#39435,#39436),(#39437,
#39438),(#39439,#39440),(#39441,#39442),(#39443,#39444),(#39445,#39446),
(#39447,#39448),(#39449,#39450),(#39451,#39452),(#39453,#39454),(#39455,
#39456),(#39457,#39458),(#39459,#39460),(#39461,#39462),(#39463,#39464),
(#39465,#39466),(#39467,#39468),(#39469,#39470),(#39471,#39472),(#39473,
#39474),(#39475,#39476),(#39477,#39478),(#39479,#39480),(#39481,#39482),
(#39483,#39484),(#39485,#39486),(#39487,#39488),(#39489,#39490),(#39491,
#39492),(#39493,#39494),(#39495,#39496),(#39497,#39498),(#39499,#39500)),
 .UNSPECIFIED.,.F.,.F.,.F.)
B_SPLINE_SURFACE_WITH_KNOTS((6,1,1,1,1,1,1,1,1,1,1,1,1,1,1,1,1,1,1,1,1,
1,1,1,1,1,1,1,1,1,6),(2,2),(0.,0.0333333333333333,0.0666666666666667,0.1,
0.133333333333333,0.166666666666667,0.2,0.233333333333333,0.266666666666667,
0.3,0.333333333333333,0.366666666666667,0.4,0.433333333333333,0.466666666666667,
0.5,0.533333333333333,0.566666666666667,0.6,0.633333333333333,0.666666666666667,
0.7,0.733333333333333,0.766666666666667,0.8,0.833333333333333,0.866666666666667,
0.9,0.933333333333333,0.966666666666667,1.),(-5.,5.),.UNSPECIFIED.)
GEOMETRIC_REPRESENTATION_ITEM()
RATIONAL_B_SPLINE_SURFACE(((1.,1.),(1.,1.),(1.,1.),(1.,1.),(1.,1.),(1.,
1.),(1.,1.),(1.,1.),(1.,1.),(1.,1.),(1.,1.),(1.,1.),(1.,1.),(1.,1.),(1.,
1.),(1.,1.),(1.,1.),(1.,1.),(1.,1.),(1.,1.),(1.,1.),(1.,1.),(1.,1.),(1.,
1.),(1.,1.),(1.,1.),(1.,1.),(1.,1.),(1.,1.),(1.,1.),(1.,1.),(1.,1.),(1.,
1.),(1.,1.),(1.,1.)))
REPRESENTATION_ITEM('')
SURFACE()
);
#508=(
BOUNDED_SURFACE()
B_SPLINE_SURFACE(5,1,((#39509,#39510),(#39511,#39512),(#39513,#39514),(#39515,
#39516),(#39517,#39518),(#39519,#39520),(#39521,#39522),(#39523,#39524),
(#39525,#39526),(#39527,#39528),(#39529,#39530),(#39531,#39532),(#39533,
#39534),(#39535,#39536),(#39537,#39538),(#39539,#39540),(#39541,#39542),
(#39543,#39544),(#39545,#39546),(#39547,#39548),(#39549,#39550),(#39551,
#39552),(#39553,#39554),(#39555,#39556),(#39557,#39558),(#39559,#39560),
(#39561,#39562),(#39563,#39564),(#39565,#39566),(#39567,#39568),(#39569,
#39570),(#39571,#39572),(#39573,#39574),(#39575,#39576),(#39577,#39578)),
 .UNSPECIFIED.,.F.,.F.,.F.)
B_SPLINE_SURFACE_WITH_KNOTS((6,1,1,1,1,1,1,1,1,1,1,1,1,1,1,1,1,1,1,1,1,
1,1,1,1,1,1,1,1,1,6),(2,2),(-1.,-0.966666666666667,-0.933333333333333,-0.9,
-0.866666666666667,-0.833333333333333,-0.8,-0.766666666666667,-0.733333333333333,
-0.7,-0.666666666666667,-0.633333333333333,-0.6,-0.566666666666667,-0.533333333333333,
-0.5,-0.466666666666667,-0.433333333333333,-0.4,-0.366666666666667,-0.333333333333333,
-0.3,-0.266666666666667,-0.233333333333333,-0.2,-0.166666666666667,-0.133333333333333,
-0.1,-0.0666666666666667,-0.0333333333333333,0.),(-5.,5.),.UNSPECIFIED.)
GEOMETRIC_REPRESENTATION_ITEM()
RATIONAL_B_SPLINE_SURFACE(((1.,1.),(1.,1.),(1.,1.),(1.,1.),(1.,1.),(1.,
1.),(1.,1.),(1.,1.),(1.,1.),(1.,1.),(1.,1.),(1.,1.),(1.,1.),(1.,1.),(1.,
1.),(1.,1.),(1.,1.),(1.,1.),(1.,1.),(1.,1.),(1.,1.),(1.,1.),(1.,1.),(1.,
1.),(1.,1.),(1.,1.),(1.,1.),(1.,1.),(1.,1.),(1.,1.),(1.,1.),(1.,1.),(1.,
1.),(1.,1.),(1.,1.)))
REPRESENTATION_ITEM('')
SURFACE()
);
#509=(
BOUNDED_SURFACE()
B_SPLINE_SURFACE(5,1,((#39590,#39591),(#39592,#39593),(#39594,#39595),(#39596,
#39597),(#39598,#39599),(#39600,#39601),(#39602,#39603),(#39604,#39605),
(#39606,#39607),(#39608,#39609),(#39610,#39611),(#39612,#39613),(#39614,
#39615),(#39616,#39617),(#39618,#39619),(#39620,#39621),(#39622,#39623),
(#39624,#39625),(#39626,#39627),(#39628,#39629),(#39630,#39631),(#39632,
#39633),(#39634,#39635),(#39636,#39637),(#39638,#39639),(#39640,#39641),
(#39642,#39643),(#39644,#39645),(#39646,#39647),(#39648,#39649),(#39650,
#39651),(#39652,#39653),(#39654,#39655),(#39656,#39657),(#39658,#39659)),
 .UNSPECIFIED.,.F.,.F.,.F.)
B_SPLINE_SURFACE_WITH_KNOTS((6,1,1,1,1,1,1,1,1,1,1,1,1,1,1,1,1,1,1,1,1,
1,1,1,1,1,1,1,1,1,6),(2,2),(0.,0.0333333333333333,0.0666666666666667,0.1,
0.133333333333333,0.166666666666667,0.2,0.233333333333333,0.266666666666667,
0.3,0.333333333333333,0.366666666666667,0.4,0.433333333333333,0.466666666666667,
0.5,0.533333333333333,0.566666666666667,0.6,0.633333333333333,0.666666666666667,
0.7,0.733333333333333,0.766666666666667,0.8,0.833333333333333,0.866666666666667,
0.9,0.933333333333333,0.966666666666667,1.),(-5.,5.),.UNSPECIFIED.)
GEOMETRIC_REPRESENTATION_ITEM()
RATIONAL_B_SPLINE_SURFACE(((1.,1.),(1.,1.),(1.,1.),(1.,1.),(1.,1.),(1.,
1.),(1.,1.),(1.,1.),(1.,1.),(1.,1.),(1.,1.),(1.,1.),(1.,1.),(1.,1.),(1.,
1.),(1.,1.),(1.,1.),(1.,1.),(1.,1.),(1.,1.),(1.,1.),(1.,1.),(1.,1.),(1.,
1.),(1.,1.),(1.,1.),(1.,1.),(1.,1.),(1.,1.),(1.,1.),(1.,1.),(1.,1.),(1.,
1.),(1.,1.),(1.,1.)))
REPRESENTATION_ITEM('')
SURFACE()
);
#510=(
BOUNDED_SURFACE()
B_SPLINE_SURFACE(5,1,((#39668,#39669),(#39670,#39671),(#39672,#39673),(#39674,
#39675),(#39676,#39677),(#39678,#39679),(#39680,#39681),(#39682,#39683),
(#39684,#39685),(#39686,#39687),(#39688,#39689),(#39690,#39691),(#39692,
#39693),(#39694,#39695),(#39696,#39697),(#39698,#39699),(#39700,#39701),
(#39702,#39703),(#39704,#39705),(#39706,#39707),(#39708,#39709),(#39710,
#39711),(#39712,#39713),(#39714,#39715),(#39716,#39717),(#39718,#39719),
(#39720,#39721),(#39722,#39723),(#39724,#39725),(#39726,#39727),(#39728,
#39729),(#39730,#39731),(#39732,#39733),(#39734,#39735),(#39736,#39737)),
 .UNSPECIFIED.,.F.,.F.,.F.)
B_SPLINE_SURFACE_WITH_KNOTS((6,1,1,1,1,1,1,1,1,1,1,1,1,1,1,1,1,1,1,1,1,
1,1,1,1,1,1,1,1,1,6),(2,2),(-1.,-0.966666666666667,-0.933333333333333,-0.9,
-0.866666666666667,-0.833333333333333,-0.8,-0.766666666666667,-0.733333333333333,
-0.7,-0.666666666666667,-0.633333333333333,-0.6,-0.566666666666667,-0.533333333333333,
-0.5,-0.466666666666667,-0.433333333333333,-0.4,-0.366666666666667,-0.333333333333333,
-0.3,-0.266666666666667,-0.233333333333333,-0.2,-0.166666666666667,-0.133333333333333,
-0.1,-0.0666666666666667,-0.0333333333333333,0.),(-5.,5.),.UNSPECIFIED.)
GEOMETRIC_REPRESENTATION_ITEM()
RATIONAL_B_SPLINE_SURFACE(((1.,1.),(1.,1.),(1.,1.),(1.,1.),(1.,1.),(1.,
1.),(1.,1.),(1.,1.),(1.,1.),(1.,1.),(1.,1.),(1.,1.),(1.,1.),(1.,1.),(1.,
1.),(1.,1.),(1.,1.),(1.,1.),(1.,1.),(1.,1.),(1.,1.),(1.,1.),(1.,1.),(1.,
1.),(1.,1.),(1.,1.),(1.,1.),(1.,1.),(1.,1.),(1.,1.),(1.,1.),(1.,1.),(1.,
1.),(1.,1.),(1.,1.)))
REPRESENTATION_ITEM('')
SURFACE()
);
#511=(
BOUNDED_SURFACE()
B_SPLINE_SURFACE(5,1,((#39749,#39750),(#39751,#39752),(#39753,#39754),(#39755,
#39756),(#39757,#39758),(#39759,#39760),(#39761,#39762),(#39763,#39764),
(#39765,#39766),(#39767,#39768),(#39769,#39770),(#39771,#39772),(#39773,
#39774),(#39775,#39776),(#39777,#39778),(#39779,#39780),(#39781,#39782),
(#39783,#39784),(#39785,#39786),(#39787,#39788),(#39789,#39790),(#39791,
#39792),(#39793,#39794),(#39795,#39796),(#39797,#39798),(#39799,#39800),
(#39801,#39802),(#39803,#39804),(#39805,#39806),(#39807,#39808),(#39809,
#39810),(#39811,#39812),(#39813,#39814),(#39815,#39816),(#39817,#39818)),
 .UNSPECIFIED.,.F.,.F.,.F.)
B_SPLINE_SURFACE_WITH_KNOTS((6,1,1,1,1,1,1,1,1,1,1,1,1,1,1,1,1,1,1,1,1,
1,1,1,1,1,1,1,1,1,6),(2,2),(0.,0.0333333333333333,0.0666666666666667,0.1,
0.133333333333333,0.166666666666667,0.2,0.233333333333333,0.266666666666667,
0.3,0.333333333333333,0.366666666666667,0.4,0.433333333333333,0.466666666666667,
0.5,0.533333333333333,0.566666666666667,0.6,0.633333333333333,0.666666666666667,
0.7,0.733333333333333,0.766666666666667,0.8,0.833333333333333,0.866666666666667,
0.9,0.933333333333333,0.966666666666667,1.),(-5.,5.),.UNSPECIFIED.)
GEOMETRIC_REPRESENTATION_ITEM()
RATIONAL_B_SPLINE_SURFACE(((1.,1.),(1.,1.),(1.,1.),(1.,1.),(1.,1.),(1.,
1.),(1.,1.),(1.,1.),(1.,1.),(1.,1.),(1.,1.),(1.,1.),(1.,1.),(1.,1.),(1.,
1.),(1.,1.),(1.,1.),(1.,1.),(1.,1.),(1.,1.),(1.,1.),(1.,1.),(1.,1.),(1.,
1.),(1.,1.),(1.,1.),(1.,1.),(1.,1.),(1.,1.),(1.,1.),(1.,1.),(1.,1.),(1.,
1.),(1.,1.),(1.,1.)))
REPRESENTATION_ITEM('')
SURFACE()
);
#512=(
BOUNDED_SURFACE()
B_SPLINE_SURFACE(5,1,((#39827,#39828),(#39829,#39830),(#39831,#39832),(#39833,
#39834),(#39835,#39836),(#39837,#39838),(#39839,#39840),(#39841,#39842),
(#39843,#39844),(#39845,#39846),(#39847,#39848),(#39849,#39850),(#39851,
#39852),(#39853,#39854),(#39855,#39856),(#39857,#39858),(#39859,#39860),
(#39861,#39862),(#39863,#39864),(#39865,#39866),(#39867,#39868),(#39869,
#39870),(#39871,#39872),(#39873,#39874),(#39875,#39876),(#39877,#39878),
(#39879,#39880),(#39881,#39882),(#39883,#39884),(#39885,#39886),(#39887,
#39888),(#39889,#39890),(#39891,#39892),(#39893,#39894),(#39895,#39896)),
 .UNSPECIFIED.,.F.,.F.,.F.)
B_SPLINE_SURFACE_WITH_KNOTS((6,1,1,1,1,1,1,1,1,1,1,1,1,1,1,1,1,1,1,1,1,
1,1,1,1,1,1,1,1,1,6),(2,2),(-1.,-0.966666666666667,-0.933333333333333,-0.9,
-0.866666666666667,-0.833333333333333,-0.8,-0.766666666666667,-0.733333333333333,
-0.7,-0.666666666666667,-0.633333333333333,-0.6,-0.566666666666667,-0.533333333333333,
-0.5,-0.466666666666667,-0.433333333333333,-0.4,-0.366666666666667,-0.333333333333333,
-0.3,-0.266666666666667,-0.233333333333333,-0.2,-0.166666666666667,-0.133333333333333,
-0.1,-0.0666666666666667,-0.0333333333333333,0.),(-5.,5.),.UNSPECIFIED.)
GEOMETRIC_REPRESENTATION_ITEM()
RATIONAL_B_SPLINE_SURFACE(((1.,1.),(1.,1.),(1.,1.),(1.,1.),(1.,1.),(1.,
1.),(1.,1.),(1.,1.),(1.,1.),(1.,1.),(1.,1.),(1.,1.),(1.,1.),(1.,1.),(1.,
1.),(1.,1.),(1.,1.),(1.,1.),(1.,1.),(1.,1.),(1.,1.),(1.,1.),(1.,1.),(1.,
1.),(1.,1.),(1.,1.),(1.,1.),(1.,1.),(1.,1.),(1.,1.),(1.,1.),(1.,1.),(1.,
1.),(1.,1.),(1.,1.)))
REPRESENTATION_ITEM('')
SURFACE()
);
#513=(
BOUNDED_SURFACE()
B_SPLINE_SURFACE(5,1,((#39908,#39909),(#39910,#39911),(#39912,#39913),(#39914,
#39915),(#39916,#39917),(#39918,#39919),(#39920,#39921),(#39922,#39923),
(#39924,#39925),(#39926,#39927),(#39928,#39929),(#39930,#39931),(#39932,
#39933),(#39934,#39935),(#39936,#39937),(#39938,#39939),(#39940,#39941),
(#39942,#39943),(#39944,#39945),(#39946,#39947),(#39948,#39949),(#39950,
#39951),(#39952,#39953),(#39954,#39955),(#39956,#39957),(#39958,#39959),
(#39960,#39961),(#39962,#39963),(#39964,#39965),(#39966,#39967),(#39968,
#39969),(#39970,#39971),(#39972,#39973),(#39974,#39975),(#39976,#39977)),
 .UNSPECIFIED.,.F.,.F.,.F.)
B_SPLINE_SURFACE_WITH_KNOTS((6,1,1,1,1,1,1,1,1,1,1,1,1,1,1,1,1,1,1,1,1,
1,1,1,1,1,1,1,1,1,6),(2,2),(0.,0.0333333333333333,0.0666666666666667,0.1,
0.133333333333333,0.166666666666667,0.2,0.233333333333333,0.266666666666667,
0.3,0.333333333333333,0.366666666666667,0.4,0.433333333333333,0.466666666666667,
0.5,0.533333333333333,0.566666666666667,0.6,0.633333333333333,0.666666666666667,
0.7,0.733333333333333,0.766666666666667,0.8,0.833333333333333,0.866666666666667,
0.9,0.933333333333333,0.966666666666667,1.),(-5.,5.),.UNSPECIFIED.)
GEOMETRIC_REPRESENTATION_ITEM()
RATIONAL_B_SPLINE_SURFACE(((1.,1.),(1.,1.),(1.,1.),(1.,1.),(1.,1.),(1.,
1.),(1.,1.),(1.,1.),(1.,1.),(1.,1.),(1.,1.),(1.,1.),(1.,1.),(1.,1.),(1.,
1.),(1.,1.),(1.,1.),(1.,1.),(1.,1.),(1.,1.),(1.,1.),(1.,1.),(1.,1.),(1.,
1.),(1.,1.),(1.,1.),(1.,1.),(1.,1.),(1.,1.),(1.,1.),(1.,1.),(1.,1.),(1.,
1.),(1.,1.),(1.,1.)))
REPRESENTATION_ITEM('')
SURFACE()
);
#514=(
BOUNDED_SURFACE()
B_SPLINE_SURFACE(5,1,((#39986,#39987),(#39988,#39989),(#39990,#39991),(#39992,
#39993),(#39994,#39995),(#39996,#39997),(#39998,#39999),(#40000,#40001),
(#40002,#40003),(#40004,#40005),(#40006,#40007),(#40008,#40009),(#40010,
#40011),(#40012,#40013),(#40014,#40015),(#40016,#40017),(#40018,#40019),
(#40020,#40021),(#40022,#40023),(#40024,#40025),(#40026,#40027),(#40028,
#40029),(#40030,#40031),(#40032,#40033),(#40034,#40035),(#40036,#40037),
(#40038,#40039),(#40040,#40041),(#40042,#40043),(#40044,#40045),(#40046,
#40047),(#40048,#40049),(#40050,#40051),(#40052,#40053),(#40054,#40055)),
 .UNSPECIFIED.,.F.,.F.,.F.)
B_SPLINE_SURFACE_WITH_KNOTS((6,1,1,1,1,1,1,1,1,1,1,1,1,1,1,1,1,1,1,1,1,
1,1,1,1,1,1,1,1,1,6),(2,2),(-1.,-0.966666666666667,-0.933333333333333,-0.9,
-0.866666666666667,-0.833333333333333,-0.8,-0.766666666666667,-0.733333333333333,
-0.7,-0.666666666666667,-0.633333333333333,-0.6,-0.566666666666667,-0.533333333333333,
-0.5,-0.466666666666667,-0.433333333333333,-0.4,-0.366666666666667,-0.333333333333333,
-0.3,-0.266666666666667,-0.233333333333333,-0.2,-0.166666666666667,-0.133333333333333,
-0.1,-0.0666666666666667,-0.0333333333333333,0.),(-5.,5.),.UNSPECIFIED.)
GEOMETRIC_REPRESENTATION_ITEM()
RATIONAL_B_SPLINE_SURFACE(((1.,1.),(1.,1.),(1.,1.),(1.,1.),(1.,1.),(1.,
1.),(1.,1.),(1.,1.),(1.,1.),(1.,1.),(1.,1.),(1.,1.),(1.,1.),(1.,1.),(1.,
1.),(1.,1.),(1.,1.),(1.,1.),(1.,1.),(1.,1.),(1.,1.),(1.,1.),(1.,1.),(1.,
1.),(1.,1.),(1.,1.),(1.,1.),(1.,1.),(1.,1.),(1.,1.),(1.,1.),(1.,1.),(1.,
1.),(1.,1.),(1.,1.)))
REPRESENTATION_ITEM('')
SURFACE()
);
#515=(
BOUNDED_SURFACE()
B_SPLINE_SURFACE(5,1,((#40067,#40068),(#40069,#40070),(#40071,#40072),(#40073,
#40074),(#40075,#40076),(#40077,#40078),(#40079,#40080),(#40081,#40082),
(#40083,#40084),(#40085,#40086),(#40087,#40088),(#40089,#40090),(#40091,
#40092),(#40093,#40094),(#40095,#40096),(#40097,#40098),(#40099,#40100),
(#40101,#40102),(#40103,#40104),(#40105,#40106),(#40107,#40108),(#40109,
#40110),(#40111,#40112),(#40113,#40114),(#40115,#40116),(#40117,#40118),
(#40119,#40120),(#40121,#40122),(#40123,#40124),(#40125,#40126),(#40127,
#40128),(#40129,#40130),(#40131,#40132),(#40133,#40134),(#40135,#40136)),
 .UNSPECIFIED.,.F.,.F.,.F.)
B_SPLINE_SURFACE_WITH_KNOTS((6,1,1,1,1,1,1,1,1,1,1,1,1,1,1,1,1,1,1,1,1,
1,1,1,1,1,1,1,1,1,6),(2,2),(0.,0.0333333333333333,0.0666666666666667,0.1,
0.133333333333333,0.166666666666667,0.2,0.233333333333333,0.266666666666667,
0.3,0.333333333333333,0.366666666666667,0.4,0.433333333333333,0.466666666666667,
0.5,0.533333333333333,0.566666666666667,0.6,0.633333333333333,0.666666666666667,
0.7,0.733333333333333,0.766666666666667,0.8,0.833333333333333,0.866666666666667,
0.9,0.933333333333333,0.966666666666667,1.),(-5.,5.),.UNSPECIFIED.)
GEOMETRIC_REPRESENTATION_ITEM()
RATIONAL_B_SPLINE_SURFACE(((1.,1.),(1.,1.),(1.,1.),(1.,1.),(1.,1.),(1.,
1.),(1.,1.),(1.,1.),(1.,1.),(1.,1.),(1.,1.),(1.,1.),(1.,1.),(1.,1.),(1.,
1.),(1.,1.),(1.,1.),(1.,1.),(1.,1.),(1.,1.),(1.,1.),(1.,1.),(1.,1.),(1.,
1.),(1.,1.),(1.,1.),(1.,1.),(1.,1.),(1.,1.),(1.,1.),(1.,1.),(1.,1.),(1.,
1.),(1.,1.),(1.,1.)))
REPRESENTATION_ITEM('')
SURFACE()
);
#516=(
BOUNDED_SURFACE()
B_SPLINE_SURFACE(5,1,((#40145,#40146),(#40147,#40148),(#40149,#40150),(#40151,
#40152),(#40153,#40154),(#40155,#40156),(#40157,#40158),(#40159,#40160),
(#40161,#40162),(#40163,#40164),(#40165,#40166),(#40167,#40168),(#40169,
#40170),(#40171,#40172),(#40173,#40174),(#40175,#40176),(#40177,#40178),
(#40179,#40180),(#40181,#40182),(#40183,#40184),(#40185,#40186),(#40187,
#40188),(#40189,#40190),(#40191,#40192),(#40193,#40194),(#40195,#40196),
(#40197,#40198),(#40199,#40200),(#40201,#40202),(#40203,#40204),(#40205,
#40206),(#40207,#40208),(#40209,#40210),(#40211,#40212),(#40213,#40214)),
 .UNSPECIFIED.,.F.,.F.,.F.)
B_SPLINE_SURFACE_WITH_KNOTS((6,1,1,1,1,1,1,1,1,1,1,1,1,1,1,1,1,1,1,1,1,
1,1,1,1,1,1,1,1,1,6),(2,2),(-1.,-0.966666666666667,-0.933333333333333,-0.9,
-0.866666666666667,-0.833333333333333,-0.8,-0.766666666666667,-0.733333333333333,
-0.7,-0.666666666666667,-0.633333333333333,-0.6,-0.566666666666667,-0.533333333333333,
-0.5,-0.466666666666667,-0.433333333333333,-0.4,-0.366666666666667,-0.333333333333333,
-0.3,-0.266666666666667,-0.233333333333333,-0.2,-0.166666666666667,-0.133333333333333,
-0.1,-0.0666666666666667,-0.0333333333333333,0.),(-5.,5.),.UNSPECIFIED.)
GEOMETRIC_REPRESENTATION_ITEM()
RATIONAL_B_SPLINE_SURFACE(((1.,1.),(1.,1.),(1.,1.),(1.,1.),(1.,1.),(1.,
1.),(1.,1.),(1.,1.),(1.,1.),(1.,1.),(1.,1.),(1.,1.),(1.,1.),(1.,1.),(1.,
1.),(1.,1.),(1.,1.),(1.,1.),(1.,1.),(1.,1.),(1.,1.),(1.,1.),(1.,1.),(1.,
1.),(1.,1.),(1.,1.),(1.,1.),(1.,1.),(1.,1.),(1.,1.),(1.,1.),(1.,1.),(1.,
1.),(1.,1.),(1.,1.)))
REPRESENTATION_ITEM('')
SURFACE()
);
#517=(
BOUNDED_SURFACE()
B_SPLINE_SURFACE(5,1,((#40226,#40227),(#40228,#40229),(#40230,#40231),(#40232,
#40233),(#40234,#40235),(#40236,#40237),(#40238,#40239),(#40240,#40241),
(#40242,#40243),(#40244,#40245),(#40246,#40247),(#40248,#40249),(#40250,
#40251),(#40252,#40253),(#40254,#40255),(#40256,#40257),(#40258,#40259),
(#40260,#40261),(#40262,#40263),(#40264,#40265),(#40266,#40267),(#40268,
#40269),(#40270,#40271),(#40272,#40273),(#40274,#40275),(#40276,#40277),
(#40278,#40279),(#40280,#40281),(#40282,#40283),(#40284,#40285),(#40286,
#40287),(#40288,#40289),(#40290,#40291),(#40292,#40293),(#40294,#40295)),
 .UNSPECIFIED.,.F.,.F.,.F.)
B_SPLINE_SURFACE_WITH_KNOTS((6,1,1,1,1,1,1,1,1,1,1,1,1,1,1,1,1,1,1,1,1,
1,1,1,1,1,1,1,1,1,6),(2,2),(0.,0.0333333333333333,0.0666666666666667,0.1,
0.133333333333333,0.166666666666667,0.2,0.233333333333333,0.266666666666667,
0.3,0.333333333333333,0.366666666666667,0.4,0.433333333333333,0.466666666666667,
0.5,0.533333333333333,0.566666666666667,0.6,0.633333333333333,0.666666666666667,
0.7,0.733333333333333,0.766666666666667,0.8,0.833333333333333,0.866666666666667,
0.9,0.933333333333333,0.966666666666667,1.),(-5.,5.),.UNSPECIFIED.)
GEOMETRIC_REPRESENTATION_ITEM()
RATIONAL_B_SPLINE_SURFACE(((1.,1.),(1.,1.),(1.,1.),(1.,1.),(1.,1.),(1.,
1.),(1.,1.),(1.,1.),(1.,1.),(1.,1.),(1.,1.),(1.,1.),(1.,1.),(1.,1.),(1.,
1.),(1.,1.),(1.,1.),(1.,1.),(1.,1.),(1.,1.),(1.,1.),(1.,1.),(1.,1.),(1.,
1.),(1.,1.),(1.,1.),(1.,1.),(1.,1.),(1.,1.),(1.,1.),(1.,1.),(1.,1.),(1.,
1.),(1.,1.),(1.,1.)))
REPRESENTATION_ITEM('')
SURFACE()
);
#518=CYLINDRICAL_SURFACE('',#27096,6.25);
#519=CYLINDRICAL_SURFACE('',#27139,6.25);
#520=CYLINDRICAL_SURFACE('',#27145,3.);
#521=CYLINDRICAL_SURFACE('',#27154,3.);
#522=CYLINDRICAL_SURFACE('',#27159,4.64999999999896);
#523=CYLINDRICAL_SURFACE('',#27162,4.6500000000015);
#524=CYLINDRICAL_SURFACE('',#27165,4.64999999999968);
#525=CYLINDRICAL_SURFACE('',#27168,4.64999999999928);
#526=CYLINDRICAL_SURFACE('',#27171,4.6500000000004);
#527=CYLINDRICAL_SURFACE('',#27174,4.64999999999845);
#528=CYLINDRICAL_SURFACE('',#27177,4.64999999999964);
#529=CYLINDRICAL_SURFACE('',#27180,4.64999999999968);
#530=CYLINDRICAL_SURFACE('',#27183,4.64999999999896);
#531=CYLINDRICAL_SURFACE('',#27186,4.64999999999943);
#532=CYLINDRICAL_SURFACE('',#27189,4.64999999999985);
#533=CYLINDRICAL_SURFACE('',#27192,4.65000000000067);
#534=CYLINDRICAL_SURFACE('',#27195,4.65000000000029);
#535=CYLINDRICAL_SURFACE('',#27198,4.65000000000076);
#536=CYLINDRICAL_SURFACE('',#27201,4.6499999999995);
#537=CYLINDRICAL_SURFACE('',#27204,4.64999999999985);
#538=CYLINDRICAL_SURFACE('',#27207,4.65000000000067);
#539=CYLINDRICAL_SURFACE('',#27210,4.65000000000016);
#540=CYLINDRICAL_SURFACE('',#27213,6.);
#541=CYLINDRICAL_SURFACE('',#27214,6.);
#542=CYLINDRICAL_SURFACE('',#27215,6.);
#543=CYLINDRICAL_SURFACE('',#27216,6.);
#544=CYLINDRICAL_SURFACE('',#27217,6.);
#545=CYLINDRICAL_SURFACE('',#27218,6.);
#546=CYLINDRICAL_SURFACE('',#27219,6.);
#547=CYLINDRICAL_SURFACE('',#27220,6.);
#548=CYLINDRICAL_SURFACE('',#27221,6.);
#549=CYLINDRICAL_SURFACE('',#27222,6.);
#550=CYLINDRICAL_SURFACE('',#27223,6.);
#551=CYLINDRICAL_SURFACE('',#27224,6.);
#552=CYLINDRICAL_SURFACE('',#27225,6.);
#553=CYLINDRICAL_SURFACE('',#27226,6.);
#554=CYLINDRICAL_SURFACE('',#27227,6.);
#555=CYLINDRICAL_SURFACE('',#27228,6.);
#556=CYLINDRICAL_SURFACE('',#27229,6.);
#557=CYLINDRICAL_SURFACE('',#27230,6.);
#558=CYLINDRICAL_SURFACE('',#27232,1.188225);
#559=CYLINDRICAL_SURFACE('',#27234,1.188225);
#560=CYLINDRICAL_SURFACE('',#27235,1.188225);
#561=CYLINDRICAL_SURFACE('',#27236,1.188225);
#562=CYLINDRICAL_SURFACE('',#27237,1.188225);
#563=CYLINDRICAL_SURFACE('',#27238,1.188225);
#564=CYLINDRICAL_SURFACE('',#27239,1.188225);
#565=CYLINDRICAL_SURFACE('',#27240,1.188225);
#566=CYLINDRICAL_SURFACE('',#27241,1.188225);
#567=CYLINDRICAL_SURFACE('',#27242,1.188225);
#568=CYLINDRICAL_SURFACE('',#27243,1.188225);
#569=CYLINDRICAL_SURFACE('',#27244,1.188225);
#570=CYLINDRICAL_SURFACE('',#27245,1.188225);
#571=CYLINDRICAL_SURFACE('',#27246,1.016475);
#572=CYLINDRICAL_SURFACE('',#27248,1.016475);
#573=CYLINDRICAL_SURFACE('',#27250,1.016475);
#574=CYLINDRICAL_SURFACE('',#27251,1.016475);
#575=CYLINDRICAL_SURFACE('',#27252,1.016475);
#576=CYLINDRICAL_SURFACE('',#27253,1.016475);
#577=CYLINDRICAL_SURFACE('',#27254,1.016475);
#578=CYLINDRICAL_SURFACE('',#27255,1.016475);
#579=CYLINDRICAL_SURFACE('',#27256,1.016475);
#580=CYLINDRICAL_SURFACE('',#27257,1.016475);
#581=CYLINDRICAL_SURFACE('',#27258,1.016475);
#582=CYLINDRICAL_SURFACE('',#27259,1.016475);
#583=CYLINDRICAL_SURFACE('',#27260,1.016475);
#584=CYLINDRICAL_SURFACE('',#27268,1.016475);
#585=CYLINDRICAL_SURFACE('',#27269,1.188225);
#586=CYLINDRICAL_SURFACE('',#27275,2.);
#587=CYLINDRICAL_SURFACE('',#27285,15.75);
#588=CYLINDRICAL_SURFACE('',#27319,2.75);
#589=CYLINDRICAL_SURFACE('',#27324,2.005);
#590=CYLINDRICAL_SURFACE('',#27331,15.75);
#591=CYLINDRICAL_SURFACE('',#27338,2.);
#592=CYLINDRICAL_SURFACE('',#27346,15.75);
#593=CYLINDRICAL_SURFACE('',#27351,3.5);
#594=CYLINDRICAL_SURFACE('',#27382,1.25);
#595=CYLINDRICAL_SURFACE('',#27386,15.75);
#596=CYLINDRICAL_SURFACE('',#27394,2.);
#597=CYLINDRICAL_SURFACE('',#27400,0.805);
#598=CYLINDRICAL_SURFACE('',#27401,7.5);
#599=CYLINDRICAL_SURFACE('',#27404,3.0025);
#600=CYLINDRICAL_SURFACE('',#27416,1.49999999999999);
#601=CYLINDRICAL_SURFACE('',#27417,1.5);
#602=CYLINDRICAL_SURFACE('',#27418,1.5);
#603=CYLINDRICAL_SURFACE('',#27419,1.5);
#604=CYLINDRICAL_SURFACE('',#27420,1.5);
#605=CYLINDRICAL_SURFACE('',#27421,1.5);
#606=CYLINDRICAL_SURFACE('',#27433,0.989525);
#607=CYLINDRICAL_SURFACE('',#27435,0.989525);
#608=CYLINDRICAL_SURFACE('',#27436,0.989525);
#609=CYLINDRICAL_SURFACE('',#27437,0.989525);
#610=CYLINDRICAL_SURFACE('',#27438,0.989525);
#611=CYLINDRICAL_SURFACE('',#27439,0.989525);
#612=CYLINDRICAL_SURFACE('',#27440,0.989525);
#613=CYLINDRICAL_SURFACE('',#27441,0.8469);
#614=CYLINDRICAL_SURFACE('',#27443,0.8469);
#615=CYLINDRICAL_SURFACE('',#27445,0.8469);
#616=CYLINDRICAL_SURFACE('',#27446,0.8469);
#617=CYLINDRICAL_SURFACE('',#27447,0.8469);
#618=CYLINDRICAL_SURFACE('',#27448,0.8469);
#619=CYLINDRICAL_SURFACE('',#27449,0.8469);
#620=CYLINDRICAL_SURFACE('',#27457,0.8469);
#621=CYLINDRICAL_SURFACE('',#27505,0.989525);
#622=CYLINDRICAL_SURFACE('',#27548,0.7911);
#623=CYLINDRICAL_SURFACE('',#27550,0.7911);
#624=CYLINDRICAL_SURFACE('',#27551,0.7911);
#625=CYLINDRICAL_SURFACE('',#27552,0.7911);
#626=CYLINDRICAL_SURFACE('',#27553,0.7911);
#627=CYLINDRICAL_SURFACE('',#27554,0.7911);
#628=CYLINDRICAL_SURFACE('',#27555,0.7911);
#629=CYLINDRICAL_SURFACE('',#27556,0.7911);
#630=CYLINDRICAL_SURFACE('',#27557,0.7911);
#631=CYLINDRICAL_SURFACE('',#27558,0.7911);
#632=CYLINDRICAL_SURFACE('',#27559,0.7911);
#633=CYLINDRICAL_SURFACE('',#27560,0.7911);
#634=CYLINDRICAL_SURFACE('',#27561,0.7911);
#635=CYLINDRICAL_SURFACE('',#27562,0.7911);
#636=CYLINDRICAL_SURFACE('',#27563,0.7911);
#637=CYLINDRICAL_SURFACE('',#27564,0.7911);
#638=CYLINDRICAL_SURFACE('',#27565,0.7911);
#639=CYLINDRICAL_SURFACE('',#27566,0.7911);
#640=CYLINDRICAL_SURFACE('',#27567,0.7911);
#641=CYLINDRICAL_SURFACE('',#27568,0.7911);
#642=CYLINDRICAL_SURFACE('',#27569,0.7911);
#643=CYLINDRICAL_SURFACE('',#27570,0.7911);
#644=CYLINDRICAL_SURFACE('',#27571,0.7911);
#645=CYLINDRICAL_SURFACE('',#27572,0.7911);
#646=CYLINDRICAL_SURFACE('',#27573,0.7911);
#647=CYLINDRICAL_SURFACE('',#27574,0.7911);
#648=CYLINDRICAL_SURFACE('',#27575,0.7911);
#649=CYLINDRICAL_SURFACE('',#27576,0.7911);
#650=CYLINDRICAL_SURFACE('',#27577,0.7911);
#651=CYLINDRICAL_SURFACE('',#27578,0.6767);
#652=CYLINDRICAL_SURFACE('',#27580,0.6767);
#653=CYLINDRICAL_SURFACE('',#27582,0.6767);
#654=CYLINDRICAL_SURFACE('',#27583,0.6767);
#655=CYLINDRICAL_SURFACE('',#27584,0.6767);
#656=CYLINDRICAL_SURFACE('',#27585,0.6767);
#657=CYLINDRICAL_SURFACE('',#27586,0.6767);
#658=CYLINDRICAL_SURFACE('',#27587,0.6767);
#659=CYLINDRICAL_SURFACE('',#27588,0.6767);
#660=CYLINDRICAL_SURFACE('',#27589,0.6767);
#661=CYLINDRICAL_SURFACE('',#27590,0.6767);
#662=CYLINDRICAL_SURFACE('',#27591,0.6767);
#663=CYLINDRICAL_SURFACE('',#27592,0.6767);
#664=CYLINDRICAL_SURFACE('',#27593,0.6767);
#665=CYLINDRICAL_SURFACE('',#27594,0.6767);
#666=CYLINDRICAL_SURFACE('',#27595,0.6767);
#667=CYLINDRICAL_SURFACE('',#27596,0.6767);
#668=CYLINDRICAL_SURFACE('',#27597,0.6767);
#669=CYLINDRICAL_SURFACE('',#27598,0.6767);
#670=CYLINDRICAL_SURFACE('',#27599,0.6767);
#671=CYLINDRICAL_SURFACE('',#27600,0.6767);
#672=CYLINDRICAL_SURFACE('',#27601,0.6767);
#673=CYLINDRICAL_SURFACE('',#27602,0.6767);
#674=CYLINDRICAL_SURFACE('',#27603,0.6767);
#675=CYLINDRICAL_SURFACE('',#27604,0.6767);
#676=CYLINDRICAL_SURFACE('',#27605,0.6767);
#677=CYLINDRICAL_SURFACE('',#27606,0.6767);
#678=CYLINDRICAL_SURFACE('',#27607,0.6767);
#679=CYLINDRICAL_SURFACE('',#27608,0.6767);
#680=CYLINDRICAL_SURFACE('',#27616,0.6767);
#681=CYLINDRICAL_SURFACE('',#27664,0.7911);
#682=CYLINDRICAL_SURFACE('',#27673,0.805);
#683=CYLINDRICAL_SURFACE('',#27690,0.7911);
#684=CYLINDRICAL_SURFACE('',#27692,0.7911);
#685=CYLINDRICAL_SURFACE('',#27693,0.7911);
#686=CYLINDRICAL_SURFACE('',#27694,0.7911);
#687=CYLINDRICAL_SURFACE('',#27695,0.7911);
#688=CYLINDRICAL_SURFACE('',#27696,0.7911);
#689=CYLINDRICAL_SURFACE('',#27697,0.7911);
#690=CYLINDRICAL_SURFACE('',#27698,0.7911);
#691=CYLINDRICAL_SURFACE('',#27699,0.7911);
#692=CYLINDRICAL_SURFACE('',#27700,0.7911);
#693=CYLINDRICAL_SURFACE('',#27701,0.7911);
#694=CYLINDRICAL_SURFACE('',#27702,0.7911);
#695=CYLINDRICAL_SURFACE('',#27703,0.7911);
#696=CYLINDRICAL_SURFACE('',#27704,0.7911);
#697=CYLINDRICAL_SURFACE('',#27705,0.7911);
#698=CYLINDRICAL_SURFACE('',#27706,0.7911);
#699=CYLINDRICAL_SURFACE('',#27707,0.7911);
#700=CYLINDRICAL_SURFACE('',#27708,0.7911);
#701=CYLINDRICAL_SURFACE('',#27709,0.7911);
#702=CYLINDRICAL_SURFACE('',#27710,0.6767);
#703=CYLINDRICAL_SURFACE('',#27712,0.6767);
#704=CYLINDRICAL_SURFACE('',#27714,0.6767);
#705=CYLINDRICAL_SURFACE('',#27715,0.6767);
#706=CYLINDRICAL_SURFACE('',#27716,0.6767);
#707=CYLINDRICAL_SURFACE('',#27717,0.6767);
#708=CYLINDRICAL_SURFACE('',#27718,0.6767);
#709=CYLINDRICAL_SURFACE('',#27719,0.6767);
#710=CYLINDRICAL_SURFACE('',#27720,0.6767);
#711=CYLINDRICAL_SURFACE('',#27721,0.6767);
#712=CYLINDRICAL_SURFACE('',#27722,0.6767);
#713=CYLINDRICAL_SURFACE('',#27723,0.6767);
#714=CYLINDRICAL_SURFACE('',#27724,0.6767);
#715=CYLINDRICAL_SURFACE('',#27725,0.6767);
#716=CYLINDRICAL_SURFACE('',#27726,0.6767);
#717=CYLINDRICAL_SURFACE('',#27727,0.6767);
#718=CYLINDRICAL_SURFACE('',#27728,0.6767);
#719=CYLINDRICAL_SURFACE('',#27729,0.6767);
#720=CYLINDRICAL_SURFACE('',#27730,0.6767);
#721=CYLINDRICAL_SURFACE('',#27738,0.6767);
#722=CYLINDRICAL_SURFACE('',#27786,0.7911);
#723=CYLINDRICAL_SURFACE('',#27792,7.5);
#724=CYLINDRICAL_SURFACE('',#27795,2.01);
#725=CYLINDRICAL_SURFACE('',#27799,1.005);
#726=CYLINDRICAL_SURFACE('',#27805,0.805000000000009);
#727=CYLINDRICAL_SURFACE('',#27806,3.0025);
#728=CYLINDRICAL_SURFACE('',#28278,0.805);
#729=CYLINDRICAL_SURFACE('',#28280,1.755);
#730=CYLINDRICAL_SURFACE('',#28307,0.25);
#731=CYLINDRICAL_SURFACE('',#28312,0.25);
#732=CYLINDRICAL_SURFACE('',#28317,0.25);
#733=CYLINDRICAL_SURFACE('',#28322,0.25);
#734=CYLINDRICAL_SURFACE('',#28327,0.25);
#735=CYLINDRICAL_SURFACE('',#28332,0.25);
#736=CYLINDRICAL_SURFACE('',#28337,0.25);
#737=CYLINDRICAL_SURFACE('',#28342,0.25);
#738=CYLINDRICAL_SURFACE('',#28380,1.3);
#739=CYLINDRICAL_SURFACE('',#28385,1.205);
#740=CYLINDRICAL_SURFACE('',#28392,2.5);
#741=CYLINDRICAL_SURFACE('',#28401,0.3);
#742=CYLINDRICAL_SURFACE('',#28404,0.3);
#743=CYLINDRICAL_SURFACE('',#28414,6.255);
#744=CYLINDRICAL_SURFACE('',#28417,0.3);
#745=CYLINDRICAL_SURFACE('',#28424,0.3);
#746=CYLINDRICAL_SURFACE('',#28430,0.3);
#747=CYLINDRICAL_SURFACE('',#28437,0.3);
#748=CYLINDRICAL_SURFACE('',#28442,0.3);
#749=CYLINDRICAL_SURFACE('',#28445,0.3);
#750=CYLINDRICAL_SURFACE('',#28446,0.3);
#751=CYLINDRICAL_SURFACE('',#28448,0.3);
#752=CYLINDRICAL_SURFACE('',#28450,0.3);
#753=CYLINDRICAL_SURFACE('',#28456,0.3);
#754=CYLINDRICAL_SURFACE('',#28457,0.3);
#755=CYLINDRICAL_SURFACE('',#28459,0.3);
#756=CYLINDRICAL_SURFACE('',#28460,0.3);
#757=CYLINDRICAL_SURFACE('',#28480,1.1);
#758=CYLINDRICAL_SURFACE('',#28490,1.1);
#759=CYLINDRICAL_SURFACE('',#28499,1.1);
#760=CYLINDRICAL_SURFACE('',#28504,1.1);
#761=CYLINDRICAL_SURFACE('',#28514,0.3);
#762=CYLINDRICAL_SURFACE('',#28515,0.3);
#763=CYLINDRICAL_SURFACE('',#28522,0.3);
#764=CYLINDRICAL_SURFACE('',#28527,0.3);
#765=CYLINDRICAL_SURFACE('',#28529,0.3);
#766=CYLINDRICAL_SURFACE('',#28534,31.5);
#767=CYLINDRICAL_SURFACE('',#28544,33.);
#768=CYLINDRICAL_SURFACE('',#28550,0.3);
#769=CYLINDRICAL_SURFACE('',#28553,0.3);
#770=CYLINDRICAL_SURFACE('',#28562,31.5);
#771=CYLINDRICAL_SURFACE('',#28566,0.3);
#772=CYLINDRICAL_SURFACE('',#28578,0.804999999999993);
#773=CYLINDRICAL_SURFACE('',#28584,0.804999999999993);
#774=CYLINDRICAL_SURFACE('',#28590,0.804999999999993);
#775=CYLINDRICAL_SURFACE('',#28596,4.00009261333671);
#776=CYLINDRICAL_SURFACE('',#28599,0.804999999999993);
#777=CYLINDRICAL_SURFACE('',#28601,0.3);
#778=CYLINDRICAL_SURFACE('',#28612,2.);
#779=CYLINDRICAL_SURFACE('',#28618,30.6296013460341);
#780=CYLINDRICAL_SURFACE('',#28639,0.3);
#781=CYLINDRICAL_SURFACE('',#28651,0.3);
#782=CYLINDRICAL_SURFACE('',#28654,0.3);
#783=CYLINDRICAL_SURFACE('',#28669,0.3);
#784=CYLINDRICAL_SURFACE('',#28686,4.00009261333671);
#785=CYLINDRICAL_SURFACE('',#28691,12.);
#786=CYLINDRICAL_SURFACE('',#28705,4.00009261333671);
#787=CYLINDRICAL_SURFACE('',#28708,4.00009261333671);
#788=CYLINDRICAL_SURFACE('',#28710,4.00009261333671);
#789=CYLINDRICAL_SURFACE('',#28722,8.);
#790=CYLINDRICAL_SURFACE('',#28724,8.);
#791=CYLINDRICAL_SURFACE('',#28735,2.5);
#792=CYLINDRICAL_SURFACE('',#28740,7.99950242947665);
#793=CYLINDRICAL_SURFACE('',#28741,7.99950242947665);
#794=CYLINDRICAL_SURFACE('',#28746,12.);
#795=CYLINDRICAL_SURFACE('',#28754,4.00009261333671);
#796=CYLINDRICAL_SURFACE('',#28758,4.00009261333671);
#797=CYLINDRICAL_SURFACE('',#28760,5.00011576667089);
#798=CYLINDRICAL_SURFACE('',#28767,7.99950242947666);
#799=CYLINDRICAL_SURFACE('',#28769,7.99950242947666);
#800=CYLINDRICAL_SURFACE('',#28772,30.6296013460341);
#801=CYLINDRICAL_SURFACE('',#28802,2.25);
#802=CYLINDRICAL_SURFACE('',#28805,2.25);
#803=CYLINDRICAL_SURFACE('',#28806,2.25);
#804=CYLINDRICAL_SURFACE('',#28807,2.25);
#805=CYLINDRICAL_SURFACE('',#28811,4.);
#806=CYLINDRICAL_SURFACE('',#28830,10.);
#807=CYLINDRICAL_SURFACE('',#28836,10.);
#808=CYLINDRICAL_SURFACE('',#28851,5.);
#809=CYLINDRICAL_SURFACE('',#28853,2.5);
#810=CYLINDRICAL_SURFACE('',#28873,1.5);
#811=CYLINDRICAL_SURFACE('',#28876,1.5);
#812=CYLINDRICAL_SURFACE('',#28889,1.5);
#813=CYLINDRICAL_SURFACE('',#28890,1.5);
#814=CYLINDRICAL_SURFACE('',#28893,0.7911);
#815=CYLINDRICAL_SURFACE('',#28895,0.7911);
#816=CYLINDRICAL_SURFACE('',#28896,0.7911);
#817=CYLINDRICAL_SURFACE('',#28897,0.7911);
#818=CYLINDRICAL_SURFACE('',#28898,0.7911);
#819=CYLINDRICAL_SURFACE('',#28899,0.7911);
#820=CYLINDRICAL_SURFACE('',#28900,0.7911);
#821=CYLINDRICAL_SURFACE('',#28901,0.7911);
#822=CYLINDRICAL_SURFACE('',#28902,0.7911);
#823=CYLINDRICAL_SURFACE('',#28903,0.7911);
#824=CYLINDRICAL_SURFACE('',#28904,0.7911);
#825=CYLINDRICAL_SURFACE('',#28905,0.7911);
#826=CYLINDRICAL_SURFACE('',#28906,0.7911);
#827=CYLINDRICAL_SURFACE('',#28907,0.7911);
#828=CYLINDRICAL_SURFACE('',#28908,0.7911);
#829=CYLINDRICAL_SURFACE('',#28910,0.6767);
#830=CYLINDRICAL_SURFACE('',#28912,0.6767);
#831=CYLINDRICAL_SURFACE('',#28913,0.6767);
#832=CYLINDRICAL_SURFACE('',#28914,0.6767);
#833=CYLINDRICAL_SURFACE('',#28915,0.6767);
#834=CYLINDRICAL_SURFACE('',#28916,0.6767);
#835=CYLINDRICAL_SURFACE('',#28917,0.6767);
#836=CYLINDRICAL_SURFACE('',#28918,0.6767);
#837=CYLINDRICAL_SURFACE('',#28919,0.6767);
#838=CYLINDRICAL_SURFACE('',#28920,0.6767);
#839=CYLINDRICAL_SURFACE('',#28921,0.6767);
#840=CYLINDRICAL_SURFACE('',#28922,0.6767);
#841=CYLINDRICAL_SURFACE('',#28923,0.6767);
#842=CYLINDRICAL_SURFACE('',#28924,0.6767);
#843=CYLINDRICAL_SURFACE('',#28943,0.6767);
#844=CYLINDRICAL_SURFACE('',#28949,0.7911);
#845=FACE_BOUND('',#4061,.T.);
#846=FACE_BOUND('',#4065,.T.);
#847=FACE_BOUND('',#4071,.T.);
#848=FACE_BOUND('',#4075,.T.);
#849=FACE_BOUND('',#4223,.T.);
#850=FACE_BOUND('',#4238,.T.);
#851=FACE_BOUND('',#4287,.T.);
#852=FACE_BOUND('',#4302,.T.);
#853=FACE_BOUND('',#4303,.T.);
#854=FACE_BOUND('',#4304,.T.);
#855=FACE_BOUND('',#4305,.T.);
#856=FACE_BOUND('',#4306,.T.);
#857=FACE_BOUND('',#4307,.T.);
#858=FACE_BOUND('',#4310,.T.);
#859=FACE_BOUND('',#4320,.T.);
#860=FACE_BOUND('',#4324,.T.);
#861=FACE_BOUND('',#4381,.T.);
#862=FACE_BOUND('',#4417,.T.);
#863=FACE_BOUND('',#4418,.T.);
#864=FACE_BOUND('',#4519,.T.);
#865=FACE_BOUND('',#4523,.T.);
#866=FACE_BOUND('',#4526,.T.);
#867=FACE_BOUND('',#4614,.T.);
#868=FACE_BOUND('',#4617,.T.);
#869=FACE_BOUND('',#4618,.T.);
#870=FACE_BOUND('',#4619,.T.);
#871=FACE_BOUND('',#4621,.T.);
#872=FACE_BOUND('',#4626,.T.);
#873=FACE_BOUND('',#4632,.T.);
#874=FACE_BOUND('',#4639,.T.);
#875=FACE_BOUND('',#4734,.T.);
#876=FACE_BOUND('',#4990,.T.);
#877=FACE_BOUND('',#5104,.T.);
#878=FACE_BOUND('',#5169,.T.);
#879=FACE_BOUND('',#5173,.T.);
#880=FACE_BOUND('',#5176,.T.);
#881=FACE_BOUND('',#5177,.T.);
#882=FACE_BOUND('',#5178,.T.);
#883=FACE_BOUND('',#5179,.T.);
#884=FACE_BOUND('',#5180,.T.);
#885=FACE_BOUND('',#5181,.T.);
#886=FACE_BOUND('',#5182,.T.);
#887=FACE_BOUND('',#5214,.T.);
#888=FACE_BOUND('',#5215,.T.);
#889=FACE_BOUND('',#5216,.T.);
#890=FACE_BOUND('',#5217,.T.);
#891=FACE_BOUND('',#5219,.T.);
#892=FACE_BOUND('',#5225,.T.);
#893=FACE_BOUND('',#5230,.T.);
#894=FACE_BOUND('',#5252,.T.);
#895=FACE_BOUND('',#5263,.T.);
#896=FACE_BOUND('',#5264,.T.);
#897=FACE_BOUND('',#5265,.T.);
#898=FACE_BOUND('',#5276,.T.);
#899=FACE_BOUND('',#5277,.T.);
#900=FACE_BOUND('',#5278,.T.);
#901=FACE_BOUND('',#5279,.T.);
#902=FACE_BOUND('',#5290,.T.);
#903=FACE_BOUND('',#5291,.T.);
#904=FACE_BOUND('',#5292,.T.);
#905=FACE_BOUND('',#5293,.T.);
#906=FACE_BOUND('',#5294,.T.);
#907=FACE_BOUND('',#5295,.T.);
#908=FACE_BOUND('',#5318,.T.);
#909=FACE_BOUND('',#5319,.T.);
#910=FACE_BOUND('',#5320,.T.);
#911=FACE_BOUND('',#5321,.T.);
#912=FACE_BOUND('',#5322,.T.);
#913=FACE_BOUND('',#5330,.T.);
#914=FACE_BOUND('',#5418,.T.);
#915=FACE_BOUND('',#5425,.T.);
#916=FACE_BOUND('',#5428,.T.);
#917=FACE_BOUND('',#5446,.T.);
#918=FACE_BOUND('',#5449,.T.);
#919=FACE_BOUND('',#5561,.T.);
#920=FACE_BOUND('',#5562,.T.);
#921=FACE_BOUND('',#5602,.T.);
#922=FACE_BOUND('',#5603,.T.);
#923=FACE_BOUND('',#5615,.T.);
#924=FACE_BOUND('',#5625,.T.);
#925=FACE_BOUND('',#5626,.T.);
#926=FACE_BOUND('',#5627,.T.);
#927=B_SPLINE_CURVE_WITH_KNOTS('',3,(#35359,#35360,#35361,#35362,#35363,
#35364,#35365,#35366),.UNSPECIFIED.,.F.,.F.,(4,2,2,4),(0.,0.132844638508084,
0.516072227163779,0.952446027985499),.UNSPECIFIED.);
#928=B_SPLINE_CURVE_WITH_KNOTS('',3,(#35370,#35371,#35372,#35373,#35374,
#35375,#35376,#35377,#35378,#35379,#35380,#35381,#35382,#35383,#35384,#35385,
#35386,#35387,#35388,#35389,#35390,#35391,#35392,#35393,#35394,#35395,#35396,
#35397,#35398,#35399,#35400,#35401,#35402,#35403,#35404,#35405,#35406,#35407,
#35408,#35409,#35410,#35411,#35412,#35413,#35414,#35415),.UNSPECIFIED.,
 .F.,.F.,(4,3,3,3,3,3,3,3,3,3,3,3,3,3,3,4),(0.0570515547696962,0.149568289595802,
0.223514482269147,0.282749049350133,0.347422910484109,0.403643225845913,
0.449479112897856,0.49960329648389,0.536801063595721,0.570796167721486,
0.605256849208612,0.653238995251095,0.689225604782957,0.723986222716722,
0.763860497206074,0.797185433378544),.UNSPECIFIED.);
#929=B_SPLINE_CURVE_WITH_KNOTS('',3,(#35423,#35424,#35425,#35426,#35427,
#35428,#35429,#35430),.UNSPECIFIED.,.F.,.F.,(4,2,2,4),(0.,0.132844645404084,
0.506252028814034,0.808059701573943),.UNSPECIFIED.);
#930=B_SPLINE_CURVE_WITH_KNOTS('',3,(#35434,#35435,#35436,#35437,#35438,
#35439,#35440,#35441,#35442,#35443,#35444,#35445,#35446,#35447,#35448,#35449,
#35450,#35451,#35452,#35453,#35454,#35455,#35456,#35457,#35458,#35459,#35460,
#35461,#35462,#35463,#35464,#35465,#35466,#35467,#35468,#35469,#35470,#35471,
#35472,#35473,#35474,#35475,#35476,#35477,#35478,#35479),.UNSPECIFIED.,
 .F.,.F.,(4,3,3,3,3,3,3,3,3,3,3,3,3,3,3,4),(0.119257110722831,0.259765467187379,
0.372070105050779,0.462031684316788,0.560254105414672,0.645637837542741,
0.715250379918589,0.791375706431016,0.847869238432041,0.899498775585672,
0.951835401168699,1.02470754148633,1.07936164672455,1.1321537960343,1.19271223244992,
1.24332396243922),.UNSPECIFIED.);
#931=B_SPLINE_CURVE_WITH_KNOTS('',3,(#35487,#35488,#35489,#35490,#35491,
#35492,#35493,#35494),.UNSPECIFIED.,.F.,.F.,(4,2,2,4),(0.,0.132844651236982,
0.50625209941203,0.808059823281027),.UNSPECIFIED.);
#932=B_SPLINE_CURVE_WITH_KNOTS('',3,(#35498,#35499,#35500,#35501,#35502,
#35503,#35504,#35505),.UNSPECIFIED.,.F.,.F.,(4,2,2,4),(0.119257110624965,
0.656228060783636,0.967756326223977,1.24332397370374),.UNSPECIFIED.);
#933=B_SPLINE_CURVE_WITH_KNOTS('',3,(#35513,#35514,#35515,#35516,#35517,
#35518,#35519,#35520),.UNSPECIFIED.,.F.,.F.,(4,2,2,4),(0.,0.13284465519222,
0.506252154763523,0.80805991875116),.UNSPECIFIED.);
#934=B_SPLINE_CURVE_WITH_KNOTS('',3,(#35524,#35525,#35526,#35527,#35528,
#35529,#35530,#35531),.UNSPECIFIED.,.F.,.F.,(4,2,2,4),(0.119257110675847,
0.656228061682481,0.967756327568862,1.2433239759647),.UNSPECIFIED.);
#935=B_SPLINE_CURVE_WITH_KNOTS('',3,(#35539,#35540,#35541,#35542,#35543,
#35544,#35545,#35546),.UNSPECIFIED.,.F.,.F.,(4,2,2,4),(0.,0.132844659512976,
0.506252186151232,0.808059968862547),.UNSPECIFIED.);
#936=B_SPLINE_CURVE_WITH_KNOTS('',3,(#35550,#35551,#35552,#35553,#35554,
#35555,#35556,#35557,#35558,#35559,#35560,#35561,#35562,#35563,#35564,#35565,
#35566,#35567,#35568,#35569,#35570,#35571,#35572,#35573,#35574,#35575,#35576,
#35577,#35578,#35579,#35580,#35581,#35582,#35583,#35584,#35585,#35586,#35587,
#35588,#35589,#35590,#35591,#35592,#35593,#35594,#35595),.UNSPECIFIED.,
 .F.,.F.,(4,3,3,3,3,3,3,3,3,3,3,3,3,3,3,4),(0.119257110749042,0.259765469653336,
0.372070124544791,0.462031702597275,0.560254122921395,0.645637855304144,
0.715250398053293,0.791375721829739,0.847869254348945,0.899498792238198,
0.951835419100633,1.02470755982132,1.07936166536184,1.13215381569044,1.19271225399545,
1.24332398198339),.UNSPECIFIED.);
#937=B_SPLINE_CURVE_WITH_KNOTS('',3,(#35603,#35604,#35605,#35606,#35607,
#35608,#35609,#35610),.UNSPECIFIED.,.F.,.F.,(4,2,2,4),(0.,0.132844660225076,
0.50625220794817,0.808060006746839),.UNSPECIFIED.);
#938=B_SPLINE_CURVE_WITH_KNOTS('',3,(#35614,#35615,#35616,#35617,#35618,
#35619,#35620,#35621,#35622,#35623,#35624,#35625,#35626,#35627,#35628,#35629,
#35630,#35631,#35632,#35633,#35634,#35635,#35636,#35637,#35638,#35639,#35640,
#35641,#35642,#35643,#35644,#35645,#35646,#35647,#35648,#35649,#35650,#35651,
#35652,#35653,#35654,#35655,#35656,#35657,#35658,#35659),.UNSPECIFIED.,
 .F.,.F.,(4,3,3,3,3,3,3,3,3,3,3,3,3,3,3,4),(0.119257110935751,0.259765470643982,
0.372070120535554,0.462031699629386,0.560254116907991,0.645637850869692,
0.715250394186009,0.791375722521945,0.847869255781902,0.899498793924427,
0.951835420553605,1.0247075625656,1.0793616690746,1.1321538192465,1.19271225740627,
1.2433239886016),.UNSPECIFIED.);
#939=B_SPLINE_CURVE_WITH_KNOTS('',3,(#35667,#35668,#35669,#35670,#35671,
#35672,#35673,#35674),.UNSPECIFIED.,.F.,.F.,(4,2,2,4),(0.,0.132844662938583,
0.506252246824074,0.808060074600784),.UNSPECIFIED.);
#940=B_SPLINE_CURVE_WITH_KNOTS('',3,(#35678,#35679,#35680,#35681,#35682,
#35683,#35684,#35685,#35686,#35687,#35688,#35689,#35690,#35691,#35692,#35693,
#35694,#35695,#35696,#35697,#35698,#35699,#35700,#35701,#35702,#35703,#35704,
#35705,#35706,#35707,#35708,#35709,#35710,#35711,#35712,#35713,#35714,#35715,
#35716,#35717,#35718,#35719,#35720,#35721,#35722,#35723),.UNSPECIFIED.,
 .F.,.F.,(4,3,3,3,3,3,3,3,3,3,3,3,3,3,3,4),(0.119257111119166,0.259765471826694,
0.37207011961253,0.462031700004267,0.560254117679798,0.645637852567247,
0.715250396938671,0.791375727041412,0.847869260758659,0.899498799503518,
0.951835426609056,1.02470756915164,1.07936167605858,1.13215382706252,1.19271226527703,
1.24332399677939),.UNSPECIFIED.);
#941=B_SPLINE_CURVE_WITH_KNOTS('',3,(#35731,#35732,#35733,#35734,#35735,
#35736,#35737,#35738),.UNSPECIFIED.,.F.,.F.,(4,2,2,4),(0.,0.132844662332266,
0.506252246901422,0.808060074727922),.UNSPECIFIED.);
#942=B_SPLINE_CURVE_WITH_KNOTS('',3,(#35742,#35743,#35744,#35745,#35746,
#35747,#35748,#35749,#35750,#35751,#35752,#35753,#35754,#35755,#35756,#35757,
#35758,#35759,#35760,#35761,#35762,#35763,#35764,#35765,#35766,#35767,#35768,
#35769,#35770,#35771,#35772,#35773,#35774,#35775,#35776,#35777,#35778,#35779,
#35780,#35781,#35782,#35783,#35784,#35785,#35786,#35787),.UNSPECIFIED.,
 .F.,.F.,(4,3,3,3,3,3,3,3,3,3,3,3,3,3,3,4),(0.119257111366122,0.259765473891839,
0.372070110740388,0.462031694612758,0.560254112754749,0.645637850106888,
0.715250395993883,0.791375732012897,0.847869266957768,0.899498806411333,
0.951835433730862,1.02470757819111,1.0793616865363,1.13215383802383,1.19271227633857,
1.24332401157186),.UNSPECIFIED.);
#943=B_SPLINE_CURVE_WITH_KNOTS('',3,(#35795,#35796,#35797,#35798,#35799,
#35800,#35801,#35802),.UNSPECIFIED.,.F.,.F.,(4,2,2,4),(0.,0.132844673397704,
0.506252379761466,0.808060307624835),.UNSPECIFIED.);
#944=B_SPLINE_CURVE_WITH_KNOTS('',3,(#35806,#35807,#35808,#35809,#35810,
#35811,#35812,#35813,#35814,#35815,#35816,#35817,#35818,#35819,#35820,#35821,
#35822,#35823,#35824,#35825,#35826,#35827,#35828,#35829,#35830,#35831,#35832,
#35833,#35834,#35835,#35836,#35837,#35838,#35839,#35840,#35841,#35842,#35843,
#35844,#35845,#35846,#35847,#35848,#35849,#35850,#35851),.UNSPECIFIED.,
 .F.,.F.,(4,3,3,3,3,3,3,3,3,3,3,3,3,3,3,4),(0.119257111629581,0.25976547574254,
0.372070105266965,0.462031691347436,0.560254108875743,0.645637848332932,
0.715250395621009,0.791375736838517,0.847869272800359,0.899498812911096,
0.951835440390312,1.02470758642605,1.07936169595285,1.13215384794752,1.19271228630097,
1.24332402453326),.UNSPECIFIED.);
#945=B_SPLINE_CURVE_WITH_KNOTS('',3,(#35859,#35860,#35861,#35862,#35863,
#35864,#35865,#35866),.UNSPECIFIED.,.F.,.F.,(4,2,2,4),(0.,0.13284466924466,
0.516072631745704,0.952446861020481),.UNSPECIFIED.);
#946=B_SPLINE_CURVE_WITH_KNOTS('',3,(#35870,#35871,#35872,#35873,#35874,
#35875),.UNSPECIFIED.,.F.,.F.,(4,2,4),(0.0570515528938123,0.427835960222195,
0.797185331883135),.UNSPECIFIED.);
#947=B_SPLINE_CURVE_WITH_KNOTS('',3,(#35883,#35884,#35885,#35886,#35887,
#35888,#35889,#35890),.UNSPECIFIED.,.F.,.F.,(4,2,2,4),(0.,0.132844667776373,
0.50625232484217,0.80806021526576),.UNSPECIFIED.);
#948=B_SPLINE_CURVE_WITH_KNOTS('',3,(#35894,#35895,#35896,#35897,#35898,
#35899,#35900,#35901),.UNSPECIFIED.,.F.,.F.,(4,2,2,4),(0.11925711175789,
0.65622808055564,0.96775635514001,1.2433240286364),.UNSPECIFIED.);
#949=B_SPLINE_CURVE_WITH_KNOTS('',3,(#35909,#35910,#35911,#35912,#35913,
#35914,#35915,#35916),.UNSPECIFIED.,.F.,.F.,(4,2,2,4),(0.,0.132844663472207,
0.506252284758126,0.808060148341119),.UNSPECIFIED.);
#950=B_SPLINE_CURVE_WITH_KNOTS('',3,(#35920,#35921,#35922,#35923,#35924,
#35925,#35926,#35927,#35928,#35929,#35930,#35931,#35932,#35933,#35934,#35935,
#35936,#35937,#35938,#35939,#35940,#35941,#35942,#35943,#35944,#35945,#35946,
#35947,#35948,#35949,#35950,#35951,#35952,#35953,#35954,#35955,#35956,#35957,
#35958,#35959,#35960,#35961,#35962,#35963,#35964,#35965),.UNSPECIFIED.,
 .F.,.F.,(4,3,3,3,3,3,3,3,3,3,3,3,3,3,3,4),(0.119257111880342,0.259765477112128,
0.372070088145812,0.462031678747241,0.560254098178944,0.645637840123405,
0.715250389444509,0.791375737515883,0.847869274543226,0.899498815448392,
0.951835443060419,1.02470759072897,1.07936170148039,1.13215385418117,1.19271229155254,
1.24332403373463),.UNSPECIFIED.);
#951=B_SPLINE_CURVE_WITH_KNOTS('',3,(#35973,#35974,#35975,#35976,#35977,
#35978,#35979,#35980),.UNSPECIFIED.,.F.,.F.,(4,2,2,4),(0.,0.132844658495434,
0.506252224582906,0.808060045014047),.UNSPECIFIED.);
#952=B_SPLINE_CURVE_WITH_KNOTS('',3,(#35984,#35985,#35986,#35987,#35988,
#35989,#35990,#35991,#35992,#35993,#35994,#35995,#35996,#35997,#35998,#35999,
#36000,#36001,#36002,#36003,#36004,#36005,#36006,#36007,#36008,#36009,#36010,
#36011,#36012,#36013,#36014,#36015,#36016,#36017,#36018,#36019,#36020,#36021,
#36022,#36023,#36024,#36025,#36026,#36027,#36028,#36029),.UNSPECIFIED.,
 .F.,.F.,(4,3,3,3,3,3,3,3,3,3,3,3,3,3,3,4),(0.119257111768233,0.259765476607262,
0.372070087318006,0.462031678446782,0.56025410111,0.645637842281308,0.715250391588022,
0.79137573761201,0.847869274220567,0.899498815109955,0.951835442916956,
1.02470758980783,1.07936169997599,1.13215385283319,1.19271229000116,1.24332403048047),
 .UNSPECIFIED.);
#953=B_SPLINE_CURVE_WITH_KNOTS('',3,(#36037,#36038,#36039,#36040,#36041,
#36042,#36043,#36044),.UNSPECIFIED.,.F.,.F.,(4,2,2,4),(0.,0.13284465245657,
0.506252146299661,0.808059910467814),.UNSPECIFIED.);
#954=B_SPLINE_CURVE_WITH_KNOTS('',3,(#36048,#36049,#36050,#36051,#36052,
#36053,#36054,#36055,#36056,#36057,#36058,#36059,#36060,#36061,#36062,#36063,
#36064,#36065,#36066,#36067,#36068,#36069,#36070,#36071,#36072,#36073,#36074,
#36075,#36076,#36077,#36078,#36079,#36080,#36081,#36082,#36083,#36084,#36085,
#36086,#36087,#36088,#36089,#36090,#36091,#36092,#36093),.UNSPECIFIED.,
 .F.,.F.,(4,3,3,3,3,3,3,3,3,3,3,3,3,3,3,4),(0.119257111589422,0.259765475268004,
0.372070087430169,0.462031677585357,0.560254102164649,0.645637842021328,
0.715250390618003,0.791375733532979,0.847869269468616,0.899498810014054,
0.951835437747858,1.02470758356541,1.07936169292858,1.13215384569843,1.19271228256891,
1.24332402101808),.UNSPECIFIED.);
#955=B_SPLINE_CURVE_WITH_KNOTS('',3,(#36101,#36102,#36103,#36104,#36105,
#36106,#36107,#36108),.UNSPECIFIED.,.F.,.F.,(4,2,2,4),(0.,0.132844642748753,
0.506252042985508,0.808059732577867),.UNSPECIFIED.);
#956=B_SPLINE_CURVE_WITH_KNOTS('',3,(#36112,#36113,#36114,#36115,#36116,
#36117,#36118,#36119,#36120,#36121,#36122,#36123,#36124,#36125,#36126,#36127,
#36128,#36129,#36130,#36131,#36132,#36133,#36134,#36135,#36136,#36137,#36138,
#36139,#36140,#36141,#36142,#36143,#36144,#36145,#36146,#36147,#36148,#36149,
#36150,#36151,#36152,#36153,#36154,#36155,#36156,#36157),.UNSPECIFIED.,
 .F.,.F.,(4,3,3,3,3,3,3,3,3,3,3,3,3,3,3,4),(0.11925711158155,0.259765474036443,
0.37207007811818,0.462031669168862,0.560254093454163,0.64563783317498,0.715250381276493,
0.791375725677586,0.847869261370474,0.899498801276523,0.951835428081933,
1.02470757386662,1.07936168320514,1.132153835061,1.19271227143741,1.2433240112207),
 .UNSPECIFIED.);
#957=B_SPLINE_CURVE_WITH_KNOTS('',3,(#36165,#36166,#36167,#36168,#36169,
#36170,#36171,#36172),.UNSPECIFIED.,.F.,.F.,(4,2,2,4),(0.,0.132844640346774,
0.506251998634185,0.808059655501969),.UNSPECIFIED.);
#958=B_SPLINE_CURVE_WITH_KNOTS('',3,(#36176,#36177,#36178,#36179,#36180,
#36181,#36182,#36183,#36184,#36185,#36186,#36187,#36188,#36189,#36190,#36191,
#36192,#36193,#36194,#36195,#36196,#36197,#36198,#36199,#36200,#36201,#36202,
#36203,#36204,#36205,#36206,#36207,#36208,#36209,#36210,#36211,#36212,#36213,
#36214,#36215,#36216,#36217,#36218,#36219,#36220,#36221),.UNSPECIFIED.,
 .F.,.F.,(4,3,3,3,3,3,3,3,3,3,3,3,3,3,3,4),(0.119257111275641,0.259765471844383,
0.372070088547094,0.462031674851804,0.56025409860193,0.645637835754886,
0.715250382069428,0.791375720258739,0.847869254704594,0.899498793847599,
0.951835420477167,1.02470756431427,1.0793616721921,1.13215382332698,1.19271225959965,
1.24332399582558),.UNSPECIFIED.);
#959=B_SPLINE_CURVE_WITH_KNOTS('',3,(#36229,#36230,#36231,#36232,#36233,
#36234,#36235,#36236),.UNSPECIFIED.,.F.,.F.,(4,2,2,4),(0.,0.132844649562065,
0.506252093176766,0.808059817747012),.UNSPECIFIED.);
#960=B_SPLINE_CURVE_WITH_KNOTS('',3,(#36240,#36241,#36242,#36243,#36244,
#36245,#36246,#36247,#36248,#36249,#36250,#36251,#36252,#36253,#36254,#36255,
#36256,#36257,#36258,#36259,#36260,#36261,#36262,#36263,#36264,#36265,#36266,
#36267,#36268,#36269,#36270,#36271,#36272,#36273,#36274,#36275,#36276,#36277,
#36278,#36279,#36280,#36281,#36282,#36283,#36284,#36285),.UNSPECIFIED.,
 .F.,.F.,(4,3,3,3,3,3,3,3,3,3,3,3,3,3,3,4),(0.11925711110465,0.259765470177295,
0.372070093314613,0.462031677669758,0.560254099913928,0.645637835385414,
0.715250380522247,0.791375714853033,0.847869248457131,0.899498786975331,
0.951835413282065,1.024707555883,1.07936166283371,1.13215381358851,1.19271224958777,
1.24332398368582),.UNSPECIFIED.);
#961=B_SPLINE_CURVE_WITH_KNOTS('',3,(#36293,#36294,#36295,#36296,#36297,
#36298,#36299,#36300),.UNSPECIFIED.,.F.,.F.,(4,2,2,4),(0.,0.132844633425521,
0.506251897062758,0.808059476130729),.UNSPECIFIED.);
#962=B_SPLINE_CURVE_WITH_KNOTS('',3,(#36304,#36305,#36306,#36307,#36308,
#36309,#36310,#36311,#36312,#36313,#36314,#36315,#36316,#36317,#36318,#36319,
#36320,#36321,#36322,#36323,#36324,#36325,#36326,#36327,#36328,#36329,#36330,
#36331,#36332,#36333,#36334,#36335,#36336,#36337,#36338,#36339,#36340,#36341,
#36342,#36343,#36344,#36345,#36346,#36347,#36348,#36349),.UNSPECIFIED.,
 .F.,.F.,(4,3,3,3,3,3,3,3,3,3,3,3,3,3,3,4),(0.119257110965343,0.259765469256534,
0.372070096273217,0.462031679137717,0.560254101459727,0.64563783593912,
0.715250380224683,0.791375712237953,0.847869245370068,0.89949878344051,
0.951835409469422,1.02470755142578,1.07936165789306,1.13215380812679,1.19271224425172,
1.24332397729487),.UNSPECIFIED.);
#963=B_SPLINE_CURVE_WITH_KNOTS('',3,(#36370,#36371,#36372,#36373,#36374,
#36375,#36376,#36377,#36378,#36379,#36380,#36381,#36382,#36383,#36384,#36385,
#36386,#36387,#36388,#36389,#36390,#36391,#36392,#36393,#36394,#36395,#36396,
#36397,#36398,#36399,#36400,#36401,#36402,#36403,#36404,#36405,#36406,#36407,
#36408,#36409,#36410,#36411,#36412,#36413,#36414,#36415),.UNSPECIFIED.,
 .F.,.F.,(4,3,3,3,3,3,3,3,3,3,3,3,3,3,3,4),(0.0570515530865148,0.149568276755442,
0.223514452534054,0.28274901337513,0.34742285854684,0.403643169033227,0.449479051155942,
0.49960323633162,0.536800999594909,0.570796099675367,0.605256776272716,
0.65323891781402,0.689225523969997,0.723986137492795,0.763860406328189,
0.79718534243793),.UNSPECIFIED.);
#964=B_SPLINE_CURVE_WITH_KNOTS('',3,(#36423,#36424,#36425,#36426,#36427,
#36428,#36429,#36430),.UNSPECIFIED.,.F.,.F.,(4,2,2,4),(0.,0.132844666637408,
0.506252309287785,0.808060187337575),.UNSPECIFIED.);
#965=B_SPLINE_CURVE_WITH_KNOTS('',3,(#36434,#36435,#36436,#36437,#36438,
#36439,#36440,#36441,#36442,#36443,#36444,#36445,#36446,#36447,#36448,#36449,
#36450,#36451,#36452,#36453,#36454,#36455,#36456,#36457,#36458,#36459,#36460,
#36461,#36462,#36463,#36464,#36465,#36466,#36467,#36468,#36469,#36470,#36471,
#36472,#36473,#36474,#36475,#36476,#36477,#36478,#36479),.UNSPECIFIED.,
 .F.,.F.,(4,3,3,3,3,3,3,3,3,3,3,3,3,3,3,4),(0.119257111738278,0.259765477798221,
0.372070100839862,0.462031689948238,0.560254109920137,0.645637851207348,
0.715250400204313,0.791375744757855,0.847869281690351,0.899498822750789,
0.951835450996311,1.02470759830169,1.07936170878072,1.13215386181501,1.1927123002489,
1.24332404021782),.UNSPECIFIED.);
#966=B_SPLINE_CURVE_WITH_KNOTS('',3,(#36487,#36488,#36489,#36490,#36491,
#36492,#36493,#36494),.UNSPECIFIED.,.F.,.F.,(4,2,2,4),(0.,0.132844665315855,
0.50625230445513,0.808060181601913),.UNSPECIFIED.);
#967=B_SPLINE_CURVE_WITH_KNOTS('',3,(#36498,#36499,#36500,#36501,#36502,
#36503,#36504,#36505,#36506,#36507,#36508,#36509,#36510,#36511,#36512,#36513,
#36514,#36515,#36516,#36517,#36518,#36519,#36520,#36521,#36522,#36523,#36524,
#36525,#36526,#36527,#36528,#36529,#36530,#36531,#36532,#36533,#36534,#36535,
#36536,#36537,#36538,#36539,#36540,#36541,#36542,#36543),.UNSPECIFIED.,
 .F.,.F.,(4,3,3,3,3,3,3,3,3,3,3,3,3,3,3,4),(0.119257111812372,0.259765475731827,
0.372070092505628,0.462031681270809,0.560254101069256,0.645637841331601,
0.71525038929406,0.791375733485408,0.847869269695733,0.899498809903491,
0.951835437077337,1.02470758360001,1.07936169349201,1.13215384552011,1.19271228284677,
1.24332402316801),.UNSPECIFIED.);
#968=B_SPLINE_CURVE_WITH_KNOTS('',3,(#36551,#36552,#36553,#36554,#36555,
#36556,#36557,#36558),.UNSPECIFIED.,.F.,.F.,(4,2,2,4),(0.,0.132844658784055,
0.506252224782715,0.808060043839757),.UNSPECIFIED.);
#969=B_SPLINE_CURVE_WITH_KNOTS('',3,(#36562,#36563,#36564,#36565,#36566,
#36567,#36568,#36569,#36570,#36571,#36572,#36573,#36574,#36575,#36576,#36577,
#36578,#36579,#36580,#36581,#36582,#36583,#36584,#36585,#36586,#36587,#36588,
#36589,#36590,#36591,#36592,#36593,#36594,#36595,#36596,#36597,#36598,#36599,
#36600,#36601,#36602,#36603,#36604,#36605,#36606,#36607),.UNSPECIFIED.,
 .F.,.F.,(4,3,3,3,3,3,3,3,3,3,3,3,3,3,3,4),(0.119257111835025,0.259765477191931,
0.372070087807762,0.46203167897918,0.560254100528681,0.64563784229888,0.715250391776462,
0.79137573900606,0.847869275966586,0.899498816981767,0.951835444817433,
1.02470759228564,1.0793617028868,1.13215385580022,1.19271229305914,1.24332403469027),
 .UNSPECIFIED.);
#970=B_SPLINE_CURVE_WITH_KNOTS('',3,(#36615,#36616,#36617,#36618,#36619,
#36620,#36621,#36622),.UNSPECIFIED.,.F.,.F.,(4,2,2,4),(0.,0.132844654191751,
0.506252166964219,0.808059945349378),.UNSPECIFIED.);
#971=B_SPLINE_CURVE_WITH_KNOTS('',3,(#36626,#36627,#36628,#36629,#36630,
#36631,#36632,#36633),.UNSPECIFIED.,.F.,.F.,(4,2,2,4),(0.119257111680258,
0.656228079177594,0.967756353404116,1.24332402668173),.UNSPECIFIED.);
#972=B_SPLINE_CURVE_WITH_KNOTS('',3,(#36641,#36642,#36643,#36644,#36645,
#36646,#36647,#36648),.UNSPECIFIED.,.F.,.F.,(4,2,2,4),(0.,0.132844645447949,
0.506252076671479,0.808059790455401),.UNSPECIFIED.);
#973=B_SPLINE_CURVE_WITH_KNOTS('',3,(#36652,#36653,#36654,#36655,#36656,
#36657,#36658,#36659,#36660,#36661,#36662,#36663,#36664,#36665,#36666,#36667,
#36668,#36669,#36670,#36671,#36672,#36673,#36674,#36675,#36676,#36677,#36678,
#36679,#36680,#36681,#36682,#36683,#36684,#36685,#36686,#36687,#36688,#36689,
#36690,#36691,#36692,#36693,#36694,#36695,#36696,#36697),.UNSPECIFIED.,
 .F.,.F.,(4,3,3,3,3,3,3,3,3,3,3,3,3,3,3,4),(0.119257111683661,0.259765474766316,
0.372070077979508,0.46203166925924,0.560254093713209,0.64563783404217,0.715250382509683,
0.791375727925691,0.847869263978092,0.899498804160855,0.951835431203088,
1.02470757748854,1.07936168720263,1.13215383920229,1.1927122757105,1.2433240163449),
 .UNSPECIFIED.);
#974=B_SPLINE_CURVE_WITH_KNOTS('',3,(#36705,#36706,#36707,#36708,#36709,
#36710,#36711,#36712),.UNSPECIFIED.,.F.,.F.,(4,2,2,4),(0.,0.132844642681371,
0.506252033924115,0.808059717106107),.UNSPECIFIED.);
#975=B_SPLINE_CURVE_WITH_KNOTS('',3,(#36716,#36717,#36718,#36719,#36720,
#36721,#36722,#36723,#36724,#36725,#36726,#36727,#36728,#36729,#36730,#36731,
#36732,#36733,#36734,#36735,#36736,#36737,#36738,#36739,#36740,#36741,#36742,
#36743,#36744,#36745,#36746,#36747,#36748,#36749,#36750,#36751,#36752,#36753,
#36754,#36755,#36756,#36757,#36758,#36759,#36760,#36761),.UNSPECIFIED.,
 .F.,.F.,(4,3,3,3,3,3,3,3,3,3,3,3,3,3,3,4),(0.119257111394877,0.259765472481849,
0.372070087964051,0.462031675530459,0.560254099488109,0.645637837063428,
0.715250383674388,0.791375722358766,0.847869257075252,0.899498796470126,
0.951835423266047,1.0247075674722,1.07936167562681,1.13215382714539,1.19271226332587,
1.24332400009066),.UNSPECIFIED.);
#976=B_SPLINE_CURVE_WITH_KNOTS('',3,(#36769,#36770,#36771,#36772,#36773,
#36774,#36775,#36776),.UNSPECIFIED.,.F.,.F.,(4,2,2,4),(0.,0.132844642259177,
0.506252014111271,0.808059681312646),.UNSPECIFIED.);
#977=B_SPLINE_CURVE_WITH_KNOTS('',3,(#36780,#36781,#36782,#36783,#36784,
#36785,#36786,#36787,#36788,#36789,#36790,#36791,#36792,#36793,#36794,#36795,
#36796,#36797,#36798,#36799,#36800,#36801,#36802,#36803,#36804,#36805,#36806,
#36807,#36808,#36809,#36810,#36811,#36812,#36813,#36814,#36815,#36816,#36817,
#36818,#36819,#36820,#36821,#36822,#36823,#36824,#36825),.UNSPECIFIED.,
 .F.,.F.,(4,3,3,3,3,3,3,3,3,3,3,3,3,3,3,4),(0.119257111232989,0.259765470932784,
0.372070089852755,0.462031675399422,0.560254097898976,0.645637834265523,
0.715250380101727,0.791375716804756,0.847869250808081,0.899498789609946,
0.951835416007403,1.02470755921339,1.07936166661788,1.1321538176216,1.19271225354742,
1.24332398883135),.UNSPECIFIED.);
#978=B_SPLINE_CURVE_WITH_KNOTS('',3,(#36833,#36834,#36835,#36836,#36837,
#36838,#36839,#36840),.UNSPECIFIED.,.F.,.F.,(4,2,2,4),(0.,0.132844644201326,
0.506252033181429,0.808059713879001),.UNSPECIFIED.);
#979=B_SPLINE_CURVE_WITH_KNOTS('',3,(#36844,#36845,#36846,#36847,#36848,
#36849,#36850,#36851,#36852,#36853,#36854,#36855,#36856,#36857,#36858,#36859,
#36860,#36861,#36862,#36863,#36864,#36865,#36866,#36867,#36868,#36869,#36870,
#36871,#36872,#36873,#36874,#36875,#36876,#36877,#36878,#36879,#36880,#36881,
#36882,#36883,#36884,#36885,#36886,#36887,#36888,#36889),.UNSPECIFIED.,
 .F.,.F.,(4,3,3,3,3,3,3,3,3,3,3,3,3,3,3,4),(0.119257111061743,0.259765469697972,
0.372070088944832,0.46203167354931,0.56025409772518,0.645637833028479,0.715250378035739,
0.791375712286345,0.847869245769498,0.899498784092187,0.951835410097075,
1.0247075526107,1.07936165949592,1.13215380990758,1.19271224573097,1.24332398015157),
 .UNSPECIFIED.);
#980=B_SPLINE_CURVE_WITH_KNOTS('',3,(#36897,#36898,#36899,#36900,#36901,
#36902,#36903,#36904),.UNSPECIFIED.,.F.,.F.,(4,2,2,4),(0.,0.132844636748929,
0.516072211405751,0.952445994998063),.UNSPECIFIED.);
#981=B_SPLINE_CURVE_WITH_KNOTS('',3,(#36908,#36909,#36910,#36911,#36912,
#36913,#36914,#36915,#36916,#36917,#36918,#36919,#36920,#36921,#36922,#36923,
#36924,#36925,#36926,#36927,#36928,#36929,#36930,#36931,#36932,#36933,#36934,
#36935,#36936,#36937,#36938,#36939,#36940,#36941,#36942,#36943,#36944,#36945,
#36946,#36947,#36948,#36949,#36950,#36951,#36952,#36953),.UNSPECIFIED.,
 .F.,.F.,(4,3,3,3,3,3,3,3,3,3,3,3,3,3,3,4),(0.0570515546134941,0.149568288423378,
0.223514476692031,0.282749043798704,0.347422904353558,0.403643219445934,
0.449479106333475,0.499603290613782,0.53680105742363,0.570796161259589,
0.605256842334552,0.653238988024055,0.689225597291183,0.723986214927346,
0.763860488675733,0.797185425092567),.UNSPECIFIED.);
#982=B_SPLINE_CURVE_WITH_KNOTS('',3,(#36961,#36962,#36963,#36964,#36965,
#36966,#36967,#36968),.UNSPECIFIED.,.F.,.F.,(4,2,2,4),(0.,0.132844644704538,
0.506252021113135,0.808059690353989),.UNSPECIFIED.);
#983=B_SPLINE_CURVE_WITH_KNOTS('',3,(#36972,#36973,#36974,#36975,#36976,
#36977,#36978,#36979),.UNSPECIFIED.,.F.,.F.,(4,2,2,4),(0.119257110771861,
0.65622806320778,0.967756328874099,1.24332396436209),.UNSPECIFIED.);
#984=B_SPLINE_CURVE_WITH_KNOTS('',3,(#36987,#36988,#36989,#36990,#36991,
#36992,#36993,#36994),.UNSPECIFIED.,.F.,.F.,(4,2,2,4),(0.,0.132844648302869,
0.506252066960849,0.808059767961743),.UNSPECIFIED.);
#985=B_SPLINE_CURVE_WITH_KNOTS('',3,(#36998,#36999,#37000,#37001,#37002,
#37003,#37004,#37005,#37006,#37007,#37008,#37009,#37010,#37011,#37012,#37013,
#37014,#37015,#37016,#37017,#37018,#37019,#37020,#37021,#37022,#37023,#37024,
#37025,#37026,#37027,#37028,#37029,#37030,#37031,#37032,#37033,#37034,#37035,
#37036,#37037,#37038,#37039,#37040,#37041,#37042,#37043),.UNSPECIFIED.,
 .F.,.F.,(4,3,3,3,3,3,3,3,3,3,3,3,3,3,3,4),(0.119257110621164,0.259765468263962,
0.372070112199727,0.462031691450782,0.560254114472962,0.645637846634284,
0.715250389295661,0.791375714007369,0.847869246226891,0.899498783860491,
0.951835410214567,1.02470755060181,1.07936165589224,1.13215380591584,1.19271224305412,
1.24332397176354),.UNSPECIFIED.);
#986=B_SPLINE_CURVE_WITH_KNOTS('',3,(#37051,#37052,#37053,#37054,#37055,
#37056,#37057,#37058),.UNSPECIFIED.,.F.,.F.,(4,2,2,4),(0.,0.132844653773461,
0.506252139652089,0.808059893305447),.UNSPECIFIED.);
#987=B_SPLINE_CURVE_WITH_KNOTS('',3,(#37062,#37063,#37064,#37065,#37066,
#37067,#37068,#37069,#37070,#37071,#37072,#37073,#37074,#37075,#37076,#37077,
#37078,#37079,#37080,#37081,#37082,#37083,#37084,#37085,#37086,#37087,#37088,
#37089,#37090,#37091,#37092,#37093,#37094,#37095,#37096,#37097,#37098,#37099,
#37100,#37101,#37102,#37103,#37104,#37105,#37106,#37107),.UNSPECIFIED.,
 .F.,.F.,(4,3,3,3,3,3,3,3,3,3,3,3,3,3,3,4),(0.119257110641572,0.259765468385939,
0.372070117379027,0.462031695480993,0.560254117172397,0.64563784910041,
0.715250391578671,0.791375715315744,0.847869247475839,0.899498785035086,
0.951835411419915,1.02470755171406,1.07936165693467,1.13215380684117,1.19271224435265,
1.24332397259651),.UNSPECIFIED.);
#988=B_SPLINE_CURVE_WITH_KNOTS('',3,(#37115,#37116,#37117,#37118,#37119,
#37120,#37121,#37122),.UNSPECIFIED.,.F.,.F.,(4,2,2,4),(0.,0.13284465680416,
0.506252153781493,0.80805991374936),.UNSPECIFIED.);
#989=B_SPLINE_CURVE_WITH_KNOTS('',3,(#37126,#37127,#37128,#37129,#37130,
#37131,#37132,#37133,#37134,#37135,#37136,#37137,#37138,#37139,#37140,#37141,
#37142,#37143,#37144,#37145,#37146,#37147,#37148,#37149,#37150,#37151,#37152,
#37153,#37154,#37155,#37156,#37157,#37158,#37159,#37160,#37161,#37162,#37163,
#37164,#37165,#37166,#37167,#37168,#37169,#37170,#37171),.UNSPECIFIED.,
 .F.,.F.,(4,3,3,3,3,3,3,3,3,3,3,3,3,3,3,4),(0.119257110659739,0.259765468839433,
0.372070119778476,0.462031697519513,0.560254116817873,0.645637849227801,
0.715250391720227,0.79137571663617,0.84786924906881,0.899498786754164,0.951835413160386,
1.02470755389461,1.07936165944528,1.13215380946011,1.19271224707953,1.24332397609729),
 .UNSPECIFIED.);
#990=B_SPLINE_CURVE_WITH_KNOTS('',3,(#37179,#37180,#37181,#37182,#37183,
#37184,#37185,#37186),.UNSPECIFIED.,.F.,.F.,(4,2,2,4),(0.,0.13284465770136,
0.506252176893417,0.808059953558626),.UNSPECIFIED.);
#991=B_SPLINE_CURVE_WITH_KNOTS('',3,(#37190,#37191,#37192,#37193,#37194,
#37195,#37196,#37197),.UNSPECIFIED.,.F.,.F.,(4,2,2,4),(0.119257110811679,
0.656228064026157,0.967756330899547,1.24332398190981),.UNSPECIFIED.);
#992=B_SPLINE_CURVE_WITH_KNOTS('',3,(#37205,#37206,#37207,#37208,#37209,
#37210,#37211,#37212),.UNSPECIFIED.,.F.,.F.,(4,2,2,4),(0.,0.132844660625905,
0.506252215494008,0.808060020062334),.UNSPECIFIED.);
#993=B_SPLINE_CURVE_WITH_KNOTS('',3,(#37216,#37217,#37218,#37219,#37220,
#37221,#37222,#37223,#37224,#37225,#37226,#37227,#37228,#37229,#37230,#37231,
#37232,#37233,#37234,#37235,#37236,#37237,#37238,#37239,#37240,#37241,#37242,
#37243,#37244,#37245,#37246,#37247,#37248,#37249,#37250,#37251,#37252,#37253,
#37254,#37255,#37256,#37257,#37258,#37259,#37260,#37261),.UNSPECIFIED.,
 .F.,.F.,(4,3,3,3,3,3,3,3,3,3,3,3,3,3,3,4),(0.119257111071676,0.259765471515195,
0.372070113835674,0.462031695224013,0.560254113799293,0.64563784890186,
0.715250393228207,0.791375724377874,0.847869258158118,0.899498796808649,
0.951835423647897,1.02470756639088,1.07936167344812,1.13215382428839,1.19271226217066,
1.24332399461983),.UNSPECIFIED.);
#994=B_SPLINE_CURVE_WITH_KNOTS('',3,(#37269,#37270,#37271,#37272,#37273,
#37274,#37275,#37276),.UNSPECIFIED.,.F.,.F.,(4,2,2,4),(0.,0.132844661742616,
0.506252230084776,0.808060044866463),.UNSPECIFIED.);
#995=B_SPLINE_CURVE_WITH_KNOTS('',3,(#37280,#37281,#37282,#37283,#37284,
#37285,#37286,#37287,#37288,#37289,#37290,#37291,#37292,#37293,#37294,#37295,
#37296,#37297,#37298,#37299,#37300,#37301,#37302,#37303,#37304,#37305,#37306,
#37307,#37308,#37309,#37310,#37311,#37312,#37313,#37314,#37315,#37316,#37317,
#37318,#37319,#37320,#37321,#37322,#37323,#37324,#37325),.UNSPECIFIED.,
 .F.,.F.,(4,3,3,3,3,3,3,3,3,3,3,3,3,3,3,4),(0.119257111238407,0.259765472915745,
0.372070114012319,0.462031696197013,0.560254114345044,0.645637850634053,
0.715250395662769,0.791375729222669,0.847869263651974,0.89949880268746,
0.951835429736583,1.02470757346672,1.07936168126432,1.13215383237257,1.19271227073433,
1.24332400465711),.UNSPECIFIED.);
#996=B_SPLINE_CURVE_WITH_KNOTS('',3,(#37333,#37334,#37335,#37336,#37337,
#37338,#37339,#37340),.UNSPECIFIED.,.F.,.F.,(4,2,2,4),(0.,0.132844672918338,
0.50625237183672,0.808060292904816),.UNSPECIFIED.);
#997=B_SPLINE_CURVE_WITH_KNOTS('',3,(#37344,#37345,#37346,#37347,#37348,
#37349,#37350,#37351,#37352,#37353,#37354,#37355,#37356,#37357,#37358,#37359,
#37360,#37361,#37362,#37363,#37364,#37365,#37366,#37367,#37368,#37369,#37370,
#37371,#37372,#37373,#37374,#37375,#37376,#37377,#37378,#37379,#37380,#37381,
#37382,#37383,#37384,#37385,#37386,#37387,#37388,#37389),.UNSPECIFIED.,
 .F.,.F.,(4,3,3,3,3,3,3,3,3,3,3,3,3,3,3,4),(0.119257111410954,0.25976547452879,
0.372070109798341,0.462031694258679,0.560254111872906,0.645637849932998,
0.71525039623539,0.791375733920728,0.847869269224843,0.899498808890005,
0.951835436167286,1.02470758121388,1.07936168999882,1.13215384163373,1.1927122800387,
1.24332401635365),.UNSPECIFIED.);
#998=B_SPLINE_CURVE_WITH_KNOTS('',3,(#37397,#37398,#37399,#37400,#37401,
#37402,#37403,#37404),.UNSPECIFIED.,.F.,.F.,(4,2,2,4),(0.,0.132844669264716,
0.51607262788724,0.952446854621337),.UNSPECIFIED.);
#999=B_SPLINE_CURVE_WITH_KNOTS('',3,(#37513,#37514,#37515,#37516,#37517,
#37518),.UNSPECIFIED.,.F.,.F.,(4,2,4),(0.,5.,9.6),.UNSPECIFIED.);
#1000=B_SPLINE_CURVE_WITH_KNOTS('',3,(#37593,#37594,#37595,#37596,#37597,
#37598),.UNSPECIFIED.,.F.,.F.,(4,2,4),(0.,5.,9.6),.UNSPECIFIED.);
#1001=B_SPLINE_CURVE_WITH_KNOTS('',3,(#37672,#37673,#37674,#37675,#37676,
#37677),.UNSPECIFIED.,.F.,.F.,(4,2,4),(0.,5.,9.6),.UNSPECIFIED.);
#1002=B_SPLINE_CURVE_WITH_KNOTS('',3,(#37752,#37753,#37754,#37755,#37756,
#37757),.UNSPECIFIED.,.F.,.F.,(4,2,4),(0.,5.,9.6),.UNSPECIFIED.);
#1003=B_SPLINE_CURVE_WITH_KNOTS('',3,(#37831,#37832,#37833,#37834,#37835,
#37836),.UNSPECIFIED.,.F.,.F.,(4,2,4),(0.,5.,9.6),.UNSPECIFIED.);
#1004=B_SPLINE_CURVE_WITH_KNOTS('',3,(#37911,#37912,#37913,#37914,#37915,
#37916),.UNSPECIFIED.,.F.,.F.,(4,2,4),(0.,5.,9.6),.UNSPECIFIED.);
#1005=B_SPLINE_CURVE_WITH_KNOTS('',3,(#37990,#37991,#37992,#37993,#37994,
#37995),.UNSPECIFIED.,.F.,.F.,(4,2,4),(0.,5.,9.6),.UNSPECIFIED.);
#1006=B_SPLINE_CURVE_WITH_KNOTS('',3,(#38070,#38071,#38072,#38073,#38074,
#38075),.UNSPECIFIED.,.F.,.F.,(4,2,4),(0.,5.,9.6),.UNSPECIFIED.);
#1007=B_SPLINE_CURVE_WITH_KNOTS('',3,(#38149,#38150,#38151,#38152,#38153,
#38154),.UNSPECIFIED.,.F.,.F.,(4,2,4),(0.,5.,9.6),.UNSPECIFIED.);
#1008=B_SPLINE_CURVE_WITH_KNOTS('',3,(#38229,#38230,#38231,#38232,#38233,
#38234),.UNSPECIFIED.,.F.,.F.,(4,2,4),(0.,5.,9.6),.UNSPECIFIED.);
#1009=B_SPLINE_CURVE_WITH_KNOTS('',3,(#38308,#38309,#38310,#38311,#38312,
#38313),.UNSPECIFIED.,.F.,.F.,(4,2,4),(0.,5.,9.6),.UNSPECIFIED.);
#1010=B_SPLINE_CURVE_WITH_KNOTS('',3,(#38388,#38389,#38390,#38391,#38392,
#38393),.UNSPECIFIED.,.F.,.F.,(4,2,4),(0.,5.,9.6),.UNSPECIFIED.);
#1011=B_SPLINE_CURVE_WITH_KNOTS('',3,(#38467,#38468,#38469,#38470,#38471,
#38472),.UNSPECIFIED.,.F.,.F.,(4,2,4),(0.,5.,9.6),.UNSPECIFIED.);
#1012=B_SPLINE_CURVE_WITH_KNOTS('',3,(#38547,#38548,#38549,#38550,#38551,
#38552),.UNSPECIFIED.,.F.,.F.,(4,2,4),(0.,5.,9.6),.UNSPECIFIED.);
#1013=B_SPLINE_CURVE_WITH_KNOTS('',3,(#38626,#38627,#38628,#38629,#38630,
#38631),.UNSPECIFIED.,.F.,.F.,(4,2,4),(0.,5.,9.6),.UNSPECIFIED.);
#1014=B_SPLINE_CURVE_WITH_KNOTS('',3,(#38706,#38707,#38708,#38709,#38710,
#38711),.UNSPECIFIED.,.F.,.F.,(4,2,4),(0.,5.,9.6),.UNSPECIFIED.);
#1015=B_SPLINE_CURVE_WITH_KNOTS('',3,(#38785,#38786,#38787,#38788,#38789,
#38790),.UNSPECIFIED.,.F.,.F.,(4,2,4),(0.,5.,9.6),.UNSPECIFIED.);
#1016=B_SPLINE_CURVE_WITH_KNOTS('',3,(#38865,#38866,#38867,#38868,#38869,
#38870),.UNSPECIFIED.,.F.,.F.,(4,2,4),(0.,5.,9.6),.UNSPECIFIED.);
#1017=B_SPLINE_CURVE_WITH_KNOTS('',3,(#38944,#38945,#38946,#38947,#38948,
#38949),.UNSPECIFIED.,.F.,.F.,(4,2,4),(0.,5.,9.6),.UNSPECIFIED.);
#1018=B_SPLINE_CURVE_WITH_KNOTS('',3,(#39024,#39025,#39026,#39027,#39028,
#39029),.UNSPECIFIED.,.F.,.F.,(4,2,4),(0.,5.,9.6),.UNSPECIFIED.);
#1019=B_SPLINE_CURVE_WITH_KNOTS('',3,(#39103,#39104,#39105,#39106,#39107,
#39108),.UNSPECIFIED.,.F.,.F.,(4,2,4),(0.,5.,9.6),.UNSPECIFIED.);
#1020=B_SPLINE_CURVE_WITH_KNOTS('',3,(#39183,#39184,#39185,#39186,#39187,
#39188),.UNSPECIFIED.,.F.,.F.,(4,2,4),(0.,5.,9.6),.UNSPECIFIED.);
#1021=B_SPLINE_CURVE_WITH_KNOTS('',3,(#39262,#39263,#39264,#39265,#39266,
#39267),.UNSPECIFIED.,.F.,.F.,(4,2,4),(0.,5.,9.6),.UNSPECIFIED.);
#1022=B_SPLINE_CURVE_WITH_KNOTS('',3,(#39342,#39343,#39344,#39345,#39346,
#39347),.UNSPECIFIED.,.F.,.F.,(4,2,4),(0.,5.,9.6),.UNSPECIFIED.);
#1023=B_SPLINE_CURVE_WITH_KNOTS('',3,(#39421,#39422,#39423,#39424,#39425,
#39426),.UNSPECIFIED.,.F.,.F.,(4,2,4),(0.,5.,9.6),.UNSPECIFIED.);
#1024=B_SPLINE_CURVE_WITH_KNOTS('',3,(#39501,#39502,#39503,#39504,#39505,
#39506),.UNSPECIFIED.,.F.,.F.,(4,2,4),(0.,5.,9.6),.UNSPECIFIED.);
#1025=B_SPLINE_CURVE_WITH_KNOTS('',3,(#39580,#39581,#39582,#39583,#39584,
#39585),.UNSPECIFIED.,.F.,.F.,(4,2,4),(0.,5.,9.6),.UNSPECIFIED.);
#1026=B_SPLINE_CURVE_WITH_KNOTS('',3,(#39660,#39661,#39662,#39663,#39664,
#39665),.UNSPECIFIED.,.F.,.F.,(4,2,4),(0.,5.,9.6),.UNSPECIFIED.);
#1027=B_SPLINE_CURVE_WITH_KNOTS('',3,(#39739,#39740,#39741,#39742,#39743,
#39744),.UNSPECIFIED.,.F.,.F.,(4,2,4),(0.,5.,9.6),.UNSPECIFIED.);
#1028=B_SPLINE_CURVE_WITH_KNOTS('',3,(#39819,#39820,#39821,#39822,#39823,
#39824),.UNSPECIFIED.,.F.,.F.,(4,2,4),(0.,5.,9.6),.UNSPECIFIED.);
#1029=B_SPLINE_CURVE_WITH_KNOTS('',3,(#39898,#39899,#39900,#39901,#39902,
#39903),.UNSPECIFIED.,.F.,.F.,(4,2,4),(0.,5.,9.6),.UNSPECIFIED.);
#1030=B_SPLINE_CURVE_WITH_KNOTS('',3,(#39978,#39979,#39980,#39981,#39982,
#39983),.UNSPECIFIED.,.F.,.F.,(4,2,4),(0.,5.,9.6),.UNSPECIFIED.);
#1031=B_SPLINE_CURVE_WITH_KNOTS('',3,(#40057,#40058,#40059,#40060,#40061,
#40062),.UNSPECIFIED.,.F.,.F.,(4,2,4),(0.,5.,9.6),.UNSPECIFIED.);
#1032=B_SPLINE_CURVE_WITH_KNOTS('',3,(#40137,#40138,#40139,#40140,#40141,
#40142),.UNSPECIFIED.,.F.,.F.,(4,2,4),(0.,5.,9.6),.UNSPECIFIED.);
#1033=B_SPLINE_CURVE_WITH_KNOTS('',3,(#40216,#40217,#40218,#40219,#40220,
#40221),.UNSPECIFIED.,.F.,.F.,(4,2,4),(0.,5.,9.6),.UNSPECIFIED.);
#1034=B_SPLINE_CURVE_WITH_KNOTS('',3,(#40296,#40297,#40298,#40299,#40300,
#40301),.UNSPECIFIED.,.F.,.F.,(4,2,4),(0.,5.,9.6),.UNSPECIFIED.);
#1035=B_SPLINE_CURVE_WITH_KNOTS('',3,(#40328,#40329,#40330,#40331,#40332,
#40333,#40334,#40335,#40336,#40337,#40338,#40339,#40340,#40341,#40342,#40343),
 .UNSPECIFIED.,.F.,.F.,(4,3,3,3,3,4),(-4.09293042013078,-3.98360069087754,
-3.48565060451784,-2.98770051815815,-2.48975043179846,-2.07680027204821),
 .UNSPECIFIED.);
#1036=B_SPLINE_CURVE_WITH_KNOTS('',3,(#40346,#40347,#40348,#40349,#40350,
#40351,#40352,#40353,#40354,#40355),.UNSPECIFIED.,.F.,.F.,(4,3,3,4),(0.,
0.497950086359684,0.995900172719378,1.12546250550734),.UNSPECIFIED.);
#1037=B_SPLINE_CURVE_WITH_KNOTS('',3,(#40360,#40361,#40362,#40363,#40364,
#40365,#40366,#40367,#40368,#40369,#40370,#40371,#40372,#40373,#40374,#40375,
#40376,#40377,#40378,#40379,#40380,#40381,#40382,#40383,#40384,#40385,#40386,
#40387,#40388,#40389,#40390,#40391,#40392,#40393,#40394,#40395,#40396,#40397,
#40398,#40399),.UNSPECIFIED.,.F.,.F.,(4,3,3,3,3,3,3,3,3,3,3,3,3,4),(-10.3761157273103,
-9.95900172719384,-9.46105164083415,-8.96310155447445,-8.46515146811476,
-7.96720138175507,-7.46925129539538,-6.97130120903569,-6.473351122676,-5.9754010363163,
-5.47745094995661,-4.97950086359692,-4.48155077723723,-4.09293042013078),
 .UNSPECIFIED.);
#1038=B_SPLINE_CURVE_WITH_KNOTS('',3,(#40400,#40401,#40402,#40403,#40404,
#40405,#40406,#40407,#40408,#40409,#40410,#40411,#40412,#40413,#40414,#40415,
#40416,#40417,#40418,#40419,#40420,#40421,#40422,#40423,#40424,#40425,#40426,
#40427,#40428,#40429,#40430,#40431,#40432,#40433,#40434,#40435,#40436,#40437,
#40438,#40439),.UNSPECIFIED.,.F.,.F.,(4,3,3,3,3,3,3,3,3,3,3,3,3,4),(1.12546250550734,
1.49385025907907,1.99180034543876,2.48975043179845,2.98770051815815,3.48565060451784,
3.98360069087753,4.48155077723722,4.97950086359691,5.47745094995661,5.9754010363163,
6.47335112267599,6.97130120903568,7.40864781268687),.UNSPECIFIED.);
#1039=B_SPLINE_CURVE_WITH_KNOTS('',3,(#40444,#40445,#40446,#40447,#40448,
#40449,#40450,#40451,#40452,#40453,#40454,#40455,#40456,#40457,#40458,#40459,
#40460,#40461,#40462,#40463,#40464,#40465,#40466,#40467,#40468,#40469,#40470,
#40471,#40472,#40473,#40474,#40475,#40476,#40477,#40478,#40479,#40480,#40481,
#40482,#40483,#40484,#40485,#40486),.UNSPECIFIED.,.F.,.F.,(4,3,3,3,3,3,
3,3,3,3,3,3,3,3,4),(-16.65930103449,-16.4323528498698,-15.9344027635101,
-15.4364526771504,-14.9385025907908,-14.4405525044311,-13.9426024180714,
-13.4446523317117,-12.946702245352,-12.4487521589923,-11.9508020726326,
-11.4528519862729,-10.9549018999132,-10.4569518135535,-10.3761157273103),
 .UNSPECIFIED.);
#1040=B_SPLINE_CURVE_WITH_KNOTS('',3,(#40487,#40488,#40489,#40490,#40491,
#40492,#40493,#40494,#40495,#40496,#40497,#40498,#40499,#40500,#40501,#40502,
#40503,#40504,#40505,#40506,#40507,#40508,#40509,#40510,#40511,#40512,#40513,
#40514,#40515,#40516,#40517,#40518,#40519,#40520,#40521,#40522,#40523,#40524,
#40525,#40526,#40527,#40528,#40529),.UNSPECIFIED.,.F.,.F.,(4,3,3,3,3,3,
3,3,3,3,3,3,3,3,4),(7.40864781268687,7.46925129539537,7.96720138175506,
8.46515146811476,8.96310155447445,9.46105164083414,9.95900172719383,10.4569518135535,
10.9549018999132,11.4528519862729,11.9508020726326,12.4487521589923,12.946702245352,
13.4446523317117,13.6918331198665),.UNSPECIFIED.);
#1041=B_SPLINE_CURVE_WITH_KNOTS('',3,(#40534,#40535,#40536,#40537,#40538,
#40539,#40540,#40541,#40542,#40543,#40544,#40545,#40546,#40547,#40548,#40549,
#40550,#40551,#40552,#40553,#40554,#40555,#40556,#40557,#40558,#40559,#40560,
#40561,#40562,#40563,#40564,#40565,#40566,#40567,#40568,#40569,#40570,#40571,
#40572,#40573,#40574,#40575,#40576),.UNSPECIFIED.,.F.,.F.,(4,3,3,3,3,3,
3,3,3,3,3,3,3,3,4),(-22.9424863416695,-22.9057039725458,-22.4077538861861,
-21.9098037998264,-21.4118537134668,-20.9139036271071,-20.4159535407474,
-19.9180034543877,-19.420053368028,-18.9221032816683,-18.4241531953086,
-17.9262031089489,-17.4282530225892,-16.9303029362295,-16.65930103449),
 .UNSPECIFIED.);
#1042=B_SPLINE_CURVE_WITH_KNOTS('',3,(#40577,#40578,#40579,#40580,#40581,
#40582,#40583,#40584,#40585,#40586,#40587,#40588,#40589,#40590,#40591,#40592,
#40593,#40594,#40595,#40596,#40597,#40598,#40599,#40600,#40601,#40602,#40603,
#40604,#40605,#40606,#40607,#40608,#40609,#40610,#40611,#40612,#40613,#40614,
#40615,#40616,#40617,#40618,#40619),.UNSPECIFIED.,.F.,.F.,(4,3,3,3,3,3,
3,3,3,3,3,3,3,3,4),(13.6918331198665,13.9426024180714,14.4405525044311,
14.9385025907907,15.4364526771504,15.9344027635101,16.4323528498698,16.9303029362295,
17.4282530225892,17.9262031089489,18.4241531953086,18.9221032816683,19.420053368028,
19.9180034543877,19.9750184270461),.UNSPECIFIED.);
#1043=B_SPLINE_CURVE_WITH_KNOTS('',3,(#40624,#40625,#40626,#40627,#40628,
#40629,#40630,#40631,#40632,#40633,#40634,#40635,#40636,#40637,#40638,#40639,
#40640,#40641,#40642,#40643,#40644,#40645,#40646,#40647,#40648,#40649,#40650,
#40651,#40652,#40653,#40654,#40655,#40656,#40657,#40658,#40659,#40660,#40661,
#40662,#40663),.UNSPECIFIED.,.F.,.F.,(4,3,3,3,3,3,3,3,3,3,3,3,3,4),(-29.2256716488492,
-28.8811050088621,-28.3831549225024,-27.8852048361428,-27.3872547497831,
-26.8893046634234,-26.3913545770637,-25.893404490704,-25.3954544043443,
-24.8975043179846,-24.3995542316249,-23.9016041452652,-23.4036540589055,
-22.9424863416695),.UNSPECIFIED.);
#1044=B_SPLINE_CURVE_WITH_KNOTS('',3,(#40664,#40665,#40666,#40667,#40668,
#40669,#40670,#40671,#40672,#40673,#40674,#40675,#40676,#40677,#40678,#40679,
#40680,#40681,#40682,#40683,#40684,#40685,#40686,#40687,#40688,#40689,#40690,
#40691,#40692,#40693,#40694,#40695,#40696,#40697,#40698,#40699,#40700,#40701,
#40702,#40703),.UNSPECIFIED.,.F.,.F.,(4,3,3,3,3,3,3,3,3,3,3,3,3,4),(19.9750184270461,
20.4159535407473,20.913903627107,21.4118537134667,21.9098037998264,22.4077538861861,
22.9057039725458,23.4036540589055,23.9016041452652,24.3995542316249,24.8975043179846,
25.3954544043443,25.893404490704,26.2582037342256),.UNSPECIFIED.);
#1045=B_SPLINE_CURVE_WITH_KNOTS('',3,(#40708,#40709,#40710,#40711,#40712,
#40713,#40714,#40715,#40716,#40717,#40718,#40719,#40720,#40721,#40722,#40723,
#40724,#40725,#40726,#40727,#40728,#40729,#40730,#40731,#40732,#40733,#40734,
#40735,#40736,#40737,#40738,#40739,#40740,#40741,#40742,#40743,#40744,#40745,
#40746,#40747,#40748,#40749,#40750),.UNSPECIFIED.,.F.,.F.,(4,3,3,3,3,3,
3,3,3,3,3,3,3,3,4),(-35.5088569560287,-35.3544561315381,-34.8565060451784,
-34.3585559588187,-33.860605872459,-33.3626557860994,-32.8647056997397,
-32.36675561338,-31.8688055270203,-31.3708554406606,-30.8729053543009,-30.3749552679412,
-29.8770051815815,-29.3790550952218,-29.2256716488492),.UNSPECIFIED.);
#1046=B_SPLINE_CURVE_WITH_KNOTS('',3,(#40751,#40752,#40753,#40754,#40755,
#40756,#40757,#40758,#40759,#40760,#40761,#40762,#40763,#40764,#40765,#40766,
#40767,#40768,#40769,#40770,#40771,#40772,#40773,#40774,#40775,#40776,#40777,
#40778,#40779,#40780,#40781,#40782,#40783,#40784,#40785,#40786,#40787,#40788,
#40789,#40790,#40791,#40792,#40793),.UNSPECIFIED.,.F.,.F.,(4,3,3,3,3,3,
3,3,3,3,3,3,3,3,4),(26.2582037342256,26.3913545770637,26.8893046634233,
27.387254749783,27.8852048361427,28.3831549225024,28.8811050088621,29.3790550952218,
29.8770051815815,30.3749552679412,30.8729053543009,31.3708554406606,31.8688055270203,
32.3667556133799,32.5413890414053),.UNSPECIFIED.);
#1047=B_SPLINE_CURVE_WITH_KNOTS('',3,(#40798,#40799,#40800,#40801,#40802,
#40803,#40804,#40805,#40806,#40807,#40808,#40809,#40810,#40811,#40812,#40813,
#40814,#40815,#40816,#40817,#40818,#40819,#40820,#40821,#40822,#40823,#40824,
#40825,#40826,#40827,#40828,#40829,#40830,#40831,#40832,#40833,#40834,#40835,
#40836,#40837),.UNSPECIFIED.,.F.,.F.,(4,3,3,3,3,3,3,3,3,3,3,3,3,4),(-41.7920422632082,
-41.3298571678544,-40.8319070814947,-40.333956995135,-39.8360069087754,
-39.3380568224157,-38.840106736056,-38.3421566496963,-37.8442065633366,
-37.3462564769769,-36.8483063906172,-36.3503563042575,-35.8524062178978,
-35.5088569560287),.UNSPECIFIED.);
#1048=B_SPLINE_CURVE_WITH_KNOTS('',3,(#40838,#40839,#40840,#40841,#40842,
#40843,#40844,#40845,#40846,#40847,#40848,#40849,#40850,#40851,#40852,#40853,
#40854,#40855,#40856,#40857,#40858,#40859,#40860,#40861,#40862,#40863,#40864,
#40865,#40866,#40867,#40868,#40869,#40870,#40871,#40872,#40873,#40874,#40875,
#40876,#40877),.UNSPECIFIED.,.F.,.F.,(4,3,3,3,3,3,3,3,3,3,3,3,3,4),(32.5413890414053,
32.8647056997396,33.3626557860993,33.860605872459,34.3585559588187,34.8565060451784,
35.3544561315381,35.8524062178978,36.3503563042575,36.8483063906172,37.3462564769769,
37.8442065633366,38.3421566496963,38.8245743485848),.UNSPECIFIED.);
#1049=B_SPLINE_CURVE_WITH_KNOTS('',3,(#40882,#40883,#40884,#40885,#40886,
#40887,#40888,#40889,#40890,#40891,#40892,#40893,#40894,#40895,#40896,#40897,
#40898,#40899,#40900,#40901,#40902,#40903,#40904,#40905,#40906,#40907,#40908,
#40909,#40910,#40911,#40912,#40913,#40914,#40915,#40916,#40917,#40918,#40919,
#40920,#40921,#40922,#40923,#40924),.UNSPECIFIED.,.F.,.F.,(4,3,3,3,3,3,
3,3,3,3,3,3,3,3,4),(-48.0752275703879,-47.8032082905304,-47.3052582041707,
-46.807308117811,-46.3093580314513,-45.8114079450917,-45.313457858732,-44.8155077723723,
-44.3175576860126,-43.8196075996529,-43.3216575132932,-42.8237074269335,
-42.3257573405738,-41.8278072542141,-41.7920422632082),.UNSPECIFIED.);
#1050=B_SPLINE_CURVE_WITH_KNOTS('',3,(#40925,#40926,#40927,#40928,#40929,
#40930,#40931,#40932,#40933,#40934,#40935,#40936,#40937,#40938,#40939,#40940,
#40941,#40942,#40943,#40944,#40945,#40946,#40947,#40948,#40949,#40950,#40951,
#40952,#40953,#40954,#40955,#40956,#40957,#40958,#40959,#40960,#40961,#40962,
#40963,#40964,#40965,#40966,#40967),.UNSPECIFIED.,.F.,.F.,(4,3,3,3,3,3,
3,3,3,3,3,3,3,3,4),(38.8245743485848,38.8401067360559,39.3380568224156,
39.8360069087753,40.333956995135,40.8319070814947,41.3298571678544,41.8278072542141,
42.3257573405738,42.8237074269335,43.3216575132932,43.8196075996529,44.3175576860125,
44.8155077723722,45.1077596557645),.UNSPECIFIED.);
#1051=B_SPLINE_CURVE_WITH_KNOTS('',3,(#40972,#40973,#40974,#40975,#40976,
#40977,#40978,#40979,#40980,#40981,#40982,#40983,#40984,#40985,#40986,#40987,
#40988,#40989,#40990,#40991,#40992,#40993,#40994,#40995,#40996,#40997,#40998,
#40999,#41000,#41001,#41002,#41003,#41004,#41005,#41006,#41007,#41008,#41009,
#41010,#41011,#41012,#41013,#41014),.UNSPECIFIED.,.F.,.F.,(4,3,3,3,3,3,
3,3,3,3,3,3,3,3,4),(-54.3584128775674,-54.2765594132064,-53.7786093268467,
-53.280659240487,-52.7827091541273,-52.2847590677677,-51.786808981408,-51.2888588950483,
-50.7909088086886,-50.2929587223289,-49.7950086359692,-49.2970585496095,
-48.7991084632498,-48.3011583768901,-48.0752275703879),.UNSPECIFIED.);
#1052=B_SPLINE_CURVE_WITH_KNOTS('',3,(#41015,#41016,#41017,#41018,#41019,
#41020,#41021,#41022,#41023,#41024,#41025,#41026,#41027,#41028,#41029,#41030,
#41031,#41032,#41033,#41034,#41035,#41036,#41037,#41038,#41039,#41040,#41041,
#41042,#41043,#41044,#41045,#41046,#41047,#41048,#41049,#41050,#41051,#41052,
#41053,#41054,#41055,#41056,#41057),.UNSPECIFIED.,.F.,.F.,(4,3,3,3,3,3,
3,3,3,3,3,3,3,3,4),(45.1077596557645,45.3134578587319,45.8114079450916,
46.3093580314513,46.807308117811,47.3052582041707,47.8032082905304,48.3011583768901,
48.7991084632498,49.2970585496095,49.7950086359692,50.2929587223289,50.7909088086885,
51.2888588950482,51.390944962944),.UNSPECIFIED.);
#1053=B_SPLINE_CURVE_WITH_KNOTS('',3,(#41062,#41063,#41064,#41065,#41066,
#41067,#41068,#41069,#41070,#41071,#41072,#41073,#41074,#41075,#41076,#41077,
#41078,#41079,#41080,#41081,#41082,#41083,#41084,#41085,#41086,#41087,#41088,
#41089,#41090,#41091,#41092,#41093,#41094,#41095,#41096,#41097,#41098,#41099,
#41100,#41101),.UNSPECIFIED.,.F.,.F.,(4,3,3,3,3,3,3,3,3,3,3,3,3,4),(-60.6415981847471,
-60.2519604495227,-59.754010363163,-59.2560602768033,-58.7581101904437,
-58.260160104084,-57.7622100177243,-57.2642599313646,-56.7663098450049,
-56.2683597586452,-55.7704096722855,-55.2724595859258,-54.7745094995661,
-54.3584128775674),.UNSPECIFIED.);
#1054=B_SPLINE_CURVE_WITH_KNOTS('',3,(#41102,#41103,#41104,#41105,#41106,
#41107,#41108,#41109,#41110,#41111,#41112,#41113,#41114,#41115,#41116,#41117,
#41118,#41119,#41120,#41121,#41122,#41123,#41124,#41125,#41126,#41127,#41128,
#41129,#41130,#41131,#41132,#41133,#41134,#41135,#41136,#41137,#41138,#41139,
#41140,#41141),.UNSPECIFIED.,.F.,.F.,(4,3,3,3,3,3,3,3,3,3,3,3,3,4),(51.390944962944,
51.7868089814079,52.2847590677676,52.7827091541273,53.280659240487,53.7786093268467,
54.2765594132064,54.7745094995661,55.2724595859258,55.7704096722855,56.2683597586451,
56.7663098450048,57.2642599313645,57.6741302701237),.UNSPECIFIED.);
#1055=B_SPLINE_CURVE_WITH_KNOTS('',3,(#41146,#41147,#41148,#41149,#41150,
#41151,#41152,#41153,#41154,#41155,#41156,#41157,#41158,#41159,#41160,#41161,
#41162,#41163,#41164,#41165,#41166,#41167,#41168,#41169,#41170,#41171,#41172,
#41173,#41174,#41175,#41176,#41177,#41178,#41179,#41180,#41181,#41182,#41183,
#41184,#41185,#41186,#41187,#41188),.UNSPECIFIED.,.F.,.F.,(4,3,3,3,3,3,
3,3,3,3,3,3,3,3,4),(-66.9247834919266,-66.7253115721987,-66.227361485839,
-65.7294113994793,-65.2314613131196,-64.73351122676,-64.2355611404003,-63.7376110540406,
-63.2396609676809,-62.7417108813212,-62.2437607949615,-61.7458107086018,
-61.2478606222421,-60.7499105358824,-60.6415981847471),.UNSPECIFIED.);
#1056=B_SPLINE_CURVE_WITH_KNOTS('',3,(#41189,#41190,#41191,#41192,#41193,
#41194,#41195,#41196,#41197,#41198,#41199,#41200,#41201,#41202,#41203,#41204,
#41205,#41206,#41207,#41208,#41209,#41210,#41211,#41212,#41213,#41214,#41215,
#41216,#41217,#41218,#41219,#41220,#41221,#41222,#41223,#41224,#41225,#41226,
#41227,#41228,#41229,#41230,#41231),.UNSPECIFIED.,.F.,.F.,(4,3,3,3,3,3,
3,3,3,3,3,3,3,3,4),(57.6741302701237,57.7622100177242,58.2601601040839,
58.7581101904436,59.2560602768033,59.754010363163,60.2519604495227,60.7499105358824,
61.2478606222421,61.7458107086018,62.2437607949614,62.7417108813211,63.2396609676808,
63.7376110540405,63.9573155773032),.UNSPECIFIED.);
#1057=B_SPLINE_CURVE_WITH_KNOTS('',3,(#41236,#41237,#41238,#41239,#41240,
#41241,#41242,#41243,#41244,#41245,#41246,#41247,#41248,#41249,#41250,#41251,
#41252,#41253,#41254,#41255,#41256,#41257,#41258,#41259,#41260,#41261,#41262,
#41263,#41264,#41265,#41266,#41267,#41268,#41269,#41270,#41271,#41272,#41273,
#41274,#41275,#41276,#41277,#41278),.UNSPECIFIED.,.F.,.F.,(4,3,3,3,3,3,
3,3,3,3,3,3,3,3,4),(-73.2079687991063,-73.1986626948747,-72.700712608515,
-72.2027625221553,-71.7048124357956,-71.206862349436,-70.7089122630762,
-70.2109621767165,-69.7130120903569,-69.2150620039972,-68.7171119176375,
-68.2191618312778,-67.7212117449181,-67.2232616585584,-66.9247834919266),
 .UNSPECIFIED.);
#1058=B_SPLINE_CURVE_WITH_KNOTS('',3,(#41279,#41280,#41281,#41282,#41283,
#41284,#41285,#41286,#41287,#41288,#41289,#41290,#41291,#41292,#41293,#41294,
#41295,#41296,#41297,#41298,#41299,#41300,#41301,#41302,#41303,#41304,#41305,
#41306,#41307,#41308,#41309,#41310,#41311,#41312,#41313,#41314,#41315,#41316,
#41317,#41318,#41319,#41320,#41321),.UNSPECIFIED.,.F.,.F.,(4,3,3,3,3,3,
3,3,3,3,3,3,3,3,4),(63.9573155773032,64.2355611404002,64.7335112267599,
65.2314613131196,65.7294113994793,66.227361485839,66.7253115721987,67.2232616585584,
67.7212117449181,68.2191618312777,68.7171119176374,69.2150620039971,69.7130120903568,
70.2109621767165,70.2405008844829),.UNSPECIFIED.);
#1059=B_SPLINE_CURVE_WITH_KNOTS('',3,(#41326,#41327,#41328,#41329,#41330,
#41331,#41332,#41333,#41334,#41335,#41336,#41337,#41338,#41339,#41340,#41341,
#41342,#41343,#41344,#41345,#41346,#41347,#41348,#41349,#41350,#41351,#41352,
#41353,#41354,#41355,#41356,#41357,#41358,#41359,#41360,#41361,#41362,#41363,
#41364,#41365),.UNSPECIFIED.,.F.,.F.,(4,3,3,3,3,3,3,3,3,3,3,3,3,4),(-79.4911541062858,
-79.174063731191,-78.6761136448313,-78.1781635584716,-77.6802134721119,
-77.1822633857523,-76.6843132993926,-76.1863632130329,-75.6884131266732,
-75.1904630403135,-74.6925129539538,-74.1945628675941,-73.6966127812344,
-73.2079687991063),.UNSPECIFIED.);
#1060=B_SPLINE_CURVE_WITH_KNOTS('',3,(#41366,#41367,#41368,#41369,#41370,
#41371,#41372,#41373,#41374,#41375,#41376,#41377,#41378,#41379,#41380,#41381,
#41382,#41383,#41384,#41385,#41386,#41387,#41388,#41389,#41390,#41391,#41392,
#41393,#41394,#41395,#41396,#41397,#41398,#41399,#41400,#41401,#41402,#41403,
#41404,#41405),.UNSPECIFIED.,.F.,.F.,(4,3,3,3,3,3,3,3,3,3,3,3,3,4),(70.2405008844829,
70.7089122630762,71.2068623494359,71.7048124357956,72.2027625221553,72.7007126085149,
73.1986626948746,73.6966127812344,74.194562867594,74.6925129539537,75.1904630403134,
75.6884131266731,76.1863632130328,76.5236861916624),.UNSPECIFIED.);
#1061=B_SPLINE_CURVE_WITH_KNOTS('',3,(#41411,#41412,#41413,#41414),
 .UNSPECIFIED.,.F.,.F.,(4,4),(91.106186954104,91.2020467387594),
 .UNSPECIFIED.);
#1062=B_SPLINE_CURVE_WITH_KNOTS('',3,(#41420,#41421,#41422,#41423,#41424,
#41425,#41426,#41427,#41428,#41429,#41430,#41431,#41432,#41433,#41434,#41435),
 .UNSPECIFIED.,.F.,.F.,(4,1,1,1,1,1,1,1,1,1,1,1,1,4),(84.8230016469245,
85.3116456290525,85.8095957154122,86.3075458017719,86.8054958881316,87.3034459744913,
87.801396060851,88.2993461472107,88.7972962335704,89.2952463199301,89.7931964062898,
90.2911464926494,90.7890965790091,91.106186954104),.UNSPECIFIED.);
#1063=B_SPLINE_CURVE_WITH_KNOTS('',3,(#41438,#41439,#41440,#41441,#41442,
#41443,#41444,#41445,#41446,#41447,#41448,#41449,#41450,#41451),
 .UNSPECIFIED.,.F.,.F.,(4,1,1,1,1,1,1,1,1,1,1,4),(84.8230016469243,84.9836287546544,
85.4815788410141,85.9795289273738,86.4774790137335,86.9754291000932,87.4733791864529,
87.9713292728126,88.4692793591723,88.967229445532,89.4651795318917,89.9631296182514),
 .UNSPECIFIED.);
#1064=B_SPLINE_CURVE_WITH_KNOTS('',3,(#41456,#41457,#41458,#41459,#41460,
#41461,#41462,#41463,#41464,#41465,#41466,#41467,#41468,#41469,#41470,#41471,
#41472),.UNSPECIFIED.,.F.,.F.,(4,1,1,1,1,1,1,1,1,1,1,1,1,1,4),(78.5398163397448,
78.8382945063765,79.3362445927362,79.8341946790959,80.3321447654556,80.8300948518153,
81.328044938175,81.8259950245347,82.3239451108944,82.8218951972541,83.3198452836138,
83.8177953699735,84.3157454563331,84.8136955426928,84.8230016469245),
 .UNSPECIFIED.);
#1065=B_SPLINE_CURVE_WITH_KNOTS('',3,(#41473,#41474,#41475,#41476,#41477,
#41478,#41479,#41480,#41481,#41482,#41483,#41484,#41485,#41486,#41487,#41488),
 .UNSPECIFIED.,.F.,.F.,(4,1,1,1,1,1,1,1,1,1,1,1,1,4),(78.5398163397448,
79.0082277183381,79.5061778046978,80.0041278910575,80.5020779774172,81.0000280637769,
81.4979781501366,81.9959282364963,82.493878322856,82.9918284092157,83.4897784955754,
83.9877285819351,84.4856786682948,84.8230016469243),.UNSPECIFIED.);
#1066=B_SPLINE_CURVE_WITH_KNOTS('',3,(#41493,#41494,#41495,#41496,#41497,
#41498,#41499,#41500,#41501,#41502,#41503,#41504,#41505,#41506,#41507,#41508,
#41509),.UNSPECIFIED.,.F.,.F.,(4,1,1,1,1,1,1,1,1,1,1,1,1,1,4),(72.2566310325653,
72.3649433837005,72.8628934700602,73.3608435564199,73.8587936427796,74.3567437291393,
74.854693815499,75.3526439018587,75.8505939882184,76.3485440745781,76.8464941609378,
77.3444442472975,77.8423943336572,78.3403444200168,78.5398163397448),
 .UNSPECIFIED.);
#1067=B_SPLINE_CURVE_WITH_KNOTS('',3,(#41510,#41511,#41512,#41513,#41514,
#41515,#41516,#41517,#41518,#41519,#41520,#41521,#41522,#41523,#41524,#41525,
#41526),.UNSPECIFIED.,.F.,.F.,(4,1,1,1,1,1,1,1,1,1,1,1,1,1,4),(72.2566310325653,
72.5348765956622,73.0328266820218,73.5307767683815,74.0287268547412,74.5266769411009,
75.0246270274606,75.5225771138203,76.02052720018,76.5184772865397,77.0164273728994,
77.5143774592591,78.0123275456188,78.5102776319785,78.5398163397448),
 .UNSPECIFIED.);
#1068=B_SPLINE_CURVE_WITH_KNOTS('',3,(#41531,#41532,#41533,#41534,#41535,
#41536,#41537,#41538,#41539,#41540,#41541,#41542,#41543,#41544,#41545,#41546),
 .UNSPECIFIED.,.F.,.F.,(4,1,1,1,1,1,1,1,1,1,1,1,1,4),(65.9734457253856,
66.3895423473842,66.8874924337439,67.3854425201036,67.8833926064633,68.381342692823,
68.8792927791827,69.3772428655424,69.8751929519021,70.3731430382618,70.8710931246215,
71.3690432109811,71.8669932973408,72.2566310325653),.UNSPECIFIED.);
#1069=B_SPLINE_CURVE_WITH_KNOTS('',3,(#41547,#41548,#41549,#41550,#41551,
#41552,#41553,#41554,#41555,#41556,#41557,#41558,#41559,#41560,#41561,#41562,
#41563),.UNSPECIFIED.,.F.,.F.,(4,1,1,1,1,1,1,1,1,1,1,1,1,1,4),(65.9734457253856,
66.0615254729862,66.5594755593459,67.0574256457055,67.5553757320652,68.0533258184249,
68.5512759047846,69.0492259911443,69.547176077504,70.0451261638637,70.5430762502234,
71.0410263365831,71.5389764229428,72.0369265093025,72.2566310325653),
 .UNSPECIFIED.);
#1070=B_SPLINE_CURVE_WITH_KNOTS('',3,(#41568,#41569,#41570,#41571,#41572,
#41573,#41574,#41575,#41576,#41577,#41578,#41579,#41580,#41581,#41582,#41583,
#41584),.UNSPECIFIED.,.F.,.F.,(4,1,1,1,1,1,1,1,1,1,1,1,1,1,4),(59.6902604182061,
59.9161912247082,60.4141413110679,60.9120913974276,61.4100414837873,61.907991570147,
62.4059416565067,62.9038917428664,63.4018418292261,63.8997919155858,64.3977420019455,
64.8956920883052,65.3936421746648,65.8915922610245,65.9734457253856),
 .UNSPECIFIED.);
#1071=B_SPLINE_CURVE_WITH_KNOTS('',3,(#41585,#41586,#41587,#41588,#41589,
#41590,#41591,#41592,#41593,#41594,#41595,#41596,#41597,#41598,#41599,#41600),
 .UNSPECIFIED.,.F.,.F.,(4,1,1,1,1,1,1,1,1,1,1,1,1,4),(59.6902604182061,
60.0861244366699,60.5840745230296,61.0820246093893,61.5799746957489,62.0779247821086,
62.5758748684683,63.073824954828,63.5717750411877,64.0697251275474,64.5676752139071,
65.0656253002668,65.5635753866265,65.9734457253856),.UNSPECIFIED.);
#1072=B_SPLINE_CURVE_WITH_KNOTS('',3,(#41605,#41606,#41607,#41608,#41609,
#41610,#41611,#41612,#41613,#41614,#41615,#41616,#41617,#41618,#41619,#41620,
#41621),.UNSPECIFIED.,.F.,.F.,(4,1,1,1,1,1,1,1,1,1,1,1,1,1,4),(53.4070751110264,
53.4428401020322,53.9407901883919,54.4387402747516,54.9366903611113,55.434640447471,
55.9325905338307,56.4305406201904,56.9284907065501,57.4264407929098,57.9243908792695,
58.4223409656292,58.9202910519889,59.4182411383485,59.6902604182061),
 .UNSPECIFIED.);
#1073=B_SPLINE_CURVE_WITH_KNOTS('',3,(#41622,#41623,#41624,#41625,#41626,
#41627,#41628,#41629,#41630,#41631,#41632,#41633,#41634,#41635,#41636,#41637,
#41638),.UNSPECIFIED.,.F.,.F.,(4,1,1,1,1,1,1,1,1,1,1,1,1,1,4),(53.4070751110264,
53.6127733139939,54.1107234003536,54.6086734867133,55.106623573073,55.6045736594326,
56.1025237457923,56.600473832152,57.0984239185117,57.5963740048714,58.0943240912311,
58.5922741775908,59.0902242639505,59.5881743503102,59.6902604182061),
 .UNSPECIFIED.);
#1074=B_SPLINE_CURVE_WITH_KNOTS('',3,(#41643,#41644,#41645,#41646,#41647,
#41648,#41649,#41650,#41651,#41652,#41653,#41654,#41655,#41656,#41657,#41658),
 .UNSPECIFIED.,.F.,.F.,(4,1,1,1,1,1,1,1,1,1,1,1,1,4),(47.1238898038469,
47.4674390657159,47.9653891520756,48.4633392384353,48.961289324795,49.4592394111547,
49.9571894975144,50.4551395838741,50.9530896702338,51.4510397565935,51.9489898429532,
52.4469399293129,52.9448900156726,53.4070751110264),.UNSPECIFIED.);
#1075=B_SPLINE_CURVE_WITH_KNOTS('',3,(#41659,#41660,#41661,#41662,#41663,
#41664,#41665,#41666,#41667,#41668,#41669,#41670,#41671,#41672,#41673,#41674,
#41675),.UNSPECIFIED.,.F.,.F.,(4,1,1,1,1,1,1,1,1,1,1,1,1,1,4),(47.1238898038469,
47.1394221913179,47.6373722776776,48.1353223640373,48.633272450397,49.1312225367567,
49.6291726231163,50.127122709476,50.6250727958357,51.1230228821954,51.6209729685551,
52.1189230549148,52.6168731412745,53.1148232276342,53.4070751110264),
 .UNSPECIFIED.);
#1076=B_SPLINE_CURVE_WITH_KNOTS('',3,(#41680,#41681,#41682,#41683,#41684,
#41685,#41686,#41687,#41688,#41689,#41690,#41691,#41692,#41693,#41694,#41695,
#41696),.UNSPECIFIED.,.F.,.F.,(4,1,1,1,1,1,1,1,1,1,1,1,1,1,4),(40.8407044966672,
40.9940879430399,41.4920380293996,41.9899881157593,42.487938202119,42.9858882884787,
43.4838383748384,43.9817884611981,44.4797385475578,44.9776886339175,45.4756387202772,
45.9735888066369,46.4715388929966,46.9694889793562,47.1238898038469),
 .UNSPECIFIED.);
#1077=B_SPLINE_CURVE_WITH_KNOTS('',3,(#41697,#41698,#41699,#41700,#41701,
#41702,#41703,#41704,#41705,#41706,#41707,#41708,#41709,#41710,#41711,#41712),
 .UNSPECIFIED.,.F.,.F.,(4,1,1,1,1,1,1,1,1,1,1,1,1,4),(40.8407044966672,
41.1640211550016,41.6619712413613,42.159921327721,42.6578714140807,43.1558215004404,
43.6537715868,44.1517216731597,44.6496717595194,45.1476218458791,45.6455719322388,
46.1435220185985,46.6414721049582,47.1238898038469),.UNSPECIFIED.);
#1078=B_SPLINE_CURVE_WITH_KNOTS('',3,(#41717,#41718,#41719,#41720,#41721,
#41722,#41723,#41724,#41725,#41726,#41727,#41728,#41729,#41730,#41731,#41732),
 .UNSPECIFIED.,.F.,.F.,(4,1,1,1,1,1,1,1,1,1,1,1,1,4),(34.5575191894877,
35.0186869067236,35.5166369930833,36.014587079443,36.5125371658027,37.0104872521624,
37.5084373385221,38.0063874248818,38.5043375112415,39.0022875976012,39.5002376839609,
39.9981877703206,40.4961378566802,40.8407044966672),.UNSPECIFIED.);
#1079=B_SPLINE_CURVE_WITH_KNOTS('',3,(#41733,#41734,#41735,#41736,#41737,
#41738,#41739,#41740,#41741,#41742,#41743,#41744,#41745,#41746,#41747,#41748,
#41749),.UNSPECIFIED.,.F.,.F.,(4,1,1,1,1,1,1,1,1,1,1,1,1,1,4),(34.5575191894877,
34.6906700323256,35.1886201186853,35.686570205045,36.1845202914047,36.6824703777644,
37.1804204641241,37.6783705504837,38.1763206368434,38.6742707232031,39.1722208095628,
39.6701708959225,40.1681209822822,40.6660710686419,40.8407044966672),
 .UNSPECIFIED.);
#1080=B_SPLINE_CURVE_WITH_KNOTS('',3,(#41754,#41755,#41756,#41757,#41758,
#41759,#41760,#41761,#41762,#41763,#41764,#41765,#41766,#41767,#41768,#41769,
#41770),.UNSPECIFIED.,.F.,.F.,(4,1,1,1,1,1,1,1,1,1,1,1,1,1,4),(28.2743338823082,
28.5453357840476,29.0432858704073,29.541235956767,30.0391860431267,30.5371361294864,
31.0350862158461,31.5330363022058,32.0309863885655,32.5289364749252,33.0268865612849,
33.5248366476446,34.0227867340043,34.520736820364,34.5575191894877),
 .UNSPECIFIED.);
#1081=B_SPLINE_CURVE_WITH_KNOTS('',3,(#41771,#41772,#41773,#41774,#41775,
#41776,#41777,#41778,#41779,#41780,#41781,#41782,#41783,#41784,#41785,#41786),
 .UNSPECIFIED.,.F.,.F.,(4,1,1,1,1,1,1,1,1,1,1,1,1,4),(28.274333882308,28.7152689960093,
29.213219082369,29.7111691687287,30.2091192550884,30.7070693414481,31.2050194278078,
31.7029695141674,32.2009196005271,32.6988696868868,33.1968197732465,33.6947698596062,
34.1927199459659,34.5575191894877),.UNSPECIFIED.);
#1082=B_SPLINE_CURVE_WITH_KNOTS('',3,(#41791,#41792,#41793,#41794,#41795,
#41796,#41797,#41798,#41799,#41800,#41801,#41802,#41803,#41804,#41805,#41806,
#41807),.UNSPECIFIED.,.F.,.F.,(4,1,1,1,1,1,1,1,1,1,1,1,1,1,4),(21.9911485751285,
22.0719846613717,22.5699347477313,23.067884834091,23.5658349204507,24.0637850068104,
24.5617350931701,25.0596851795298,25.5576352658895,26.0555853522492,26.5535354386089,
27.0514855249686,27.5494356113283,28.047385697688,28.2743338823082),
 .UNSPECIFIED.);
#1083=B_SPLINE_CURVE_WITH_KNOTS('',3,(#41808,#41809,#41810,#41811,#41812,
#41813,#41814,#41815,#41816,#41817,#41818,#41819,#41820,#41821,#41822,#41823,
#41824),.UNSPECIFIED.,.F.,.F.,(4,1,1,1,1,1,1,1,1,1,1,1,1,1,4),(21.9911485751285,
22.2419178733333,22.739867959693,23.2378180460527,23.7357681324124,24.2337182187721,
24.7316683051318,25.2296183914915,25.7275684778511,26.2255185642108,26.7234686505705,
27.2214187369302,27.7193688232899,28.2173189096496,28.274333882308),
 .UNSPECIFIED.);
#1084=B_SPLINE_CURVE_WITH_KNOTS('',3,(#41829,#41830,#41831,#41832,#41833,
#41834,#41835,#41836,#41837,#41838,#41839,#41840,#41841,#41842,#41843,#41844),
 .UNSPECIFIED.,.F.,.F.,(4,1,1,1,1,1,1,1,1,1,1,1,1,4),(15.707963267949,16.0965836250554,
16.594533711415,17.0924837977747,17.5904338841344,18.0883839704941,18.5863340568538,
19.0842841432135,19.5822342295732,20.0801843159329,20.5781344022926,21.0760844886523,
21.574034575012,21.9911485751285),.UNSPECIFIED.);
#1085=B_SPLINE_CURVE_WITH_KNOTS('',3,(#41845,#41846,#41847,#41848,#41849,
#41850,#41851,#41852,#41853,#41854,#41855,#41856,#41857,#41858,#41859,#41860,
#41861),.UNSPECIFIED.,.F.,.F.,(4,1,1,1,1,1,1,1,1,1,1,1,1,1,4),(15.707963267949,
15.7685667506573,16.266516837017,16.7644669233767,17.2624170097364,17.7603670960961,
18.2583171824558,18.7562672688155,19.2542173551752,19.7521674415349,20.2501175278945,
20.7480676142542,21.2460177006139,21.7439677869736,21.9911485751285),
 .UNSPECIFIED.);
#1086=B_SPLINE_CURVE_WITH_KNOTS('',3,(#41864,#41865,#41866,#41867,#41868,
#41869,#41870,#41871,#41872,#41873,#41874,#41875,#41876,#41877,#41878,#41879,
#41880,#41881,#41882,#41883,#41884,#41885,#41886,#41887,#41888,#41889,#41890,
#41891,#41892,#41893,#41894,#41895,#41896,#41897,#41898,#41899,#41900,#41901,
#41902,#41903,#41904,#41905,#41906,#41907,#41908,#41909,#41910,#41911,#41912,
#41913,#41914,#41915,#41916,#41917,#41918,#41919,#41920,#41921,#41922,#41923,
#41924,#41925,#41926,#41927,#41928,#41929,#41930,#41931,#41932,#41933,#41934,
#41935,#41936,#41937,#41938,#41939,#41940,#41941,#41942),.UNSPECIFIED.,
 .F.,.F.,(4,3,3,3,3,3,3,3,3,3,3,3,3,3,3,3,3,3,3,3,3,3,3,3,3,3,4),(-2.30573780455543,
-2.21841113392645,-2.08749160267076,-2.03463636793378,-2.00263204080081,
-1.86521061460393,-1.77569625734445,-1.73401588570404,-1.69473300890369,
-1.55556413645857,-1.41514237879565,-1.33427014934624,-1.30800108531491,
-1.16478112610678,-1.14989664424401,-1.00863390696719,-0.941358480514188,
-0.905079352339792,-0.875958582765696,-0.729465446527128,-0.584845695136702,
-0.511739983244614,-0.464615362770142,-0.437368675712909,-0.289286735155622,
-0.139857796807127,0.),.UNSPECIFIED.);
#1087=B_SPLINE_CURVE_WITH_KNOTS('',3,(#41947,#41948,#41949,#41950,#41951,
#41952,#41953,#41954,#41955,#41956,#41957,#41958,#41959,#41960,#41961,#41962,
#41963,#41964,#41965,#41966,#41967,#41968,#41969,#41970,#41971,#41972,#41973,
#41974,#41975,#41976,#41977,#41978,#41979,#41980,#41981,#41982,#41983,#41984,
#41985,#41986,#41987,#41988,#41989,#41990,#41991,#41992,#41993,#41994,#41995,
#41996,#41997,#41998,#41999,#42000,#42001,#42002,#42003,#42004,#42005,#42006,
#42007,#42008,#42009,#42010,#42011,#42012,#42013,#42014,#42015,#42016,#42017,
#42018,#42019,#42020,#42021,#42022,#42023,#42024,#42025,#42026,#42027,#42028),
 .UNSPECIFIED.,.F.,.F.,(4,3,3,3,3,3,3,3,3,3,3,3,3,3,3,3,3,3,3,3,3,3,3,3,
3,3,3,4),(-2.29817876007981,-2.19741091509423,-2.05273312368805,-1.99504166905861,
-1.96232249553947,-1.81492097586906,-1.71681036266927,-1.68268796625865,
-1.65188428124604,-1.61869974946949,-1.47364208734527,-1.32963263754991,
-1.25161162956993,-1.22444539494046,-1.08298576005188,-1.05905266124946,
-0.924129685546555,-0.862356703818927,-0.817065087590977,-0.790581206788844,
-0.652351590986891,-0.519360758437836,-0.454238466605207,-0.402777609553242,
-0.376224313666366,-0.240439074152116,-0.107056245968069,0.),
 .UNSPECIFIED.);
#1088=B_SPLINE_CURVE_WITH_KNOTS('',3,(#42697,#42698,#42699,#42700,#42701,
#42702,#42703,#42704,#42705,#42706,#42707,#42708,#42709,#42710,#42711,#42712,
#42713,#42714,#42715,#42716,#42717,#42718),.UNSPECIFIED.,.F.,.F.,(4,3,3,
3,3,3,3,4),(76.5236861916624,76.6843132993925,77.1822633857522,77.6802134721119,
78.1781635584716,78.6761136448312,79.1740637311909,79.5870138909412),
 .UNSPECIFIED.);
#1089=B_SPLINE_CURVE_WITH_KNOTS('',3,(#42720,#42721,#42722,#42723,#42724,
#42725,#42726,#42727,#42728,#42729,#42730,#42731,#42732,#42733,#42734,#42735,
#42736,#42737,#42738,#42739,#42740,#42741,#42742,#42743,#42744,#42745,#42746,
#42747,#42748,#42749,#42750,#42751,#42752,#42753,#42754,#42755,#42756,#42757,
#42758,#42759,#42760,#42761,#42762,#42763,#42764,#42765,#42766,#42767,#42768,
#42769,#42770,#42771,#42772,#42773,#42774,#42775,#42776,#42777,#42778,#42779,
#42780,#42781,#42782,#42783,#42784,#42785,#42786,#42787,#42788,#42789,#42790,
#42791,#42792,#42793,#42794,#42795,#42796,#42797,#42798),.UNSPECIFIED.,
 .F.,.F.,(4,3,3,3,3,3,3,3,3,3,3,3,3,3,3,3,3,3,3,3,3,3,3,3,3,3,4),(-2.30573780455542,
-2.2184111339264,-2.08749160267071,-2.03463636764165,-2.00263204069499,
-1.86521061414297,-1.77569625699512,-1.73401588567174,-1.69473300890364,
-1.555564136972,-1.41514237955304,-1.33427015017412,-1.3080010854375,-1.16478112641558,
-1.14989664424397,-1.00863390696714,-0.94135847965341,-0.905079350045409,
-0.875958582289399,-0.729465445933032,-0.584845695136671,-0.511739983244587,
-0.464615363394834,-0.437368676240646,-0.289286726941639,-0.139857794152545,
0.),.UNSPECIFIED.);
#1090=B_SPLINE_CURVE_WITH_KNOTS('',3,(#42799,#42800,#42801,#42802,#42803,
#42804,#42805,#42806,#42807,#42808,#42809,#42810,#42811,#42812),
 .UNSPECIFIED.,.F.,.F.,(4,1,1,1,1,1,1,1,1,1,1,4),(10.3761157273102,10.7890658870604,
11.2870159734201,11.7849660597798,12.2829161461395,12.7808662324992,13.2788163188589,
13.7767664052186,14.2747164915782,14.7726665779379,15.2706166642976,15.707963267949),
 .UNSPECIFIED.);
#1091=B_SPLINE_CURVE_WITH_KNOTS('',3,(#42818,#42819,#42820,#42821,#42822,
#42823,#42824,#42825,#42826,#42827,#42828,#42829,#42830,#42831,#42832,#42833,
#42834,#42835,#42836,#42837,#42838,#42839,#42840,#42841,#42842,#42843,#42844,
#42845,#42846,#42847,#42848,#42849,#42850,#42851,#42852,#42853,#42854,#42855,
#42856,#42857,#42858,#42859,#42860,#42861,#42862,#42863,#42864,#42865,#42866,
#42867,#42868,#42869,#42870,#42871,#42872,#42873,#42874,#42875,#42876,#42877,
#42878,#42879,#42880,#42881,#42882,#42883,#42884,#42885,#42886,#42887,#42888,
#42889,#42890,#42891,#42892,#42893,#42894,#42895,#42896,#42897,#42898,#42899),
 .UNSPECIFIED.,.F.,.F.,(4,3,3,3,3,3,3,3,3,3,3,3,3,3,3,3,3,3,3,3,3,3,3,3,
3,3,3,4),(-2.29817876007991,-2.19741091509428,-2.05273312368808,-1.99504166925756,
-1.96232249570202,-1.81492097587876,-1.71681036267412,-1.68268796661413,
-1.6518842813445,-1.61869974946948,-1.47364208662842,-1.32963263430615,
-1.25161162484676,-1.22444539341282,-1.08298575668718,-1.05905266124945,
-0.924129685546546,-0.862356703698319,-0.817065087328252,-0.790581206971903,
-0.652351598429523,-0.519360758437847,-0.454238469053417,-0.40277761002181,
-0.37622431360753,-0.240439072833657,-0.107056229103949,0.),
 .UNSPECIFIED.);
#1092=B_SPLINE_CURVE_WITH_KNOTS('',3,(#42902,#42903,#42904,#42905,#42906,
#42907,#42908,#42909,#42910,#42911,#42912,#42913),.UNSPECIFIED.,.F.,.F.,
(4,1,1,1,1,1,1,1,1,4),(11.6150328478181,12.1129829341778,12.6109330205375,
13.1088831068972,13.6068331932569,14.1047832796166,14.6027333659763,15.100683452336,
15.5986335386957,15.707963267949),.UNSPECIFIED.);
#1093=B_SPLINE_CURVE_WITH_KNOTS('',3,(#43582,#43583,#43584,#43585,#43586,
#43587,#43588,#43589,#43590,#43591,#43592,#43593,#43594,#43595,#43596,#43597),
 .UNSPECIFIED.,.F.,.F.,(4,3,3,3,3,4),(-81.6638141629894,-81.1658640766298,
-80.6679139902701,-80.1699639039104,-79.6720138175507,-79.4911541062858),
 .UNSPECIFIED.);
#1094=B_SPLINE_CURVE_WITH_KNOTS('',3,(#43666,#43667,#43668,#43669),
 .UNSPECIFIED.,.F.,.F.,(4,4),(0.,0.203579345120206),.UNSPECIFIED.);
#1095=B_SPLINE_CURVE_WITH_KNOTS('',3,(#43707,#43708,#43709,#43710),
 .UNSPECIFIED.,.F.,.F.,(4,4),(0.,0.203579415270987),.UNSPECIFIED.);
#1096=B_SPLINE_CURVE_WITH_KNOTS('',3,(#43788,#43789,#43790,#43791),
 .UNSPECIFIED.,.F.,.F.,(4,4),(0.,0.211711806319391),.UNSPECIFIED.);
#1097=B_SPLINE_CURVE_WITH_KNOTS('',3,(#43865,#43866,#43867,#43868),
 .UNSPECIFIED.,.F.,.F.,(4,4),(0.,0.207414265317584),.UNSPECIFIED.);
#1098=B_SPLINE_CURVE_WITH_KNOTS('',3,(#43945,#43946,#43947,#43948),
 .UNSPECIFIED.,.F.,.F.,(4,4),(0.,0.21653079565574),.UNSPECIFIED.);
#1099=B_SPLINE_CURVE_WITH_KNOTS('',3,(#43992,#43993,#43994,#43995),
 .UNSPECIFIED.,.F.,.F.,(4,4),(0.,0.207414336599568),.UNSPECIFIED.);
#1100=B_SPLINE_CURVE_WITH_KNOTS('',3,(#43999,#44000,#44001,#44002),
 .UNSPECIFIED.,.F.,.F.,(4,4),(0.,0.211711879270631),.UNSPECIFIED.);
#1101=B_SPLINE_CURVE_WITH_KNOTS('',3,(#44008,#44009,#44010,#44011),
 .UNSPECIFIED.,.F.,.F.,(4,4),(0.,0.216530870858263),.UNSPECIFIED.);
#1102=B_SPLINE_CURVE_WITH_KNOTS('',3,(#44335,#44336,#44337,#44338,#44339,
#44340,#44341,#44342,#44343,#44344,#44345,#44346,#44347,#44348,#44349,#44350,
#44351,#44352,#44353,#44354,#44355,#44356,#44357,#44358,#44359,#44360,#44361,
#44362,#44363,#44364,#44365,#44366,#44367,#44368,#44369,#44370,#44371,#44372,
#44373,#44374,#44375,#44376,#44377,#44378,#44379,#44380,#44381,#44382,#44383,
#44384,#44385,#44386,#44387,#44388,#44389,#44390,#44391,#44392,#44393,#44394,
#44395,#44396,#44397,#44398,#44399),.UNSPECIFIED.,.T.,.F.,(4,1,1,1,1,1,
1,1,1,1,1,1,1,1,1,1,1,1,1,1,1,1,1,1,1,1,1,1,1,1,1,1,1,1,1,1,1,1,1,1,1,1,
1,1,1,1,1,1,1,1,1,1,1,1,1,1,1,1,1,1,1,1,4),(0.,0.346838652723539,0.433548315904424,
0.455225731699645,0.476903147494867,0.498580563290088,0.520257979085309,
0.693677305447079,0.7153547212423,0.737032137037521,0.780386968627963,0.823741800218406,
0.867096631808848,0.953806294989733,0.997161126580175,1.04051595817062,
1.38735461089416,1.39096751352669,1.39458041615923,1.4018062214243,1.41625783195445,
1.42348363721953,1.4307094424846,1.44516105301475,1.50296749513534,1.56077393725593,
1.61858037937652,1.7341932636177,1.79199970573829,1.84980614785888,2.08103191634124,
2.13883835846183,2.19664480058242,2.25445124270301,2.31225768482359,2.54348345330595,
2.65909633754713,2.77470922178831,2.94812854815008,3.12154787451185,3.20825753769274,
3.29496720087362,3.38167686405451,3.42503169564495,3.43587040354256,3.44670911144017,
3.45754781933778,3.46838652723539,3.64180585359716,3.81522517995893,3.85858001154937,
3.90193484313982,3.9886445063207,4.07535416950159,4.11870900109203,4.16206383268247,
4.33548315904424,4.34632186694185,4.35716057483946,4.37883799063468,4.42219282222513,
4.50890248540601,4.85574113812955),.UNSPECIFIED.);
#1103=B_SPLINE_CURVE_WITH_KNOTS('',3,(#44400,#44401,#44402,#44403,#44404,
#44405,#44406,#44407,#44408,#44409,#44410,#44411,#44412,#44413,#44414,#44415,
#44416,#44417,#44418,#44419,#44420,#44421,#44422,#44423,#44424,#44425,#44426,
#44427,#44428,#44429,#44430,#44431,#44432,#44433,#44434,#44435,#44436,#44437,
#44438,#44439,#44440,#44441,#44442,#44443,#44444,#44445,#44446,#44447,#44448,
#44449,#44450,#44451,#44452,#44453,#44454,#44455,#44456,#44457,#44458,#44459,
#44460,#44461,#44462,#44463,#44464),.UNSPECIFIED.,.T.,.F.,(4,1,1,1,1,1,
1,1,1,1,1,1,1,1,1,1,1,1,1,1,1,1,1,1,1,1,1,1,1,1,1,1,1,1,1,1,1,1,1,1,1,1,
1,1,1,1,1,1,1,1,1,1,1,1,1,1,1,1,1,1,1,1,4),(-4.85574113812955,-4.50890248540601,
-4.42219282222513,-4.37883799063468,-4.35716057483946,-4.34632186694185,
-4.33548315904424,-4.16206383268247,-4.11870900109203,-4.07535416950159,
-3.9886445063207,-3.90193484313982,-3.85858001154937,-3.81522517995893,
-3.64180585359716,-3.46838652723539,-3.45754781933778,-3.44670911144017,
-3.43587040354256,-3.42503169564495,-3.38167686405451,-3.29496720087362,
-3.20825753769274,-3.12154787451185,-2.94812854815008,-2.77470922178831,
-2.65909633754713,-2.54348345330595,-2.31225768482359,-2.25445124270301,
-2.19664480058242,-2.13883835846183,-2.08103191634124,-1.84980614785888,
-1.79199970573829,-1.7341932636177,-1.61858037937652,-1.56077393725593,
-1.50296749513534,-1.44516105301475,-1.4307094424846,-1.42348363721953,
-1.41625783195445,-1.4018062214243,-1.39458041615923,-1.39096751352669,
-1.38735461089416,-1.04051595817062,-0.997161126580175,-0.953806294989733,
-0.867096631808848,-0.823741800218406,-0.780386968627963,-0.737032137037521,
-0.7153547212423,-0.693677305447079,-0.520257979085309,-0.498580563290088,
-0.476903147494867,-0.455225731699645,-0.433548315904424,-0.346838652723539,
0.),.UNSPECIFIED.);
#1104=B_SPLINE_CURVE_WITH_KNOTS('',3,(#44468,#44469,#44470,#44471,#44472,
#44473,#44474,#44475,#44476,#44477,#44478,#44479,#44480,#44481,#44482,#44483,
#44484,#44485,#44486,#44487),.UNSPECIFIED.,.F.,.F.,(4,1,1,1,1,2,2,1,1,1,
1,1,2,1,4),(1.16422336569995,1.62550842979414,2.08679349388834,2.31743602593544,
2.54807855798254,3.00936362207673,3.08125863299769,3.36971080227501,3.65816297155233,
3.73027601387166,3.802389056191,3.94661514082966,4.23506731010698,4.71432612693143,
4.89579080658336),.UNSPECIFIED.);
#1105=B_SPLINE_CURVE_WITH_KNOTS('',3,(#44488,#44489,#44490,#44491,#44492,
#44493,#44494),.UNSPECIFIED.,.F.,.F.,(4,1,1,1,4),(4.89579080658336,5.19358494375588,
5.67284376058034,5.91247316899256,6.15210257740479),.UNSPECIFIED.);
#1106=B_SPLINE_CURVE_WITH_KNOTS('',3,(#44502,#44503,#44504,#44505,#44506,
#44507,#44508,#44509,#44510,#44511,#44512,#44513,#44514,#44515,#44516,#44517,
#44518,#44519,#44520,#44521,#44522,#44523,#44524,#44525,#44526,#44527),
 .UNSPECIFIED.,.F.,.F.,(4,2,2,2,2,2,2,2,2,2,2,2,4),(2.26670802646318,2.55003859116132,
2.83336915585947,3.40003028525577,3.96672316909106,4.25006961100871,4.53341605292635,
4.816762494844,5.10010893676165,5.66680182059694,6.23346294999324,6.51679351469138,
6.80012407938953),.UNSPECIFIED.);
#1107=B_SPLINE_CURVE_WITH_KNOTS('',3,(#44532,#44533,#44534,#44535,#44536,
#44537,#44538,#44539,#44540,#44541,#44542,#44543,#44544,#44545),
 .UNSPECIFIED.,.F.,.F.,(4,2,2,2,2,2,4),(6.80012407938953,7.08345464408768,
7.36678520878583,7.93344633818212,8.50013922201742,8.78348566393506,9.06683210585271),
 .UNSPECIFIED.);
#1108=B_SPLINE_CURVE_WITH_KNOTS('',3,(#44546,#44547,#44548,#44549,#44550,
#44551,#44552,#44553,#44554,#44555,#44556,#44557,#44558,#44559),
 .UNSPECIFIED.,.F.,.F.,(4,2,2,2,2,2,4),(0.,0.283346441917647,0.566692883835293,
1.13338576767059,1.70004689706688,1.98337746176503,2.26670802646318),
 .UNSPECIFIED.);
#1109=B_SPLINE_CURVE_WITH_KNOTS('',3,(#44561,#44562,#44563,#44564,#44565,
#44566,#44567,#44568,#44569,#44570,#44571,#44572,#44573,#44574,#44575,#44576,
#44577,#44578,#44579,#44580,#44581,#44582,#44583,#44584,#44585,#44586,#44587,
#44588,#44589,#44590,#44591,#44592,#44593,#44594,#44595,#44596,#44597,#44598,
#44599,#44600,#44601,#44602,#44603,#44604,#44605,#44606,#44607,#44608,#44609,
#44610),.UNSPECIFIED.,.T.,.F.,(4,2,2,2,2,2,2,2,2,2,2,2,2,2,2,2,2,2,2,2,
2,2,2,2,4),(0.,0.283346441917647,0.566692883835293,1.13338576767059,1.70004689706688,
1.98337746176503,2.26670802646318,2.55003859116132,2.83336915585947,3.40003028525577,
3.96672316909106,4.25006961100871,4.53341605292635,4.816762494844,5.10010893676165,
5.66680182059694,6.23346294999323,6.51679351469138,6.80012407938953,7.08345464408768,
7.36678520878582,7.93344633818212,8.50013922201741,8.78348566393506,9.06683210585271),
 .UNSPECIFIED.);
#1110=B_SPLINE_CURVE_WITH_KNOTS('',3,(#44612,#44613,#44614,#44615,#44616,
#44617,#44618,#44619,#44620,#44621,#44622,#44623,#44624,#44625,#44626,#44627,
#44628,#44629,#44630,#44631,#44632,#44633,#44634,#44635,#44636,#44637,#44638,
#44639,#44640,#44641,#44642,#44643,#44644,#44645,#44646,#44647,#44648,#44649,
#44650,#44651,#44652,#44653,#44654,#44655,#44656,#44657,#44658,#44659,#44660,
#44661),.UNSPECIFIED.,.T.,.F.,(4,2,2,2,2,2,2,2,2,2,2,2,2,2,2,2,2,2,2,2,
2,2,2,2,4),(0.,0.283346441917646,0.566692883835292,1.13338576767058,1.70004689706688,
1.98337746176503,2.26670802646318,2.55003859116133,2.83336915585948,3.40003028525578,
3.96672316909107,4.25006961100872,4.53341605292636,4.81676249484401,5.10010893676166,
5.66680182059695,6.23346294999325,6.5167935146914,6.80012407938955,7.0834546440877,
7.36678520878585,7.93344633818214,8.50013922201744,8.78348566393508,9.06683210585273),
 .UNSPECIFIED.);
#1111=B_SPLINE_CURVE_WITH_KNOTS('',3,(#44663,#44664,#44665,#44666,#44667,
#44668,#44669,#44670,#44671,#44672,#44673,#44674,#44675,#44676,#44677,#44678,
#44679,#44680,#44681,#44682,#44683,#44684,#44685,#44686,#44687,#44688,#44689,
#44690,#44691,#44692,#44693,#44694,#44695,#44696,#44697,#44698,#44699,#44700,
#44701,#44702,#44703,#44704,#44705,#44706,#44707,#44708,#44709,#44710,#44711,
#44712),.UNSPECIFIED.,.T.,.F.,(4,2,2,2,2,2,2,2,2,2,2,2,2,2,2,2,2,2,2,2,
2,2,2,2,4),(0.,0.283346441917645,0.566692883835289,1.13338576767058,1.70004689706688,
1.98337746176503,2.26670802646318,2.55003859116133,2.83336915585948,3.40003028525578,
3.96672316909107,4.25006961100871,4.53341605292636,4.816762494844,5.10010893676165,
5.66680182059694,6.23346294999324,6.51679351469139,6.80012407938954,7.08345464408769,
7.36678520878584,7.93344633818214,8.50013922201743,8.78348566393507,9.06683210585271),
 .UNSPECIFIED.);
#1112=B_SPLINE_CURVE_WITH_KNOTS('',3,(#44714,#44715,#44716,#44717,#44718,
#44719,#44720,#44721,#44722,#44723,#44724,#44725,#44726,#44727,#44728,#44729,
#44730,#44731,#44732,#44733,#44734,#44735,#44736,#44737,#44738,#44739,#44740,
#44741,#44742,#44743,#44744,#44745,#44746,#44747,#44748,#44749,#44750,#44751,
#44752,#44753,#44754,#44755,#44756,#44757,#44758,#44759,#44760,#44761,#44762,
#44763),.UNSPECIFIED.,.T.,.F.,(4,2,2,2,2,2,2,2,2,2,2,2,2,2,2,2,2,2,2,2,
2,2,2,2,4),(0.,0.283346441917645,0.566692883835291,1.13338576767058,1.70004689706688,
1.98337746176503,2.26670802646318,2.55003859116133,2.83336915585948,3.40003028525578,
3.96672316909107,4.25006961100872,4.53341605292636,4.81676249484401,5.10010893676165,
5.66680182059694,6.23346294999324,6.51679351469139,6.80012407938954,7.08345464408769,
7.36678520878584,7.93344633818214,8.50013922201743,8.78348566393508,9.06683210585273),
 .UNSPECIFIED.);
#1113=B_SPLINE_CURVE_WITH_KNOTS('',3,(#44765,#44766,#44767,#44768,#44769,
#44770,#44771,#44772,#44773,#44774,#44775,#44776,#44777,#44778,#44779,#44780,
#44781,#44782,#44783,#44784,#44785,#44786,#44787,#44788,#44789,#44790,#44791,
#44792,#44793,#44794,#44795,#44796,#44797,#44798,#44799,#44800,#44801,#44802,
#44803,#44804,#44805,#44806,#44807,#44808,#44809,#44810,#44811,#44812,#44813,
#44814),.UNSPECIFIED.,.T.,.F.,(4,2,2,2,2,2,2,2,2,2,2,2,2,2,2,2,2,2,2,2,
2,2,2,2,4),(0.,0.283346441917644,0.566692883835287,1.13338576767057,1.70004689706687,
1.98337746176502,2.26670802646317,2.55003859116132,2.83336915585947,3.40003028525577,
3.96672316909106,4.2500696110087,4.53341605292635,4.81676249484399,5.10010893676164,
5.66680182059692,6.23346294999322,6.51679351469137,6.80012407938952,7.08345464408767,
7.36678520878582,7.93344633818212,8.50013922201741,8.78348566393505,9.0668321058527),
 .UNSPECIFIED.);
#1114=B_SPLINE_CURVE_WITH_KNOTS('',3,(#44910,#44911,#44912,#44913,#44914,
#44915,#44916,#44917,#44918,#44919),.UNSPECIFIED.,.F.,.F.,(4,1,1,1,1,2,
4),(-6.15210257740479,-5.91247316899256,-5.67284376058034,-5.19358494375588,
-4.71432612693143,-4.23506731010698,-4.12936945995859),.UNSPECIFIED.);
#1115=B_SPLINE_CURVE_WITH_KNOTS('',3,(#44921,#44922,#44923,#44924,#44925,
#44926,#44927,#44928,#44929),.UNSPECIFIED.,.F.,.F.,(4,1,1,1,1,1,4),(-4.12936945995859,
-3.94661514082966,-3.802389056191,-3.73027601387166,-3.65816297155233,-3.36971080227501,
-3.18695648314609),.UNSPECIFIED.);
#1116=B_SPLINE_CURVE_WITH_KNOTS('',3,(#44930,#44931,#44932,#44933,#44934,
#44935,#44936,#44937,#44938,#44939,#44940,#44941),.UNSPECIFIED.,.F.,.F.,
(4,2,2,1,1,1,1,4),(-3.18695648314609,-3.08125863299769,-3.00936362207673,
-2.54807855798254,-2.31743602593544,-2.08679349388834,-1.62550842979414,
-1.16422336569995),.UNSPECIFIED.);
#1117=B_SPLINE_CURVE_WITH_KNOTS('',3,(#44954,#44955,#44956,#44957,#44958,
#44959,#44960,#44961,#44962,#44963,#44964,#44965,#44966,#44967,#44968,#44969,
#44970,#44971,#44972,#44973,#44974,#44975,#44976,#44977,#44978,#44979),
 .UNSPECIFIED.,.F.,.F.,(4,2,2,2,2,2,2,2,2,2,2,2,4),(2.38843711110425,2.73991717768157,
3.18290676087182,3.79372965899082,4.41467175444456,4.65907472712817,4.82558871054652,
5.00595266090074,5.33402028952842,5.78028507040623,6.42716241421292,6.9078895490275,
7.2160083509484),.UNSPECIFIED.);
#1118=B_SPLINE_CURVE_WITH_KNOTS('',3,(#44983,#44984,#44985,#44986,#44987,
#44988,#44989,#44990,#44991,#44992,#44993,#44994,#44995,#44996,#44997,#44998,
#44999,#45000,#45001,#45002,#45003,#45004,#45005,#45006),.UNSPECIFIED.,
 .F.,.F.,(4,2,2,2,2,2,2,2,2,2,2,4),(2.22240766759392,2.51631391142046,2.86860433098781,
3.30769808976926,3.80274376109231,4.15490018438336,4.49463257862064,4.88220060274562,
5.47385284067091,6.01546654165425,6.42750720918413,6.5614735041056),
 .UNSPECIFIED.);
#1119=B_SPLINE_CURVE_WITH_KNOTS('',3,(#45010,#45011,#45012,#45013,#45014,
#45015,#45016,#45017,#45018,#45019,#45020,#45021,#45022,#45023,#45024,#45025,
#45026,#45027,#45028,#45029,#45030,#45031,#45032,#45033,#45034,#45035),
 .UNSPECIFIED.,.F.,.F.,(4,2,2,2,2,2,2,2,2,2,2,2,4),(2.38843711109743,2.73991717767369,
3.18290676086253,3.79372965898107,4.41467175443591,4.65907472712015,4.82558871053879,
5.00595266089327,5.33402028952175,5.78028507040088,6.42716241420991,6.90788954902662,
7.216008350949),.UNSPECIFIED.);
#1120=B_SPLINE_CURVE_WITH_KNOTS('',3,(#45039,#45040,#45041,#45042,#45043,
#45044,#45045,#45046,#45047,#45048,#45049,#45050,#45051,#45052,#45053,#45054,
#45055,#45056,#45057,#45058,#45059,#45060,#45061,#45062,#45063,#45064),
 .UNSPECIFIED.,.F.,.F.,(4,2,2,2,2,2,2,2,2,2,2,2,4),(2.3884371111015,2.73991717767853,
3.18290676086844,3.79372965898921,4.41467175444667,4.65907472713178,4.82558871055129,
5.00595266090689,5.33402028953752,5.7802850704188,6.4271624142303,6.90788954904922,
7.21600835097295),.UNSPECIFIED.);
#1121=B_SPLINE_CURVE_WITH_KNOTS('',3,(#45068,#45069,#45070,#45071,#45072,
#45073,#45074,#45075,#45076,#45077,#45078,#45079,#45080,#45081,#45082,#45083,
#45084,#45085,#45086,#45087,#45088,#45089,#45090,#45091),.UNSPECIFIED.,
 .F.,.F.,(4,2,2,2,2,2,2,2,2,2,2,4),(2.2224076675936,2.51631391142003,2.8686043309871,
3.30769808976771,3.80274376108999,4.15490018438039,4.49463257861656,4.88220060273995,
5.47385284066319,6.01546654164533,6.42750720917386,6.56147350409479),
 .UNSPECIFIED.);
#1122=B_SPLINE_CURVE_WITH_KNOTS('',3,(#45095,#45096,#45097,#45098,#45099,
#45100,#45101,#45102,#45103,#45104,#45105,#45106,#45107,#45108,#45109,#45110,
#45111,#45112,#45113,#45114,#45115,#45116,#45117,#45118,#45119,#45120),
 .UNSPECIFIED.,.F.,.F.,(4,2,2,2,2,2,2,2,2,2,2,2,4),(2.38843711111166,2.73991717769056,
3.18290676088307,3.79372965900683,4.4146717544666,4.65907472715359,4.82558871057392,
5.00595266093029,5.33402028956311,5.78028507044741,6.42716241426385,6.90788954908701,
7.21600835101346),.UNSPECIFIED.);
#1123=B_SPLINE_CURVE_WITH_KNOTS('',3,(#45123,#45124,#45125,#45126,#45127,
#45128,#45129,#45130,#45131,#45132,#45133,#45134,#45135,#45136,#45137,#45138),
 .UNSPECIFIED.,.F.,.F.,(4,2,2,2,2,2,2,4),(0.,0.163315076677852,0.428209466619433,
0.780925001042535,1.38907330894996,1.92592908231006,2.3460116526462,2.38843711111166),
 .UNSPECIFIED.);
#1124=B_SPLINE_CURVE_WITH_KNOTS('',3,(#45139,#45140,#45141,#45142,#45143,
#45144,#45145,#45146,#45147,#45148,#45149,#45150,#45151,#45152,#45153,#45154),
 .UNSPECIFIED.,.F.,.F.,(4,2,2,2,2,2,2,4),(7.21600835101346,7.31138807064545,
7.71016155437429,8.19219414711906,8.90541863857944,9.32049440063031,9.51422700130749,
9.59086664090117),.UNSPECIFIED.);
#1125=B_SPLINE_CURVE_WITH_KNOTS('',3,(#45156,#45157,#45158,#45159,#45160,
#45161,#45162,#45163,#45164,#45165,#45166,#45167,#45168,#45169),
 .UNSPECIFIED.,.F.,.F.,(4,2,2,2,2,2,4),(0.,0.314217231275812,0.709389217563233,
1.32114854838333,1.80769659482899,2.17854969785705,2.2224076675936),
 .UNSPECIFIED.);
#1126=B_SPLINE_CURVE_WITH_KNOTS('',3,(#45170,#45171,#45172,#45173,#45174,
#45175,#45176,#45177,#45178,#45179,#45180,#45181,#45182,#45183),
 .UNSPECIFIED.,.F.,.F.,(4,2,2,2,2,2,4),(6.56147350409479,6.79183498105132,
7.15166374851714,7.58660248971605,8.17287181265779,8.55036069386147,8.66642098576321),
 .UNSPECIFIED.);
#1127=B_SPLINE_CURVE_WITH_KNOTS('',3,(#45185,#45186,#45187,#45188,#45189,
#45190,#45191,#45192,#45193,#45194,#45195,#45196,#45197,#45198,#45199,#45200),
 .UNSPECIFIED.,.F.,.F.,(4,2,2,2,2,2,2,4),(0.,0.163315076677636,0.428209466618054,
0.780925001039408,1.38907330894433,1.92592908230217,2.34601165263628,2.3884371111015),
 .UNSPECIFIED.);
#1128=B_SPLINE_CURVE_WITH_KNOTS('',3,(#45201,#45202,#45203,#45204,#45205,
#45206,#45207,#45208,#45209,#45210,#45211,#45212,#45213,#45214,#45215,#45216),
 .UNSPECIFIED.,.F.,.F.,(4,2,2,2,2,2,2,4),(7.21600835097295,7.311388070604,
7.71016155432903,8.19219414706878,8.90541863852133,9.32049440056781,9.51422700124278,
9.59086664083621),.UNSPECIFIED.);
#1129=B_SPLINE_CURVE_WITH_KNOTS('',3,(#45218,#45219,#45220,#45221,#45222,
#45223,#45224,#45225,#45226,#45227,#45228,#45229,#45230,#45231,#45232,#45233),
 .UNSPECIFIED.,.F.,.F.,(4,2,2,2,2,2,2,4),(0.,0.163315076677541,0.428209466617523,
0.780925001038301,1.38907330894207,1.92592908229898,2.34601165263229,2.38843711109743),
 .UNSPECIFIED.);
#1130=B_SPLINE_CURVE_WITH_KNOTS('',3,(#45234,#45235,#45236,#45237,#45238,
#45239,#45240,#45241,#45242,#45243,#45244,#45245,#45246,#45247,#45248,#45249),
 .UNSPECIFIED.,.F.,.F.,(4,2,2,2,2,2,2,4),(7.216008350949,7.31138807057958,
7.71016155430275,8.19219414704005,8.90541863848882,9.32049440053308,9.51422700120671,
9.59086664079997),.UNSPECIFIED.);
#1131=B_SPLINE_CURVE_WITH_KNOTS('',3,(#45251,#45252,#45253,#45254,#45255,
#45256,#45257,#45258,#45259,#45260,#45261,#45262,#45263,#45264),
 .UNSPECIFIED.,.F.,.F.,(4,2,2,2,2,2,4),(0.,0.314217231275878,0.709389217563644,
1.3211485483838,1.80769659482918,2.1785496978573,2.22240766759392),
 .UNSPECIFIED.);
#1132=B_SPLINE_CURVE_WITH_KNOTS('',3,(#45265,#45266,#45267,#45268,#45269,
#45270,#45271,#45272,#45273,#45274,#45275,#45276,#45277,#45278),
 .UNSPECIFIED.,.F.,.F.,(4,2,2,2,2,2,4),(6.5614735041056,6.79183498106296,
7.15166374853013,7.58660248973094,8.17287181267555,8.5503606938791,8.66642098578064),
 .UNSPECIFIED.);
#1133=B_SPLINE_CURVE_WITH_KNOTS('',3,(#45280,#45281,#45282,#45283,#45284,
#45285,#45286,#45287,#45288,#45289,#45290,#45291,#45292,#45293,#45294,#45295),
 .UNSPECIFIED.,.F.,.F.,(4,2,2,2,2,2,2,4),(0.,0.163315076677694,0.428209466618468,
0.780925001040192,1.38907330894576,1.92592908230429,2.34601165263891,2.38843711110425),
 .UNSPECIFIED.);
#1134=B_SPLINE_CURVE_WITH_KNOTS('',3,(#45296,#45297,#45298,#45299,#45300,
#45301,#45302,#45303,#45304,#45305,#45306,#45307,#45308,#45309,#45310,#45311),
 .UNSPECIFIED.,.F.,.F.,(4,2,2,2,2,2,2,4),(7.2160083509484,7.31138807057855,
7.71016155429981,8.1921941470349,8.90541863848042,9.3204944005228,9.5142270011958,
9.59086664078899),.UNSPECIFIED.);
#1135=B_SPLINE_CURVE_WITH_KNOTS('',3,(#45348,#45349,#45350,#45351,#45352,
#45353,#45354,#45355,#45356,#45357,#45358,#45359,#45360,#45361,#45362,#45363),
 .UNSPECIFIED.,.F.,.F.,(4,3,3,3,3,4),(-4.09274904019422,-3.96157812047045,
-3.46638085541164,-2.97118359035283,-2.47598632529403,-2.06954507459125),
 .UNSPECIFIED.);
#1136=B_SPLINE_CURVE_WITH_KNOTS('',3,(#45366,#45367,#45368,#45369,#45370,
#45371,#45372,#45373,#45374,#45375),.UNSPECIFIED.,.F.,.F.,(4,3,3,4),(0.,
0.495197265058804,0.990394530117612,1.11838868798682),.UNSPECIFIED.);
#1137=B_SPLINE_CURVE_WITH_KNOTS('',3,(#45380,#45381,#45382,#45383,#45384,
#45385,#45386,#45387,#45388,#45389,#45390,#45391,#45392,#45393,#45394,#45395,
#45396,#45397,#45398,#45399,#45400,#45401,#45402,#45403,#45404,#45405,#45406,
#45407,#45408,#45409,#45410,#45411,#45412,#45413,#45414,#45415,#45416,#45417,
#45418,#45419),.UNSPECIFIED.,.F.,.F.,(4,3,3,3,3,3,3,3,3,3,3,3,3,4),(-10.3759343473738,
-9.90394530117612,-9.40874803611731,-8.91355077105851,-8.4183535059997,
-7.9231562409409,-7.42795897588209,-6.93276171082328,-6.43756444576448,
-5.94236718070567,-5.44716991564687,-4.95197265058806,-4.45677538552925,
-4.09274904019422),.UNSPECIFIED.);
#1138=B_SPLINE_CURVE_WITH_KNOTS('',3,(#45420,#45421,#45422,#45423,#45424,
#45425,#45426,#45427,#45428,#45429,#45430,#45431,#45432,#45433,#45434,#45435,
#45436,#45437,#45438,#45439,#45440,#45441,#45442,#45443,#45444,#45445,#45446,
#45447,#45448,#45449,#45450,#45451,#45452,#45453,#45454,#45455,#45456,#45457,
#45458,#45459),.UNSPECIFIED.,.F.,.F.,(4,3,3,3,3,3,3,3,3,3,3,3,3,4),(1.11838868798682,
1.48559179517642,1.98078906023522,2.47598632529403,2.97118359035284,3.46638085541164,
3.96157812047045,4.45677538552925,4.95197265058806,5.44716991564687,5.94236718070567,
6.43756444576448,6.93276171082328,7.4015739951664),.UNSPECIFIED.);
#1139=B_SPLINE_CURVE_WITH_KNOTS('',3,(#45464,#45465,#45466,#45467,#45468,
#45469,#45470,#45471,#45472,#45473,#45474,#45475,#45476,#45477,#45478,#45479,
#45480,#45481,#45482,#45483,#45484,#45485,#45486,#45487,#45488,#45489,#45490,
#45491,#45492,#45493,#45494,#45495,#45496,#45497,#45498,#45499,#45500,#45501,
#45502,#45503,#45504,#45505,#45506),.UNSPECIFIED.,.F.,.F.,(4,3,3,3,3,3,
3,3,3,3,3,3,3,3,4),(-16.6591196545534,-16.3415097469406,-15.8463124818818,
-15.351115216823,-14.8559179517642,-14.3607206867054,-13.8655234216466,
-13.3703261565878,-12.875128891529,-12.3799316264701,-11.8847343614113,
-11.3895370963525,-10.8943398312937,-10.3991425662349,-10.3759343473738),
 .UNSPECIFIED.);
#1140=B_SPLINE_CURVE_WITH_KNOTS('',3,(#45507,#45508,#45509,#45510,#45511,
#45512,#45513,#45514,#45515,#45516,#45517,#45518,#45519,#45520,#45521,#45522,
#45523,#45524,#45525,#45526,#45527,#45528,#45529,#45530,#45531,#45532,#45533,
#45534,#45535,#45536,#45537,#45538,#45539,#45540,#45541,#45542,#45543,#45544,
#45545,#45546,#45547,#45548,#45549),.UNSPECIFIED.,.F.,.F.,(4,3,3,3,3,3,
3,3,3,3,3,3,3,3,4),(7.4015739951664,7.42795897588209,7.92315624094089,8.4183535059997,
8.9135507710585,9.40874803611731,9.90394530117612,10.3991425662349,10.8943398312937,
11.3895370963525,11.8847343614113,12.3799316264701,12.875128891529,13.3703261565878,
13.684759302346),.UNSPECIFIED.);
#1141=B_SPLINE_CURVE_WITH_KNOTS('',3,(#45554,#45555,#45556,#45557,#45558,
#45559,#45560,#45561,#45562,#45563,#45564,#45565,#45566,#45567,#45568,#45569,
#45570,#45571,#45572,#45573,#45574,#45575,#45576,#45577,#45578,#45579,#45580,
#45581,#45582,#45583,#45584,#45585,#45586,#45587,#45588,#45589,#45590,#45591,
#45592,#45593,#45594,#45595,#45596),.UNSPECIFIED.,.F.,.F.,(4,3,3,3,3,3,
3,3,3,3,3,3,3,3,4),(-22.942304961733,-22.7790741927051,-22.2838769276463,
-21.7886796625875,-21.2934823975287,-20.7982851324699,-20.303087867411,
-19.8078906023522,-19.3126933372934,-18.8174960722346,-18.3222988071758,
-17.827101542117,-17.3319042770582,-16.8367070119994,-16.6591196545534),
 .UNSPECIFIED.);
#1142=B_SPLINE_CURVE_WITH_KNOTS('',3,(#45597,#45598,#45599,#45600,#45601,
#45602,#45603,#45604,#45605,#45606,#45607,#45608,#45609,#45610,#45611,#45612,
#45613,#45614,#45615,#45616,#45617,#45618,#45619,#45620,#45621,#45622,#45623,
#45624,#45625,#45626,#45627,#45628,#45629,#45630,#45631,#45632,#45633,#45634,
#45635,#45636,#45637,#45638,#45639),.UNSPECIFIED.,.F.,.F.,(4,3,3,3,3,3,
3,3,3,3,3,3,3,3,4),(13.684759302346,13.8655234216466,14.3607206867054,14.8559179517642,
15.351115216823,15.8463124818818,16.3415097469406,16.8367070119994,17.3319042770582,
17.827101542117,18.3222988071758,18.8174960722346,19.3126933372934,19.8078906023522,
19.9679446095256),.UNSPECIFIED.);
#1143=B_SPLINE_CURVE_WITH_KNOTS('',3,(#45644,#45645,#45646,#45647,#45648,
#45649,#45650,#45651,#45652,#45653,#45654,#45655,#45656,#45657,#45658,#45659,
#45660,#45661,#45662,#45663,#45664,#45665,#45666,#45667,#45668,#45669,#45670,
#45671,#45672,#45673,#45674,#45675,#45676,#45677,#45678,#45679,#45680,#45681,
#45682,#45683,#45684,#45685,#45686),.UNSPECIFIED.,.F.,.F.,(4,3,3,3,3,3,
3,3,3,3,3,3,3,3,4),(-29.2254902689126,-29.2166386384695,-28.7214413734107,
-28.2262441083519,-27.7310468432931,-27.2358495782343,-26.7406523131755,
-26.2454550481167,-25.7502577830579,-25.2550605179991,-24.7598632529403,
-24.2646659878815,-23.7694687228227,-23.2742714577639,-22.942304961733),
 .UNSPECIFIED.);
#1144=B_SPLINE_CURVE_WITH_KNOTS('',3,(#45687,#45688,#45689,#45690,#45691,
#45692,#45693,#45694,#45695,#45696,#45697,#45698,#45699,#45700,#45701,#45702,
#45703,#45704,#45705,#45706,#45707,#45708,#45709,#45710,#45711,#45712,#45713,
#45714,#45715,#45716,#45717,#45718,#45719,#45720,#45721,#45722,#45723,#45724,
#45725,#45726,#45727,#45728,#45729),.UNSPECIFIED.,.F.,.F.,(4,3,3,3,3,3,
3,3,3,3,3,3,3,3,4),(19.9679446095256,20.303087867411,20.7982851324698,21.2934823975286,
21.7886796625875,22.2838769276463,22.7790741927051,23.2742714577639,23.7694687228227,
24.2646659878815,24.7598632529403,25.2550605179991,25.7502577830579,26.2454550481167,
26.2511299167052),.UNSPECIFIED.);
#1145=B_SPLINE_CURVE_WITH_KNOTS('',3,(#45734,#45735,#45736,#45737,#45738,
#45739,#45740,#45741,#45742,#45743,#45744,#45745,#45746,#45747,#45748,#45749,
#45750,#45751,#45752,#45753,#45754,#45755,#45756,#45757,#45758,#45759,#45760,
#45761,#45762,#45763,#45764,#45765,#45766,#45767,#45768,#45769,#45770,#45771,
#45772,#45773),.UNSPECIFIED.,.F.,.F.,(4,3,3,3,3,3,3,3,3,3,3,3,3,4),(-35.5086755760922,
-35.1590058191752,-34.6638085541164,-34.1686112890576,-33.6734140239988,
-33.17821675894,-32.6830194938812,-32.1878222288224,-31.6926249637636,-31.1974276987048,
-30.702230433646,-30.2070331685872,-29.7118359035283,-29.2254902689126),
 .UNSPECIFIED.);
#1146=B_SPLINE_CURVE_WITH_KNOTS('',3,(#45774,#45775,#45776,#45777,#45778,
#45779,#45780,#45781,#45782,#45783,#45784,#45785,#45786,#45787,#45788,#45789,
#45790,#45791,#45792,#45793,#45794,#45795,#45796,#45797,#45798,#45799,#45800,
#45801,#45802,#45803,#45804,#45805,#45806,#45807,#45808,#45809,#45810,#45811,
#45812,#45813),.UNSPECIFIED.,.F.,.F.,(4,3,3,3,3,3,3,3,3,3,3,3,3,4),(26.2511299167052,
26.7406523131755,27.2358495782343,27.7310468432931,28.2262441083519,28.7214413734107,
29.2166386384696,29.7118359035284,30.2070331685872,30.702230433646,31.1974276987048,
31.6926249637636,32.1878222288224,32.5343152238847),.UNSPECIFIED.);
#1147=B_SPLINE_CURVE_WITH_KNOTS('',3,(#45818,#45819,#45820,#45821,#45822,
#45823,#45824,#45825,#45826,#45827,#45828,#45829,#45830,#45831,#45832,#45833,
#45834,#45835,#45836,#45837,#45838,#45839,#45840,#45841,#45842,#45843,#45844,
#45845,#45846,#45847,#45848,#45849,#45850,#45851,#45852,#45853,#45854,#45855,
#45856,#45857,#45858,#45859,#45860),.UNSPECIFIED.,.F.,.F.,(4,3,3,3,3,3,
3,3,3,3,3,3,3,3,4),(-41.7918608832718,-41.5965702649397,-41.1013729998809,
-40.6061757348221,-40.1109784697633,-39.6157812047045,-39.1205839396457,
-38.6253866745869,-38.1301894095281,-37.6349921444693,-37.1397948794104,
-36.6445976143516,-36.1494003492928,-35.654203084234,-35.5086755760922),
 .UNSPECIFIED.);
#1148=B_SPLINE_CURVE_WITH_KNOTS('',3,(#45861,#45862,#45863,#45864,#45865,
#45866,#45867,#45868,#45869,#45870,#45871,#45872,#45873,#45874,#45875,#45876,
#45877,#45878,#45879,#45880,#45881,#45882,#45883,#45884,#45885,#45886,#45887,
#45888,#45889,#45890,#45891,#45892,#45893,#45894,#45895,#45896,#45897,#45898,
#45899,#45900,#45901,#45902,#45903),.UNSPECIFIED.,.F.,.F.,(4,3,3,3,3,3,
3,3,3,3,3,3,3,3,4),(32.5343152238847,32.6830194938812,33.17821675894,33.6734140239988,
34.1686112890576,34.6638085541164,35.1590058191752,35.654203084234,36.1494003492928,
36.6445976143516,37.1397948794104,37.6349921444692,38.130189409528,38.6253866745868,
38.8175005310643),.UNSPECIFIED.);
#1149=B_SPLINE_CURVE_WITH_KNOTS('',3,(#45909,#45910,#45911,#45912,#45913),
 .UNSPECIFIED.,.F.,.F.,(4,1,4),(53.4070751110265,53.7069817577532,54.113423008456),
 .UNSPECIFIED.);
#1150=B_SPLINE_CURVE_WITH_KNOTS('',3,(#45919,#45920,#45921,#45922,#45923,
#45924,#45925,#45926,#45927,#45928,#45929,#45930,#45931,#45932,#45933,#45934,
#45935),.UNSPECIFIED.,.F.,.F.,(4,1,1,1,1,1,1,1,1,1,1,1,1,1,4),(47.1238898038469,
47.2694173119888,47.7646145770476,48.2598118421064,48.7550091071652,49.250206372224,
49.7454036372828,50.2406009023416,50.7357981674004,51.2309954324592,51.726192697518,
52.2213899625768,52.7165872276356,53.2117844926944,53.4070751110265),
 .UNSPECIFIED.);
#1151=B_SPLINE_CURVE_WITH_KNOTS('',3,(#45938,#45939,#45940,#45941,#45942,
#45943,#45944,#45945,#45946,#45947,#45948,#45949,#45950,#45951,#45952),
 .UNSPECIFIED.,.F.,.F.,(4,1,1,1,1,1,1,1,1,1,1,1,4),(47.1238898038469,47.4269732124282,
47.922170477487,48.4173677425458,48.9125650076046,49.4077622726634,49.9029595377222,
50.398156802781,50.8933540678398,51.3885513328986,51.8837485979574,52.3789458630163,
52.8741431280751),.UNSPECIFIED.);
#1152=B_SPLINE_CURVE_WITH_KNOTS('',3,(#45957,#45958,#45959,#45960,#45961,
#45962,#45963,#45964,#45965,#45966,#45967,#45968,#45969,#45970,#45971,#45972),
 .UNSPECIFIED.,.F.,.F.,(4,1,1,1,1,1,1,1,1,1,1,1,1,4),(40.8407044966673,
41.3270501312831,41.8222473963419,42.3174446614007,42.8126419264595,43.3078391915183,
43.8030364565771,44.2982337216359,44.7934309866947,45.2886282517535,45.7838255168123,
46.2790227818711,46.7742200469299,47.1238898038469),.UNSPECIFIED.);
#1153=B_SPLINE_CURVE_WITH_KNOTS('',3,(#45973,#45974,#45975,#45976,#45977,
#45978,#45979,#45980,#45981,#45982,#45983,#45984,#45985,#45986,#45987,#45988,
#45989),.UNSPECIFIED.,.F.,.F.,(4,1,1,1,1,1,1,1,1,1,1,1,1,1,4),(40.8407044966673,
40.9894087666637,41.4846060317225,41.9798032967813,42.4750005618401,42.9701978268989,
43.4653950919578,43.9605923570166,44.4557896220754,44.9509868871342,45.446184152193,
45.9413814172518,46.4365786823106,46.9317759473694,47.1238898038469),
 .UNSPECIFIED.);
#1154=B_SPLINE_CURVE_WITH_KNOTS('',3,(#45994,#45995,#45996,#45997,#45998,
#45999,#46000,#46001,#46002,#46003,#46004,#46005,#46006,#46007,#46008,#46009,
#46010),.UNSPECIFIED.,.F.,.F.,(4,1,1,1,1,1,1,1,1,1,1,1,1,1,4),(34.5575191894877,
34.8894856855186,35.3846829505774,35.8798802156362,36.375077480695,36.8702747457538,
37.3654720108126,37.8606692758714,38.3558665409303,38.8510638059891,39.3462610710479,
39.8414583361067,40.3366556011655,40.8318528662243,40.8407044966673),
 .UNSPECIFIED.);
#1155=B_SPLINE_CURVE_WITH_KNOTS('',3,(#46011,#46012,#46013,#46014,#46015,
#46016,#46017,#46018,#46019,#46020,#46021,#46022,#46023,#46024,#46025,#46026),
 .UNSPECIFIED.,.F.,.F.,(4,1,1,1,1,1,1,1,1,1,1,1,1,4),(34.5575191894877,
35.0470415859581,35.5422388510169,36.0374361160757,36.5326333811345,37.0278306461933,
37.5230279112521,38.0182251763109,38.5134224413697,39.0086197064285,39.5038169714873,
39.9990142365461,40.4942115016049,40.8407044966673),.UNSPECIFIED.);
#1156=B_SPLINE_CURVE_WITH_KNOTS('',3,(#46031,#46032,#46033,#46034,#46035,
#46036,#46037,#46038,#46039,#46040,#46041,#46042,#46043,#46044,#46045,#46046,
#46047),.UNSPECIFIED.,.F.,.F.,(4,1,1,1,1,1,1,1,1,1,1,1,1,1,4),(28.2743338823081,
28.4519212397541,28.9471185048129,29.4423157698717,29.9375130349305,30.4327102999894,
30.9279075650482,31.423104830107,31.9183020951658,32.4134993602246,32.9086966252834,
33.4038938903422,33.899091155401,34.3942884204598,34.5575191894877),
 .UNSPECIFIED.);
#1157=B_SPLINE_CURVE_WITH_KNOTS('',3,(#46048,#46049,#46050,#46051,#46052,
#46053,#46054,#46055,#46056,#46057,#46058,#46059,#46060,#46061,#46062,#46063,
#46064),.UNSPECIFIED.,.F.,.F.,(4,1,1,1,1,1,1,1,1,1,1,1,1,1,4),(28.2743338823081,
28.6094771401936,29.1046744052524,29.5998716703112,30.09506893537,30.5902662004288,
31.0854634654876,31.5806607305464,32.0758579956052,32.571055260664,33.0662525257228,
33.5614497907816,34.0566470558404,34.5518443208992,34.5575191894877),
 .UNSPECIFIED.);
#1158=B_SPLINE_CURVE_WITH_KNOTS('',3,(#46069,#46070,#46071,#46072,#46073,
#46074,#46075,#46076,#46077,#46078,#46079,#46080,#46081,#46082,#46083,#46084,
#46085),.UNSPECIFIED.,.F.,.F.,(4,1,1,1,1,1,1,1,1,1,1,1,1,1,4),(21.9911485751285,
22.0143567939897,22.5095540590485,23.0047513241073,23.4999485891661,23.9951458542249,
24.4903431192837,24.9855403843425,25.4807376494013,25.9759349144601,26.4711321795189,
26.9663294445777,27.4615267096365,27.9567239746953,28.2743338823081),
 .UNSPECIFIED.);
#1159=B_SPLINE_CURVE_WITH_KNOTS('',3,(#46086,#46087,#46088,#46089,#46090,
#46091,#46092,#46093,#46094,#46095,#46096,#46097,#46098,#46099,#46100,#46101,
#46102),.UNSPECIFIED.,.F.,.F.,(4,1,1,1,1,1,1,1,1,1,1,1,1,1,4),(21.9911485751285,
22.1719126944291,22.6671099594879,23.1623072245467,23.6575044896055,24.1527017546643,
24.6478990197231,25.1430962847819,25.6382935498407,26.1334908148995,26.6286880799584,
27.1238853450172,27.619082610076,28.1142798751348,28.2743338823081),
 .UNSPECIFIED.);
#1160=B_SPLINE_CURVE_WITH_KNOTS('',3,(#46107,#46108,#46109,#46110,#46111,
#46112,#46113,#46114,#46115,#46116,#46117,#46118,#46119,#46120,#46121,#46122),
 .UNSPECIFIED.,.F.,.F.,(4,1,1,1,1,1,1,1,1,1,1,1,1,4),(15.7079632679489,
16.071989613284,16.5671868783428,17.0623841434016,17.5575814084604,18.0527786735192,
18.547975938578,19.0431732036368,19.5383704686956,20.0335677337544,20.5287649988132,
21.023962263872,21.5191595289308,21.9911485751285),.UNSPECIFIED.);
#1161=B_SPLINE_CURVE_WITH_KNOTS('',3,(#46123,#46124,#46125,#46126,#46127,
#46128,#46129,#46130,#46131,#46132,#46133,#46134,#46135,#46136,#46137,#46138,
#46139),.UNSPECIFIED.,.F.,.F.,(4,1,1,1,1,1,1,1,1,1,1,1,1,1,4),(15.7079632679489,
15.7343482486646,16.2295455137234,16.7247427787822,17.219940043841,17.7151373088998,
18.2103345739587,18.7055318390175,19.2007291040763,19.6959263691351,20.1911236341939,
20.6863208992527,21.1815181643115,21.6767154293703,21.9911485751285),
 .UNSPECIFIED.);
#1162=B_SPLINE_CURVE_WITH_KNOTS('',3,(#46142,#46143,#46144,#46145,#46146,
#46147,#46148,#46149,#46150,#46151,#46152,#46153,#46154,#46155,#46156,#46157,
#46158,#46159,#46160,#46161,#46162,#46163,#46164,#46165,#46166,#46167,#46168,
#46169,#46170,#46171,#46172,#46173,#46174,#46175,#46176,#46177,#46178,#46179,
#46180,#46181,#46182,#46183,#46184,#46185,#46186,#46187,#46188,#46189,#46190,
#46191,#46192,#46193,#46194,#46195,#46196,#46197,#46198,#46199,#46200,#46201,
#46202,#46203,#46204,#46205,#46206,#46207,#46208,#46209,#46210,#46211,#46212,
#46213,#46214,#46215,#46216,#46217),.UNSPECIFIED.,.F.,.F.,(4,3,3,3,3,3,
3,3,3,3,3,3,3,3,3,3,3,3,3,3,3,3,3,3,3,4),(-1.91386167632963,-1.83787666420088,
-1.72938395031299,-1.69638705507551,-1.66779038111967,-1.54802690914779,
-1.46245266964146,-1.43449001143917,-1.40390580864931,-1.28249728337303,
-1.19581509431375,-1.13105418444924,-1.10714354766822,-0.982416794980164,
-0.952469860823683,-0.835450486557249,-0.774018515207216,-0.748138511354911,
-0.616265437556429,-0.484392363757948,-0.423843318288204,-0.388665671195739,
-0.36353285337654,-0.234458855956312,-0.104218518256837,0.),
 .UNSPECIFIED.);
#1163=B_SPLINE_CURVE_WITH_KNOTS('',3,(#46222,#46223,#46224,#46225,#46226,
#46227,#46228,#46229,#46230,#46231,#46232,#46233,#46234,#46235,#46236,#46237,
#46238,#46239,#46240,#46241,#46242,#46243,#46244,#46245,#46246,#46247,#46248,
#46249,#46250,#46251,#46252,#46253,#46254,#46255,#46256,#46257,#46258,#46259,
#46260,#46261,#46262,#46263,#46264,#46265,#46266,#46267,#46268,#46269,#46270,
#46271,#46272,#46273,#46274,#46275,#46276,#46277,#46278,#46279,#46280,#46281,
#46282,#46283,#46284,#46285,#46286,#46287,#46288,#46289,#46290,#46291,#46292,
#46293,#46294,#46295,#46296,#46297,#46298,#46299,#46300),.UNSPECIFIED.,
 .F.,.F.,(4,3,3,3,3,3,3,3,3,3,3,3,3,3,3,3,3,3,3,3,3,3,3,3,3,3,4),(-1.90760546354383,
-1.81998897247625,-1.70019436157863,-1.65920884954384,-1.62916942004787,
-1.50064906159473,-1.41275923540419,-1.38440638426796,-1.34081052888579,
-1.21430756052813,-1.088913657374,-1.03595243864197,-1.0113746483739,-0.888053044233851,
-0.877312664850233,-0.765554368577898,-0.706871867177446,-0.68052011894822,
-0.656720355914381,-0.536198813546398,-0.430279479760896,-0.375078455320756,
-0.336309197496637,-0.311758984916726,-0.19334490167706,-0.0770967652264511,
0.),.UNSPECIFIED.);
#1164=B_SPLINE_CURVE_WITH_KNOTS('',3,(#46673,#46674,#46675,#46676,#46677,
#46678,#46679,#46680,#46681,#46682,#46683,#46684,#46685,#46686,#46687,#46688,
#46689,#46690,#46691,#46692,#46693,#46694,#46695,#46696,#46697),
 .UNSPECIFIED.,.F.,.F.,(4,3,3,3,3,3,3,3,4),(38.8175005310643,39.1205839396457,
39.6157812047045,40.1109784697633,40.6061757348221,41.1013729998809,41.5965702649397,
42.0917675299985,42.4982087807013),.UNSPECIFIED.);
#1165=B_SPLINE_CURVE_WITH_KNOTS('',3,(#46699,#46700,#46701,#46702,#46703,
#46704,#46705,#46706,#46707,#46708,#46709,#46710,#46711,#46712,#46713,#46714,
#46715,#46716,#46717,#46718,#46719,#46720,#46721,#46722,#46723,#46724,#46725,
#46726,#46727,#46728,#46729,#46730,#46731,#46732,#46733,#46734,#46735,#46736,
#46737,#46738,#46739,#46740,#46741,#46742,#46743,#46744,#46745,#46746,#46747,
#46748,#46749,#46750,#46751,#46752,#46753,#46754,#46755,#46756,#46757,#46758,
#46759,#46760,#46761,#46762,#46763,#46764,#46765,#46766,#46767,#46768,#46769,
#46770,#46771,#46772,#46773,#46774),.UNSPECIFIED.,.F.,.F.,(4,3,3,3,3,3,
3,3,3,3,3,3,3,3,3,3,3,3,3,3,3,3,3,3,3,4),(-1.91386167632967,-1.83787666420092,
-1.72938395031302,-1.69638705987941,-1.66779038861988,-1.54802692650689,
-1.46245267849424,-1.4344900129501,-1.40390580864934,-1.28249727261198,
-1.19581511826659,-1.13105421602521,-1.10714359156754,-0.982416836462222,
-0.952469860823725,-0.835450486557284,-0.774018545328602,-0.748138537086926,
-0.616265450422444,-0.484392363757962,-0.423843318288217,-0.388665667195217,
-0.363532849728275,-0.234458958092049,-0.104218565736301,0.),
 .UNSPECIFIED.);
#1166=B_SPLINE_CURVE_WITH_KNOTS('',3,(#46775,#46776,#46777,#46778,#46779,
#46780,#46781,#46782,#46783,#46784,#46785,#46786,#46787,#46788),
 .UNSPECIFIED.,.F.,.F.,(4,1,1,1,1,1,1,1,1,1,1,4),(10.3759343473738,10.7823755980766,
11.2775728631354,11.7727701281942,12.267967393253,12.7631646583118,13.2583619233706,
13.7535591884294,14.2487564534882,14.743953718547,15.2391509836058,15.7079632679489),
 .UNSPECIFIED.);
#1167=B_SPLINE_CURVE_WITH_KNOTS('',3,(#46794,#46795,#46796,#46797,#46798,
#46799,#46800,#46801,#46802,#46803,#46804,#46805,#46806,#46807,#46808,#46809,
#46810,#46811,#46812,#46813,#46814,#46815,#46816,#46817,#46818,#46819,#46820,
#46821,#46822,#46823,#46824,#46825,#46826,#46827,#46828,#46829,#46830,#46831,
#46832,#46833,#46834,#46835,#46836,#46837,#46838,#46839,#46840,#46841,#46842,
#46843,#46844,#46845,#46846,#46847,#46848,#46849,#46850,#46851,#46852,#46853,
#46854,#46855,#46856,#46857,#46858,#46859,#46860,#46861,#46862,#46863,#46864,
#46865,#46866,#46867,#46868,#46869,#46870,#46871,#46872),.UNSPECIFIED.,
 .F.,.F.,(4,3,3,3,3,3,3,3,3,3,3,3,3,3,3,3,3,3,3,3,3,3,3,3,3,3,4),(-1.90760546354381,
-1.81998897247621,-1.7001943615786,-1.65920884369368,-1.62916941167379,
-1.50064905344499,-1.412759230544,-1.38440638462706,-1.34081052888577,-1.21430757107678,
-1.08891372531773,-1.03595283676006,-1.01137473308098,-0.888053166855498,
-0.877312664850218,-0.765554368577884,-0.706871875281147,-0.680520127214094,
-0.656720353469998,-0.536198723300522,-0.430279479760884,-0.375078429667684,
-0.33630914297151,-0.311758975914638,-0.193344896342556,-0.0770969253539728,
0.),.UNSPECIFIED.);
#1168=B_SPLINE_CURVE_WITH_KNOTS('',3,(#46875,#46876,#46877,#46878,#46879,
#46880,#46881,#46882,#46883,#46884,#46885,#46886),.UNSPECIFIED.,.F.,.F.,
(4,1,1,1,1,1,1,1,1,4),(11.6152142277547,12.1104114928135,12.6056087578723,
13.1008060229311,13.59600328799,14.0912005530488,14.5863978181076,15.0815950831664,
15.5767923482252,15.7079632679489),.UNSPECIFIED.);
#1169=B_SPLINE_CURVE_WITH_KNOTS('',3,(#47259,#47260,#47261,#47262,#47263,
#47264,#47265,#47266,#47267,#47268,#47269,#47270,#47271,#47272,#47273,#47274,
#47275,#47276,#47277),.UNSPECIFIED.,.F.,.F.,(4,3,3,3,3,3,4),(-44.5677538552925,
-44.0725565902337,-43.5773593251749,-43.0821620601161,-42.5869647950573,
-42.0917675299985,-41.7918608832718),.UNSPECIFIED.);
#1170=B_SPLINE_CURVE_WITH_KNOTS('',3,(#47594,#47595,#47596,#47597,#47598,
#47599,#47600,#47601,#47602,#47603,#47604,#47605,#47606,#47607,#47608,#47609),
 .UNSPECIFIED.,.F.,.F.,(4,3,3,3,3,4),(-4.09293042013069,-3.98542709836851,
-3.48724871107244,-2.98907032377638,-2.49089193648032,-2.07498647268394),
 .UNSPECIFIED.);
#1171=B_SPLINE_CURVE_WITH_KNOTS('',3,(#47612,#47613,#47614,#47615,#47616,
#47617,#47618,#47619,#47620,#47621),.UNSPECIFIED.,.F.,.F.,(4,3,3,4),(0.,
0.498178387296066,0.996356774592132,1.1236487061432),.UNSPECIFIED.);
#1172=B_SPLINE_CURVE_WITH_KNOTS('',3,(#47626,#47627,#47628,#47629,#47630,
#47631,#47632,#47633,#47634,#47635,#47636,#47637,#47638,#47639,#47640,#47641,
#47642,#47643,#47644,#47645,#47646,#47647,#47648,#47649,#47650,#47651,#47652,
#47653,#47654,#47655,#47656,#47657,#47658,#47659,#47660,#47661,#47662,#47663,
#47664,#47665),.UNSPECIFIED.,.F.,.F.,(4,3,3,3,3,3,3,3,3,3,3,3,3,4),(-10.3761157273103,
-9.96356774592127,-9.4653893586252,-8.96721097132914,-8.46903258403308,
-7.97085419673701,-7.47267580944095,-6.97449742214489,-6.47631903484883,
-5.97814064755276,-5.4799622602567,-4.98178387296063,-4.48360548566457,
-4.09293042013069),.UNSPECIFIED.);
#1173=B_SPLINE_CURVE_WITH_KNOTS('',3,(#47666,#47667,#47668,#47669,#47670,
#47671,#47672,#47673,#47674,#47675,#47676,#47677,#47678,#47679,#47680,#47681,
#47682,#47683,#47684,#47685,#47686,#47687,#47688,#47689,#47690,#47691,#47692,
#47693,#47694,#47695,#47696,#47697,#47698,#47699,#47700,#47701,#47702,#47703,
#47704,#47705),.UNSPECIFIED.,.F.,.F.,(4,3,3,3,3,3,3,3,3,3,3,3,3,4),(1.1236487061432,
1.4945351618882,1.99271354918426,2.49089193648032,2.98907032377638,3.48724871107245,
3.98542709836851,4.48360548566457,4.98178387296063,5.4799622602567,5.97814064755276,
6.47631903484882,6.97449742214488,7.40683401332279),.UNSPECIFIED.);
#1174=B_SPLINE_CURVE_WITH_KNOTS('',3,(#47710,#47711,#47712,#47713,#47714,
#47715,#47716,#47717,#47718,#47719,#47720,#47721,#47722,#47723,#47724,#47725,
#47726,#47727,#47728,#47729,#47730,#47731,#47732,#47733,#47734,#47735,#47736,
#47737,#47738,#47739,#47740,#47741,#47742,#47743,#47744,#47745,#47746,#47747,
#47748,#47749,#47750,#47751,#47752),.UNSPECIFIED.,.F.,.F.,(4,3,3,3,3,3,
3,3,3,3,3,3,3,3,4),(-16.6593010344898,-16.4398867807701,-15.941708393474,
-15.443530006178,-14.9453516188819,-14.4471732315858,-13.9489948442898,
-13.4508164569937,-12.9526380696976,-12.4544596824016,-11.9562812951055,
-11.4581029078095,-10.9599245205134,-10.4617461332173,-10.3761157273103),
 .UNSPECIFIED.);
#1175=B_SPLINE_CURVE_WITH_KNOTS('',3,(#47753,#47754,#47755,#47756,#47757,
#47758,#47759,#47760,#47761,#47762,#47763,#47764,#47765,#47766,#47767,#47768,
#47769,#47770,#47771,#47772,#47773,#47774,#47775,#47776,#47777,#47778,#47779,
#47780,#47781,#47782,#47783,#47784,#47785,#47786,#47787,#47788,#47789,#47790,
#47791,#47792,#47793,#47794,#47795),.UNSPECIFIED.,.F.,.F.,(4,3,3,3,3,3,
3,3,3,3,3,3,3,3,4),(7.40683401332279,7.47267580944095,7.97085419673701,
8.46903258403307,8.96721097132914,9.4653893586252,9.96356774592126,10.4617461332173,
10.9599245205134,11.4581029078095,11.9562812951055,12.4544596824016,12.9526380696976,
13.4508164569937,13.6900193205024),.UNSPECIFIED.);
#1176=B_SPLINE_CURVE_WITH_KNOTS('',3,(#47800,#47801,#47802,#47803,#47804,
#47805,#47806,#47807,#47808,#47809,#47810,#47811,#47812,#47813,#47814,#47815,
#47816,#47817,#47818,#47819,#47820,#47821,#47822,#47823,#47824,#47825,#47826,
#47827,#47828,#47829,#47830,#47831,#47832,#47833,#47834,#47835,#47836,#47837,
#47838,#47839,#47840,#47841,#47842),.UNSPECIFIED.,.F.,.F.,(4,3,3,3,3,3,
3,3,3,3,3,3,3,3,4),(-22.9424863416694,-22.9162058156189,-22.4180274283228,
-21.9198490410268,-21.4216706537307,-20.9234922664347,-20.4253138791386,
-19.9271354918425,-19.4289571045465,-18.9307787172504,-18.4326003299543,
-17.9344219426583,-17.4362435553622,-16.9380651680661,-16.6593010344898),
 .UNSPECIFIED.);
#1177=B_SPLINE_CURVE_WITH_KNOTS('',3,(#47843,#47844,#47845,#47846,#47847,
#47848,#47849,#47850,#47851,#47852,#47853,#47854,#47855,#47856,#47857,#47858,
#47859,#47860,#47861,#47862,#47863,#47864,#47865,#47866,#47867,#47868,#47869,
#47870,#47871,#47872,#47873,#47874,#47875,#47876,#47877,#47878,#47879,#47880,
#47881,#47882,#47883,#47884,#47885),.UNSPECIFIED.,.F.,.F.,(4,3,3,3,3,3,
3,3,3,3,3,3,3,3,4),(13.6900193205024,13.9489948442898,14.4471732315858,
14.9453516188819,15.443530006178,15.941708393474,16.4398867807701,16.9380651680661,
17.4362435553622,17.9344219426583,18.4326003299543,18.9307787172504,19.4289571045465,
19.9271354918425,19.9732046276819),.UNSPECIFIED.);
#1178=B_SPLINE_CURVE_WITH_KNOTS('',3,(#47890,#47891,#47892,#47893,#47894,
#47895,#47896,#47897,#47898,#47899,#47900,#47901,#47902,#47903,#47904,#47905,
#47906,#47907,#47908,#47909,#47910,#47911,#47912,#47913,#47914,#47915,#47916,
#47917,#47918,#47919,#47920,#47921,#47922,#47923,#47924,#47925,#47926,#47927,
#47928,#47929),.UNSPECIFIED.,.F.,.F.,(4,3,3,3,3,3,3,3,3,3,3,3,3,4),(-29.225671648849,
-28.8943464631717,-28.3961680758756,-27.8979896885795,-27.3998113012835,
-26.9016329139874,-26.4034545266914,-25.9052761393953,-25.4070977520992,
-24.9089193648032,-24.4107409775071,-23.912562590211,-23.414384202915,-22.9424863416694),
 .UNSPECIFIED.);
#1179=B_SPLINE_CURVE_WITH_KNOTS('',3,(#47930,#47931,#47932,#47933,#47934,
#47935,#47936,#47937,#47938,#47939,#47940,#47941,#47942,#47943,#47944,#47945,
#47946,#47947,#47948,#47949,#47950,#47951,#47952,#47953,#47954,#47955,#47956,
#47957,#47958,#47959,#47960,#47961,#47962,#47963,#47964,#47965,#47966,#47967,
#47968,#47969),.UNSPECIFIED.,.F.,.F.,(4,3,3,3,3,3,3,3,3,3,3,3,3,4),(19.9732046276819,
20.4253138791386,20.9234922664346,21.4216706537307,21.9198490410268,22.4180274283228,
22.9162058156189,23.414384202915,23.912562590211,24.4107409775071,24.9089193648032,
25.4070977520992,25.9052761393953,26.2563899348615),.UNSPECIFIED.);
#1180=B_SPLINE_CURVE_WITH_KNOTS('',3,(#47974,#47975,#47976,#47977,#47978,
#47979,#47980,#47981,#47982,#47983,#47984,#47985,#47986,#47987,#47988,#47989,
#47990,#47991,#47992,#47993,#47994,#47995,#47996,#47997,#47998,#47999,#48000,
#48001,#48002,#48003,#48004,#48005,#48006,#48007,#48008,#48009,#48010,#48011,
#48012,#48013,#48014,#48015,#48016),.UNSPECIFIED.,.F.,.F.,(4,3,3,3,3,3,
3,3,3,3,3,3,3,3,4),(-35.5088569560286,-35.3706654980205,-34.8724871107244,
-34.3743087234284,-33.8761303361323,-33.3779519488362,-32.8797735615402,
-32.3815951742441,-31.883416786948,-31.385238399652,-30.8870600123559,-30.3888816250599,
-29.8907032377638,-29.3925248504677,-29.225671648849),.UNSPECIFIED.);
#1181=B_SPLINE_CURVE_WITH_KNOTS('',3,(#48017,#48018,#48019,#48020,#48021,
#48022,#48023,#48024,#48025,#48026,#48027,#48028,#48029,#48030,#48031,#48032,
#48033,#48034,#48035,#48036,#48037,#48038,#48039,#48040,#48041,#48042,#48043,
#48044,#48045,#48046,#48047,#48048,#48049,#48050,#48051,#48052,#48053,#48054,
#48055,#48056,#48057,#48058,#48059),.UNSPECIFIED.,.F.,.F.,(4,3,3,3,3,3,
3,3,3,3,3,3,3,3,4),(26.2563899348615,26.4034545266914,26.9016329139874,
27.3998113012835,27.8979896885795,28.3961680758756,28.8943464631717,29.3925248504677,
29.8907032377638,30.3888816250599,30.8870600123559,31.385238399652,31.883416786948,
32.3815951742441,32.5395752420411),.UNSPECIFIED.);
#1182=B_SPLINE_CURVE_WITH_KNOTS('',3,(#48064,#48065,#48066,#48067,#48068,
#48069,#48070,#48071,#48072,#48073,#48074,#48075,#48076,#48077,#48078,#48079,
#48080,#48081,#48082,#48083,#48084,#48085,#48086,#48087,#48088,#48089,#48090,
#48091,#48092,#48093,#48094,#48095,#48096,#48097,#48098,#48099,#48100,#48101,
#48102,#48103),.UNSPECIFIED.,.F.,.F.,(4,3,3,3,3,3,3,3,3,3,3,3,3,4),(-41.7920422632082,
-41.3488061455732,-40.8506277582772,-40.3524493709811,-39.8542709836851,
-39.356092596389,-38.8579142090929,-38.3597358217969,-37.8615574345008,
-37.3633790472047,-36.8652006599087,-36.3670222726126,-35.8688438853166,
-35.5088569560286),.UNSPECIFIED.);
#1183=B_SPLINE_CURVE_WITH_KNOTS('',3,(#48104,#48105,#48106,#48107,#48108,
#48109,#48110,#48111,#48112,#48113,#48114,#48115,#48116,#48117,#48118,#48119,
#48120,#48121,#48122,#48123,#48124,#48125,#48126,#48127,#48128,#48129,#48130,
#48131,#48132,#48133,#48134,#48135,#48136,#48137,#48138,#48139,#48140,#48141,
#48142,#48143),.UNSPECIFIED.,.F.,.F.,(4,3,3,3,3,3,3,3,3,3,3,3,3,4),(32.5395752420411,
32.8797735615402,33.3779519488362,33.8761303361323,34.3743087234284,34.8724871107244,
35.3706654980205,35.8688438853165,36.3670222726126,36.8652006599087,37.3633790472047,
37.8615574345008,38.3597358217969,38.8227605492207),.UNSPECIFIED.);
#1184=B_SPLINE_CURVE_WITH_KNOTS('',3,(#48148,#48149,#48150,#48151,#48152,
#48153,#48154,#48155,#48156,#48157,#48158,#48159,#48160,#48161,#48162,#48163,
#48164,#48165,#48166,#48167,#48168,#48169,#48170,#48171,#48172,#48173,#48174,
#48175,#48176,#48177,#48178,#48179,#48180,#48181,#48182,#48183,#48184,#48185,
#48186,#48187,#48188,#48189,#48190),.UNSPECIFIED.,.F.,.F.,(4,3,3,3,3,3,
3,3,3,3,3,3,3,3,4),(-48.0752275703878,-47.8251251804221,-47.326946793126,
-46.8287684058299,-46.3305900185339,-45.8324116312378,-45.3342332439418,
-44.8360548566457,-44.3378764693496,-43.8396980820536,-43.3415196947575,
-42.8433413074614,-42.3451629201654,-41.8469845328693,-41.7920422632082),
 .UNSPECIFIED.);
#1185=B_SPLINE_CURVE_WITH_KNOTS('',3,(#48191,#48192,#48193,#48194,#48195,
#48196,#48197,#48198,#48199,#48200,#48201,#48202,#48203,#48204,#48205,#48206,
#48207,#48208,#48209,#48210,#48211,#48212,#48213,#48214,#48215,#48216,#48217,
#48218,#48219,#48220,#48221,#48222,#48223,#48224,#48225,#48226,#48227,#48228,
#48229,#48230,#48231,#48232,#48233),.UNSPECIFIED.,.F.,.F.,(4,3,3,3,3,3,
3,3,3,3,3,3,3,3,4),(38.8227605492207,38.8579142090929,39.356092596389,39.8542709836851,
40.3524493709811,40.8506277582772,41.3488061455732,41.8469845328693,42.3451629201654,
42.8433413074614,43.3415196947575,43.8396980820536,44.3378764693496,44.8360548566457,
45.1059458564003),.UNSPECIFIED.);
#1186=B_SPLINE_CURVE_WITH_KNOTS('',3,(#48238,#48239,#48240,#48241,#48242,
#48243,#48244,#48245,#48246,#48247,#48248,#48249,#48250,#48251,#48252,#48253,
#48254,#48255,#48256,#48257,#48258,#48259,#48260,#48261,#48262,#48263,#48264,
#48265,#48266,#48267,#48268,#48269,#48270,#48271,#48272,#48273,#48274,#48275,
#48276,#48277,#48278,#48279,#48280),.UNSPECIFIED.,.F.,.F.,(4,3,3,3,3,3,
3,3,3,3,3,3,3,3,4),(-54.3584128775674,-54.3014442152709,-53.8032658279748,
-53.3050874406788,-52.8069090533827,-52.3087306660866,-51.8105522787906,
-51.3123738914945,-50.8141955041984,-50.3160171169024,-49.8178387296063,
-49.3196603423103,-48.8214819550142,-48.3233035677181,-48.0752275703878),
 .UNSPECIFIED.);
#1187=B_SPLINE_CURVE_WITH_KNOTS('',3,(#48281,#48282,#48283,#48284,#48285,
#48286,#48287,#48288,#48289,#48290,#48291,#48292,#48293,#48294,#48295,#48296,
#48297,#48298,#48299,#48300,#48301,#48302,#48303,#48304,#48305,#48306,#48307,
#48308,#48309,#48310,#48311,#48312,#48313,#48314,#48315,#48316,#48317,#48318,
#48319,#48320,#48321,#48322,#48323),.UNSPECIFIED.,.F.,.F.,(4,3,3,3,3,3,
3,3,3,3,3,3,3,3,4),(45.1059458564003,45.3342332439418,45.8324116312378,
46.3305900185339,46.8287684058299,47.326946793126,47.8251251804221,48.3233035677181,
48.8214819550142,49.3196603423102,49.8178387296063,50.3160171169024,50.8141955041984,
51.3123738914945,51.3891311635799),.UNSPECIFIED.);
#1188=B_SPLINE_CURVE_WITH_KNOTS('',3,(#48328,#48329,#48330,#48331,#48332,
#48333,#48334,#48335,#48336,#48337,#48338,#48339,#48340,#48341,#48342,#48343,
#48344,#48345,#48346,#48347,#48348,#48349,#48350,#48351,#48352,#48353,#48354,
#48355,#48356,#48357,#48358,#48359,#48360,#48361,#48362,#48363,#48364,#48365,
#48366,#48367),.UNSPECIFIED.,.F.,.F.,(4,3,3,3,3,3,3,3,3,3,3,3,3,4),(-60.641598184747,
-60.2795848628236,-59.7814064755276,-59.2832280882315,-58.7850497009355,
-58.2868713136394,-57.7886929263433,-57.2905145390473,-56.7923361517512,
-56.2941577644551,-55.7959793771591,-55.297800989863,-54.7996226025669,
-54.3584128775674),.UNSPECIFIED.);
#1189=B_SPLINE_CURVE_WITH_KNOTS('',3,(#48368,#48369,#48370,#48371,#48372,
#48373,#48374,#48375,#48376,#48377,#48378,#48379,#48380,#48381,#48382,#48383,
#48384,#48385,#48386,#48387,#48388,#48389,#48390,#48391,#48392,#48393,#48394,
#48395,#48396,#48397,#48398,#48399,#48400,#48401,#48402,#48403,#48404,#48405,
#48406,#48407),.UNSPECIFIED.,.F.,.F.,(4,3,3,3,3,3,3,3,3,3,3,3,3,4),(51.3891311635799,
51.8105522787905,52.3087306660866,52.8069090533827,53.3050874406787,53.8032658279748,
54.3014442152709,54.7996226025669,55.297800989863,55.7959793771591,56.2941577644551,
56.7923361517512,57.2905145390473,57.6723164707595),.UNSPECIFIED.);
#1190=B_SPLINE_CURVE_WITH_KNOTS('',3,(#48412,#48413,#48414,#48415,#48416,
#48417,#48418,#48419,#48420,#48421,#48422,#48423,#48424,#48425,#48426,#48427,
#48428,#48429,#48430,#48431,#48432,#48433,#48434,#48435,#48436,#48437,#48438,
#48439,#48440,#48441,#48442,#48443,#48444,#48445,#48446,#48447,#48448,#48449,
#48450,#48451,#48452,#48453,#48454),.UNSPECIFIED.,.F.,.F.,(4,3,3,3,3,3,
3,3,3,3,3,3,3,3,4),(-66.9247834919266,-66.7559038976725,-66.2577255103764,
-65.7595471230803,-65.2613687357843,-64.7631903484882,-64.2650119611921,
-63.7668335738961,-63.2686551866,-62.770476799304,-62.2722984120079,-61.7741200247118,
-61.2759416374158,-60.7777632501197,-60.641598184747),.UNSPECIFIED.);
#1191=B_SPLINE_CURVE_WITH_KNOTS('',3,(#48455,#48456,#48457,#48458,#48459,
#48460,#48461,#48462,#48463,#48464,#48465,#48466,#48467,#48468,#48469,#48470,
#48471,#48472,#48473,#48474,#48475,#48476,#48477,#48478,#48479,#48480,#48481,
#48482,#48483,#48484,#48485,#48486,#48487,#48488,#48489,#48490,#48491,#48492,
#48493,#48494,#48495,#48496,#48497),.UNSPECIFIED.,.F.,.F.,(4,3,3,3,3,3,
3,3,3,3,3,3,3,3,4),(57.6723164707595,57.7886929263433,58.2868713136394,
58.7850497009355,59.2832280882315,59.7814064755276,60.2795848628236,60.7777632501197,
61.2759416374158,61.7741200247118,62.2722984120079,62.770476799304,63.2686551866,
63.7668335738961,63.9555017779391),.UNSPECIFIED.);
#1192=B_SPLINE_CURVE_WITH_KNOTS('',3,(#48502,#48503,#48504,#48505,#48506,
#48507,#48508,#48509,#48510,#48511,#48512,#48513,#48514,#48515,#48516,#48517,
#48518,#48519,#48520,#48521,#48522,#48523,#48524,#48525,#48526,#48527,#48528,
#48529,#48530,#48531,#48532,#48533,#48534,#48535,#48536,#48537,#48538,#48539,
#48540,#48541),.UNSPECIFIED.,.F.,.F.,(4,3,3,3,3,3,3,3,3,3,3,3,3,4),(-73.2079687991062,
-72.7340445452252,-72.2358661579292,-71.7376877706331,-71.239509383337,
-70.741330996041,-70.2431526087449,-69.7449742214488,-69.2467958341528,
-68.7486174468567,-68.2504390595606,-67.7522606722646,-67.2540822849685,
-66.9247834919266),.UNSPECIFIED.);
#1193=B_SPLINE_CURVE_WITH_KNOTS('',3,(#48542,#48543,#48544,#48545,#48546,
#48547,#48548,#48549,#48550,#48551,#48552,#48553,#48554,#48555,#48556,#48557,
#48558,#48559,#48560,#48561,#48562,#48563,#48564,#48565,#48566,#48567,#48568,
#48569,#48570,#48571,#48572,#48573,#48574,#48575,#48576,#48577,#48578,#48579,
#48580,#48581),.UNSPECIFIED.,.F.,.F.,(4,3,3,3,3,3,3,3,3,3,3,3,3,4),(63.9555017779391,
64.2650119611922,64.7631903484882,65.2613687357843,65.7595471230804,66.2577255103764,
66.7559038976725,67.2540822849685,67.7522606722646,68.2504390595607,68.7486174468567,
69.2467958341528,69.7449742214488,70.2386870851187),.UNSPECIFIED.);
#1194=B_SPLINE_CURVE_WITH_KNOTS('',3,(#48586,#48587,#48588,#48589,#48590,
#48591,#48592,#48593,#48594,#48595,#48596,#48597,#48598,#48599,#48600,#48601,
#48602,#48603,#48604,#48605,#48606,#48607,#48608,#48609,#48610,#48611,#48612,
#48613,#48614,#48615,#48616,#48617,#48618,#48619,#48620,#48621,#48622,#48623,
#48624,#48625,#48626,#48627,#48628),.UNSPECIFIED.,.F.,.F.,(4,3,3,3,3,3,
3,3,3,3,3,3,3,3,4),(-79.4911541062858,-79.2103635800741,-78.712185192778,
-78.2140068054819,-77.7158284181859,-77.2176500308898,-76.7194716435937,
-76.2212932562977,-75.7231148690016,-75.2249364817055,-74.7267580944095,
-74.2285797071134,-73.7304013198173,-73.2322229325213,-73.2079687991062),
 .UNSPECIFIED.);
#1195=B_SPLINE_CURVE_WITH_KNOTS('',3,(#48629,#48630,#48631,#48632,#48633,
#48634,#48635,#48636,#48637,#48638,#48639,#48640,#48641,#48642,#48643,#48644,
#48645,#48646,#48647,#48648,#48649,#48650,#48651,#48652,#48653,#48654,#48655,
#48656,#48657,#48658,#48659,#48660,#48661,#48662,#48663,#48664,#48665,#48666,
#48667,#48668,#48669,#48670,#48671),.UNSPECIFIED.,.F.,.F.,(4,3,3,3,3,3,
3,3,3,3,3,3,3,3,4),(70.2386870851187,70.2431526087449,70.741330996041,71.239509383337,
71.7376877706331,72.2358661579292,72.7340445452252,73.2322229325213,73.7304013198174,
74.2285797071134,74.7267580944095,75.2249364817056,75.7231148690016,76.2212932562977,
76.5218723922983),.UNSPECIFIED.);
#1196=B_SPLINE_CURVE_WITH_KNOTS('',3,(#48676,#48677,#48678,#48679,#48680,
#48681,#48682,#48683,#48684,#48685,#48686,#48687,#48688,#48689,#48690,#48691,
#48692,#48693,#48694,#48695,#48696,#48697,#48698,#48699,#48700,#48701,#48702,
#48703,#48704,#48705,#48706,#48707,#48708,#48709,#48710,#48711,#48712,#48713,
#48714,#48715,#48716,#48717,#48718),.UNSPECIFIED.,.F.,.F.,(4,3,3,3,3,3,
3,3,3,3,3,3,3,3,4),(-85.7743394134654,-85.6866826149229,-85.1885042276268,
-84.6903258403307,-84.1921474530347,-83.6939690657386,-83.1957906784425,
-82.6976122911465,-82.1994339038504,-81.7012555165544,-81.2030771292583,
-80.7048987419623,-80.2067203546662,-79.7085419673701,-79.4911541062858),
 .UNSPECIFIED.);
#1197=B_SPLINE_CURVE_WITH_KNOTS('',3,(#48719,#48720,#48721,#48722,#48723,
#48724,#48725,#48726,#48727,#48728,#48729,#48730,#48731,#48732,#48733,#48734,
#48735,#48736,#48737,#48738,#48739,#48740,#48741,#48742,#48743,#48744,#48745,
#48746,#48747,#48748,#48749,#48750,#48751,#48752,#48753,#48754,#48755,#48756,
#48757,#48758,#48759,#48760,#48761),.UNSPECIFIED.,.F.,.F.,(4,3,3,3,3,3,
3,3,3,3,3,3,3,3,4),(76.5218723922983,76.7194716435937,77.2176500308898,
77.7158284181859,78.2140068054819,78.712185192778,79.210363580074,79.7085419673701,
80.2067203546662,80.7048987419622,81.2030771292583,81.7012555165544,82.1994339038504,
82.6976122911465,82.8050576994779),.UNSPECIFIED.);
#1198=B_SPLINE_CURVE_WITH_KNOTS('',3,(#48766,#48767,#48768,#48769,#48770,
#48771,#48772,#48773,#48774,#48775,#48776,#48777,#48778,#48779,#48780,#48781,
#48782,#48783,#48784,#48785,#48786,#48787,#48788,#48789,#48790,#48791,#48792,
#48793,#48794,#48795,#48796,#48797,#48798,#48799,#48800,#48801,#48802,#48803,
#48804,#48805),.UNSPECIFIED.,.F.,.F.,(4,3,3,3,3,3,3,3,3,3,3,3,3,4),(-92.0575247206449,
-91.6648232624756,-91.1666448751796,-90.6684664878835,-90.1702881005874,
-89.6721097132914,-89.1739313259953,-88.6757529386992,-88.1775745514032,
-87.6793961641071,-87.1812177768111,-86.683039389515,-86.1848610022189,
-85.7743394134654),.UNSPECIFIED.);
#1199=B_SPLINE_CURVE_WITH_KNOTS('',3,(#48806,#48807,#48808,#48809,#48810,
#48811,#48812,#48813,#48814,#48815,#48816,#48817,#48818,#48819,#48820,#48821,
#48822,#48823,#48824,#48825,#48826,#48827,#48828,#48829,#48830,#48831,#48832,
#48833,#48834,#48835,#48836,#48837,#48838,#48839,#48840,#48841,#48842,#48843,
#48844,#48845),.UNSPECIFIED.,.F.,.F.,(4,3,3,3,3,3,3,3,3,3,3,3,3,4),(82.8050576994779,
83.1957906784425,83.6939690657386,84.1921474530347,84.6903258403308,85.1885042276268,
85.6866826149229,86.1848610022189,86.683039389515,87.1812177768111,87.6793961641071,
88.1775745514032,88.6757529386992,89.0882430066575),.UNSPECIFIED.);
#1200=B_SPLINE_CURVE_WITH_KNOTS('',3,(#48850,#48851,#48852,#48853,#48854,
#48855,#48856,#48857,#48858,#48859,#48860,#48861,#48862,#48863,#48864,#48865,
#48866,#48867,#48868,#48869,#48870,#48871,#48872,#48873,#48874,#48875,#48876,
#48877,#48878,#48879,#48880,#48881,#48882,#48883,#48884,#48885,#48886,#48887,
#48888,#48889,#48890,#48891,#48892),.UNSPECIFIED.,.F.,.F.,(4,3,3,3,3,3,
3,3,3,3,3,3,3,3,4),(-98.3407100278245,-98.1411422973244,-97.6429639100284,
-97.1447855227323,-96.6466071354363,-96.1484287481402,-95.6502503608441,
-95.1520719735481,-94.653893586252,-94.1557151989559,-93.6575368116599,
-93.1593584243638,-92.6611800370678,-92.1630016497717,-92.0575247206449),
 .UNSPECIFIED.);
#1201=B_SPLINE_CURVE_WITH_KNOTS('',3,(#48893,#48894,#48895,#48896,#48897,
#48898,#48899,#48900,#48901,#48902,#48903,#48904,#48905,#48906,#48907,#48908,
#48909,#48910,#48911,#48912,#48913,#48914,#48915,#48916,#48917,#48918,#48919,
#48920,#48921,#48922,#48923,#48924,#48925,#48926,#48927,#48928,#48929,#48930,
#48931,#48932,#48933,#48934,#48935),.UNSPECIFIED.,.F.,.F.,(4,3,3,3,3,3,
3,3,3,3,3,3,3,3,4),(89.0882430066575,89.1739313259953,89.6721097132914,
90.1702881005874,90.6684664878835,91.1666448751796,91.6648232624756,92.1630016497717,
92.6611800370678,93.1593584243638,93.6575368116599,94.1557151989559,94.653893586252,
95.1520719735481,95.371428313837),.UNSPECIFIED.);
#1202=B_SPLINE_CURVE_WITH_KNOTS('',3,(#48940,#48941,#48942,#48943,#48944,
#48945,#48946,#48947,#48948,#48949,#48950,#48951,#48952,#48953,#48954,#48955,
#48956,#48957,#48958,#48959,#48960,#48961,#48962,#48963,#48964,#48965,#48966,
#48967,#48968,#48969,#48970,#48971,#48972,#48973,#48974,#48975,#48976,#48977,
#48978,#48979,#48980,#48981,#48982),.UNSPECIFIED.,.F.,.F.,(4,3,3,3,3,3,
3,3,3,3,3,3,3,3,4),(-104.623895335004,-104.617461332173,-104.119282944877,
-103.621104557581,-103.122926170285,-102.624747782989,-102.126569395693,
-101.628391008397,-101.130212621101,-100.632034233805,-100.133855846509,
-99.6356774592126,-99.1374990719166,-98.6393206846205,-98.3407100278245),
 .UNSPECIFIED.);
#1203=B_SPLINE_CURVE_WITH_KNOTS('',3,(#48983,#48984,#48985,#48986,#48987,
#48988,#48989,#48990,#48991,#48992,#48993,#48994,#48995,#48996,#48997,#48998,
#48999,#49000,#49001,#49002,#49003,#49004,#49005,#49006,#49007,#49008,#49009,
#49010,#49011,#49012,#49013,#49014,#49015,#49016,#49017,#49018,#49019,#49020,
#49021,#49022,#49023,#49024,#49025),.UNSPECIFIED.,.F.,.F.,(4,3,3,3,3,3,
3,3,3,3,3,3,3,3,4),(95.371428313837,95.6502503608441,96.1484287481402,96.6466071354362,
97.1447855227323,97.6429639100284,98.1411422973244,98.6393206846205,99.1374990719166,
99.6356774592126,100.133855846509,100.632034233805,101.130212621101,101.628391008397,
101.654613621017),.UNSPECIFIED.);
#1204=B_SPLINE_CURVE_WITH_KNOTS('',3,(#49030,#49031,#49032,#49033,#49034,
#49035,#49036,#49037,#49038,#49039,#49040,#49041,#49042,#49043,#49044,#49045,
#49046,#49047,#49048,#49049,#49050,#49051,#49052,#49053,#49054,#49055,#49056,
#49057,#49058,#49059,#49060,#49061,#49062,#49063,#49064,#49065,#49066,#49067,
#49068,#49069),.UNSPECIFIED.,.F.,.F.,(4,3,3,3,3,3,3,3,3,3,3,3,3,4),(-110.907080642184,
-110.595601979726,-110.09742359243,-109.599245205134,-109.101066817838,
-108.602888430542,-108.104710043246,-107.60653165595,-107.108353268654,
-106.610174881358,-106.111996494061,-105.613818106765,-105.115639719469,
-104.623895335004),.UNSPECIFIED.);
#1205=B_SPLINE_CURVE_WITH_KNOTS('',3,(#49070,#49071,#49072,#49073,#49074,
#49075,#49076,#49077,#49078,#49079,#49080,#49081,#49082,#49083,#49084,#49085,
#49086,#49087,#49088,#49089,#49090,#49091,#49092,#49093,#49094,#49095,#49096,
#49097,#49098,#49099,#49100,#49101,#49102,#49103,#49104,#49105,#49106,#49107,
#49108,#49109),.UNSPECIFIED.,.F.,.F.,(4,3,3,3,3,3,3,3,3,3,3,3,3,4),(101.654613621017,
102.126569395693,102.624747782989,103.122926170285,103.621104557581,104.119282944877,
104.617461332173,105.115639719469,105.613818106765,106.111996494061,106.610174881358,
107.108353268654,107.60653165595,107.937798928196),.UNSPECIFIED.);
#1206=B_SPLINE_CURVE_WITH_KNOTS('',3,(#49114,#49115,#49116,#49117,#49118,
#49119,#49120,#49121,#49122,#49123,#49124,#49125,#49126,#49127,#49128,#49129,
#49130,#49131,#49132,#49133,#49134,#49135,#49136,#49137,#49138,#49139,#49140,
#49141,#49142,#49143,#49144,#49145,#49146,#49147,#49148,#49149,#49150,#49151,
#49152,#49153,#49154,#49155,#49156),.UNSPECIFIED.,.F.,.F.,(4,3,3,3,3,3,
3,3,3,3,3,3,3,3,4),(-117.190265949363,-117.071921014575,-116.573742627279,
-116.075564239983,-115.577385852687,-115.079207465391,-114.581029078095,
-114.082850690798,-113.584672303502,-113.086493916206,-112.58831552891,
-112.090137141614,-111.591958754318,-111.093780367022,-110.907080642184),
 .UNSPECIFIED.);
#1207=B_SPLINE_CURVE_WITH_KNOTS('',3,(#49157,#49158,#49159,#49160,#49161,
#49162,#49163,#49164,#49165,#49166,#49167,#49168,#49169,#49170,#49171,#49172,
#49173,#49174,#49175,#49176,#49177,#49178,#49179,#49180,#49181,#49182,#49183,
#49184,#49185,#49186,#49187,#49188,#49189,#49190,#49191,#49192,#49193,#49194,
#49195,#49196,#49197,#49198,#49199),.UNSPECIFIED.,.F.,.F.,(4,3,3,3,3,3,
3,3,3,3,3,3,3,3,4),(107.937798928196,108.104710043246,108.602888430542,
109.101066817838,109.599245205134,110.09742359243,110.595601979726,111.093780367022,
111.591958754318,112.090137141614,112.58831552891,113.086493916206,113.584672303502,
114.082850690798,114.220984235376),.UNSPECIFIED.);
#1208=B_SPLINE_CURVE_WITH_KNOTS('',3,(#49204,#49205,#49206,#49207,#49208,
#49209,#49210,#49211,#49212,#49213,#49214,#49215,#49216,#49217,#49218,#49219,
#49220,#49221,#49222,#49223,#49224,#49225,#49226,#49227,#49228,#49229,#49230,
#49231,#49232,#49233,#49234,#49235,#49236,#49237,#49238,#49239,#49240,#49241,
#49242,#49243),.UNSPECIFIED.,.F.,.F.,(4,3,3,3,3,3,3,3,3,3,3,3,3,4),(-123.473451256543,
-123.050061662128,-122.551883274832,-122.053704887536,-121.555526500239,
-121.057348112943,-120.559169725647,-120.060991338351,-119.562812951055,
-119.064634563759,-118.566456176463,-118.068277789167,-117.570099401871,
-117.190265949363),.UNSPECIFIED.);
#1209=B_SPLINE_CURVE_WITH_KNOTS('',3,(#49244,#49245,#49246,#49247,#49248,
#49249,#49250,#49251,#49252,#49253,#49254,#49255,#49256,#49257,#49258,#49259,
#49260,#49261,#49262,#49263,#49264,#49265,#49266,#49267,#49268,#49269,#49270,
#49271,#49272,#49273,#49274,#49275,#49276,#49277,#49278,#49279,#49280,#49281,
#49282,#49283),.UNSPECIFIED.,.F.,.F.,(4,3,3,3,3,3,3,3,3,3,3,3,3,4),(114.220984235376,
114.581029078095,115.079207465391,115.577385852687,116.075564239983,116.573742627279,
117.071921014575,117.570099401871,118.068277789167,118.566456176463,119.064634563759,
119.562812951055,120.060991338351,120.504169542555),.UNSPECIFIED.);
#1210=B_SPLINE_CURVE_WITH_KNOTS('',3,(#49288,#49289,#49290,#49291,#49292,
#49293,#49294,#49295,#49296,#49297,#49298,#49299,#49300,#49301,#49302,#49303,
#49304,#49305,#49306,#49307,#49308,#49309,#49310,#49311,#49312,#49313,#49314,
#49315,#49316,#49317,#49318,#49319,#49320,#49321,#49322,#49323,#49324,#49325,
#49326,#49327,#49328,#49329,#49330),.UNSPECIFIED.,.F.,.F.,(4,3,3,3,3,3,
3,3,3,3,3,3,3,3,4),(-129.756636563722,-129.526380696976,-129.02820230968,
-128.530023922384,-128.031845535088,-127.533667147792,-127.035488760496,
-126.5373103732,-126.039131985904,-125.540953598608,-125.042775211312,-124.544596824016,
-124.04641843672,-123.548240049424,-123.473451256543),.UNSPECIFIED.);
#1211=B_SPLINE_CURVE_WITH_KNOTS('',3,(#49331,#49332,#49333,#49334,#49335,
#49336,#49337,#49338,#49339,#49340,#49341,#49342,#49343,#49344,#49345,#49346,
#49347,#49348,#49349,#49350,#49351,#49352,#49353,#49354,#49355,#49356,#49357,
#49358,#49359,#49360,#49361,#49362,#49363,#49364,#49365,#49366,#49367,#49368,
#49369,#49370,#49371,#49372,#49373),.UNSPECIFIED.,.F.,.F.,(4,3,3,3,3,3,
3,3,3,3,3,3,3,3,4),(120.504169542555,120.559169725647,121.057348112943,
121.555526500239,122.053704887535,122.551883274832,123.050061662128,123.548240049424,
124.04641843672,124.544596824016,125.042775211312,125.540953598608,126.039131985904,
126.5373103732,126.787354849735),.UNSPECIFIED.);
#1212=B_SPLINE_CURVE_WITH_KNOTS('',3,(#49378,#49379,#49380,#49381,#49382,
#49383,#49384,#49385,#49386,#49387,#49388,#49389,#49390,#49391,#49392,#49393,
#49394,#49395,#49396,#49397,#49398,#49399,#49400,#49401,#49402,#49403,#49404,
#49405,#49406,#49407,#49408,#49409,#49410,#49411,#49412,#49413,#49414,#49415,
#49416,#49417,#49418,#49419,#49420),.UNSPECIFIED.,.F.,.F.,(4,3,3,3,3,3,
3,3,3,3,3,3,3,3,4),(-136.039821870902,-136.002699731825,-135.504521344529,
-135.006342957233,-134.508164569937,-134.009986182641,-133.511807795345,
-133.013629408049,-132.515451020753,-132.017272633457,-131.519094246161,
-131.020915858865,-130.522737471569,-130.024559084273,-129.756636563722),
 .UNSPECIFIED.);
#1213=B_SPLINE_CURVE_WITH_KNOTS('',3,(#49421,#49422,#49423,#49424,#49425,
#49426,#49427,#49428,#49429,#49430,#49431,#49432,#49433,#49434,#49435,#49436,
#49437,#49438,#49439,#49440,#49441,#49442,#49443,#49444,#49445,#49446,#49447,
#49448,#49449,#49450,#49451,#49452,#49453,#49454,#49455,#49456,#49457,#49458,
#49459,#49460,#49461,#49462,#49463),.UNSPECIFIED.,.F.,.F.,(4,3,3,3,3,3,
3,3,3,3,3,3,3,3,4),(126.787354849735,127.035488760496,127.533667147792,
128.031845535088,128.530023922384,129.02820230968,129.526380696976,130.024559084273,
130.522737471569,131.020915858865,131.519094246161,132.017272633457,132.515451020753,
133.013629408049,133.070540156915),.UNSPECIFIED.);
#1214=B_SPLINE_CURVE_WITH_KNOTS('',3,(#49468,#49469,#49470,#49471,#49472,
#49473,#49474,#49475,#49476,#49477,#49478,#49479,#49480,#49481,#49482,#49483,
#49484,#49485,#49486,#49487,#49488,#49489,#49490,#49491,#49492,#49493,#49494,
#49495,#49496,#49497,#49498,#49499,#49500,#49501,#49502,#49503,#49504,#49505,
#49506,#49507),.UNSPECIFIED.,.F.,.F.,(4,3,3,3,3,3,3,3,3,3,3,3,3,4),(-142.323007178082,
-141.980840379378,-141.482661992082,-140.984483604786,-140.48630521749,
-139.988126830194,-139.489948442898,-138.991770055602,-138.493591668306,
-137.995413281009,-137.497234893713,-136.999056506417,-136.500878119121,
-136.039821870902),.UNSPECIFIED.);
#1215=B_SPLINE_CURVE_WITH_KNOTS('',3,(#49508,#49509,#49510,#49511,#49512,
#49513,#49514,#49515,#49516,#49517,#49518,#49519,#49520,#49521,#49522,#49523,
#49524,#49525,#49526,#49527,#49528,#49529,#49530,#49531,#49532,#49533,#49534,
#49535,#49536,#49537,#49538,#49539,#49540,#49541,#49542,#49543,#49544,#49545,
#49546,#49547),.UNSPECIFIED.,.F.,.F.,(4,3,3,3,3,3,3,3,3,3,3,3,3,4),(133.070540156915,
133.511807795345,134.009986182641,134.508164569937,135.006342957233,135.504521344529,
136.002699731825,136.500878119121,136.999056506417,137.497234893713,137.995413281009,
138.493591668306,138.991770055602,139.353725464094),.UNSPECIFIED.);
#1216=B_SPLINE_CURVE_WITH_KNOTS('',3,(#49552,#49553,#49554,#49555,#49556,
#49557,#49558,#49559,#49560,#49561,#49562,#49563,#49564,#49565,#49566,#49567,
#49568,#49569,#49570,#49571,#49572,#49573,#49574,#49575,#49576,#49577,#49578,
#49579,#49580,#49581,#49582,#49583,#49584,#49585,#49586,#49587,#49588,#49589,
#49590,#49591,#49592,#49593,#49594),.UNSPECIFIED.,.F.,.F.,(4,3,3,3,3,3,
3,3,3,3,3,3,3,3,4),(-148.606192485261,-148.457159414227,-147.958981026931,
-147.460802639635,-146.962624252339,-146.464445865043,-145.966267477746,
-145.46808909045,-144.969910703154,-144.471732315858,-143.973553928562,
-143.475375541266,-142.97719715397,-142.479018766674,-142.323007178082),
 .UNSPECIFIED.);
#1217=B_SPLINE_CURVE_WITH_KNOTS('',3,(#49595,#49596,#49597,#49598,#49599,
#49600,#49601,#49602,#49603,#49604,#49605,#49606,#49607,#49608,#49609,#49610,
#49611,#49612,#49613,#49614,#49615,#49616,#49617,#49618,#49619,#49620,#49621,
#49622,#49623,#49624,#49625,#49626,#49627,#49628,#49629,#49630,#49631,#49632,
#49633,#49634,#49635,#49636,#49637),.UNSPECIFIED.,.F.,.F.,(4,3,3,3,3,3,
3,3,3,3,3,3,3,3,4),(139.353725464094,139.489948442898,139.988126830194,
140.48630521749,140.984483604786,141.482661992082,141.980840379378,142.479018766674,
142.97719715397,143.475375541266,143.973553928562,144.471732315858,144.969910703154,
145.46808909045,145.636910771274),.UNSPECIFIED.);
#1218=B_SPLINE_CURVE_WITH_KNOTS('',3,(#49642,#49643,#49644,#49645,#49646,
#49647,#49648,#49649,#49650,#49651,#49652,#49653,#49654,#49655,#49656,#49657,
#49658,#49659,#49660,#49661,#49662,#49663,#49664,#49665,#49666,#49667,#49668,
#49669,#49670,#49671,#49672,#49673,#49674,#49675,#49676,#49677,#49678,#49679,
#49680,#49681),.UNSPECIFIED.,.F.,.F.,(4,3,3,3,3,3,3,3,3,3,3,3,3,4),(-154.889377792441,
-154.43530006178,-153.937121674484,-153.438943287187,-152.940764899891,
-152.442586512595,-151.944408125299,-151.446229738003,-150.948051350707,
-150.449872963411,-149.951694576115,-149.453516188819,-148.955337801523,
-148.606192485261),.UNSPECIFIED.);
#1219=B_SPLINE_CURVE_WITH_KNOTS('',3,(#49682,#49683,#49684,#49685,#49686,
#49687,#49688,#49689,#49690,#49691,#49692,#49693,#49694,#49695,#49696,#49697,
#49698,#49699,#49700,#49701,#49702,#49703,#49704,#49705,#49706,#49707,#49708,
#49709,#49710,#49711,#49712,#49713,#49714,#49715,#49716,#49717,#49718,#49719,
#49720,#49721),.UNSPECIFIED.,.F.,.F.,(4,3,3,3,3,3,3,3,3,3,3,3,3,4),(145.636910771274,
145.966267477746,146.464445865043,146.962624252339,147.460802639635,147.958981026931,
148.457159414227,148.955337801523,149.453516188819,149.951694576115,150.449872963411,
150.948051350707,151.446229738003,151.920096078453),.UNSPECIFIED.);
#1220=B_SPLINE_CURVE_WITH_KNOTS('',3,(#49726,#49727,#49728,#49729,#49730,
#49731,#49732,#49733,#49734,#49735,#49736,#49737,#49738,#49739,#49740,#49741,
#49742,#49743,#49744,#49745,#49746,#49747,#49748,#49749,#49750,#49751,#49752,
#49753,#49754,#49755,#49756,#49757,#49758,#49759,#49760,#49761,#49762,#49763,
#49764,#49765,#49766,#49767,#49768),.UNSPECIFIED.,.F.,.F.,(4,3,3,3,3,3,
3,3,3,3,3,3,3,3,4),(-161.17256309962,-160.911619096628,-160.413440709332,
-159.915262322036,-159.41708393474,-158.918905547444,-158.420727160148,
-157.922548772852,-157.424370385556,-156.92619199826,-156.428013610964,
-155.929835223668,-155.431656836372,-154.933478449076,-154.889377792441),
 .UNSPECIFIED.);
#1221=B_SPLINE_CURVE_WITH_KNOTS('',3,(#49769,#49770,#49771,#49772,#49773,
#49774,#49775,#49776,#49777,#49778,#49779,#49780,#49781,#49782,#49783,#49784,
#49785,#49786,#49787,#49788,#49789,#49790,#49791,#49792,#49793,#49794,#49795,
#49796,#49797,#49798,#49799,#49800,#49801,#49802,#49803,#49804,#49805,#49806,
#49807,#49808,#49809,#49810,#49811),.UNSPECIFIED.,.F.,.F.,(4,3,3,3,3,3,
3,3,3,3,3,3,3,3,4),(151.920096078453,151.944408125299,152.442586512595,
152.940764899891,153.438943287187,153.937121674484,154.43530006178,154.933478449076,
155.431656836372,155.929835223668,156.428013610964,156.92619199826,157.424370385556,
157.922548772852,158.203281385633),.UNSPECIFIED.);
#1222=B_SPLINE_CURVE_WITH_KNOTS('',3,(#49816,#49817,#49818,#49819,#49820,
#49821,#49822,#49823,#49824,#49825,#49826,#49827,#49828,#49829,#49830,#49831,
#49832,#49833,#49834,#49835,#49836,#49837,#49838,#49839,#49840,#49841,#49842,
#49843,#49844,#49845,#49846,#49847,#49848,#49849,#49850,#49851,#49852,#49853,
#49854,#49855,#49856,#49857,#49858),.UNSPECIFIED.,.F.,.F.,(4,3,3,3,3,3,
3,3,3,3,3,3,3,3,4),(-167.4557484068,-167.387938131477,-166.889759744181,
-166.391581356885,-165.893402969589,-165.395224582293,-164.897046194997,
-164.398867807701,-163.900689420405,-163.402511033109,-162.904332645813,
-162.406154258517,-161.907975871221,-161.409797483924,-161.17256309962),
 .UNSPECIFIED.);
#1223=B_SPLINE_CURVE_WITH_KNOTS('',3,(#49859,#49860,#49861,#49862,#49863,
#49864,#49865,#49866,#49867,#49868,#49869,#49870,#49871,#49872,#49873,#49874,
#49875,#49876,#49877,#49878,#49879,#49880,#49881,#49882,#49883,#49884,#49885,
#49886,#49887,#49888,#49889,#49890,#49891,#49892,#49893,#49894,#49895,#49896,
#49897,#49898,#49899,#49900,#49901),.UNSPECIFIED.,.F.,.F.,(4,3,3,3,3,3,
3,3,3,3,3,3,3,3,4),(158.203281385633,158.420727160148,158.918905547444,
159.41708393474,159.915262322036,160.413440709332,160.911619096628,161.409797483924,
161.907975871221,162.406154258517,162.904332645813,163.402511033109,163.900689420405,
164.398867807701,164.486466692812),.UNSPECIFIED.);
#1224=B_SPLINE_CURVE_WITH_KNOTS('',3,(#49906,#49907,#49908,#49909,#49910,
#49911,#49912,#49913,#49914,#49915,#49916,#49917,#49918,#49919,#49920,#49921,
#49922,#49923,#49924,#49925,#49926,#49927,#49928,#49929,#49930,#49931,#49932,
#49933,#49934,#49935,#49936,#49937,#49938,#49939,#49940,#49941,#49942,#49943,
#49944,#49945),.UNSPECIFIED.,.F.,.F.,(4,3,3,3,3,3,3,3,3,3,3,3,3,4),(-173.738933713979,
-173.36607877903,-172.867900391734,-172.369722004438,-171.871543617142,
-171.373365229846,-170.87518684255,-170.377008455254,-169.878830067958,
-169.380651680662,-168.882473293365,-168.384294906069,-167.886116518773,
-167.4557484068),.UNSPECIFIED.);
#1225=B_SPLINE_CURVE_WITH_KNOTS('',3,(#49946,#49947,#49948,#49949,#49950,
#49951,#49952,#49953,#49954,#49955,#49956,#49957,#49958,#49959,#49960,#49961,
#49962,#49963,#49964,#49965,#49966,#49967,#49968,#49969,#49970,#49971,#49972,
#49973,#49974,#49975,#49976,#49977,#49978,#49979,#49980,#49981,#49982,#49983,
#49984,#49985),.UNSPECIFIED.,.F.,.F.,(4,3,3,3,3,3,3,3,3,3,3,3,3,4),(164.486466692812,
164.897046194997,165.395224582293,165.893402969589,166.391581356885,166.889759744181,
167.387938131477,167.886116518773,168.384294906069,168.882473293365,169.380651680661,
169.878830067958,170.377008455254,170.769651999992),.UNSPECIFIED.);
#1226=B_SPLINE_CURVE_WITH_KNOTS('',3,(#49990,#49991,#49992,#49993,#49994,
#49995,#49996,#49997,#49998,#49999,#50000,#50001,#50002,#50003,#50004,#50005,
#50006,#50007,#50008,#50009,#50010,#50011,#50012,#50013,#50014,#50015,#50016,
#50017,#50018,#50019,#50020,#50021,#50022,#50023,#50024,#50025,#50026,#50027,
#50028,#50029,#50030,#50031,#50032),.UNSPECIFIED.,.F.,.F.,(4,3,3,3,3,3,
3,3,3,3,3,3,3,3,4),(-180.022119021159,-179.842397813879,-179.344219426583,
-178.846041039287,-178.347862651991,-177.849684264695,-177.351505877398,
-176.853327490102,-176.355149102806,-175.85697071551,-175.358792328214,
-174.860613940918,-174.362435553622,-173.864257166326,-173.738933713979),
 .UNSPECIFIED.);
#1227=B_SPLINE_CURVE_WITH_KNOTS('',3,(#50033,#50034,#50035,#50036,#50037,
#50038,#50039,#50040,#50041,#50042,#50043,#50044,#50045,#50046,#50047,#50048,
#50049,#50050,#50051,#50052,#50053,#50054,#50055,#50056,#50057,#50058,#50059,
#50060,#50061,#50062,#50063,#50064,#50065,#50066,#50067,#50068,#50069,#50070,
#50071,#50072,#50073,#50074,#50075),.UNSPECIFIED.,.F.,.F.,(4,3,3,3,3,3,
3,3,3,3,3,3,3,3,4),(170.769651999992,170.87518684255,171.373365229846,171.871543617142,
172.369722004438,172.867900391734,173.36607877903,173.864257166326,174.362435553622,
174.860613940918,175.358792328214,175.85697071551,176.355149102806,176.853327490102,
177.052837307172),.UNSPECIFIED.);
#1228=B_SPLINE_CURVE_WITH_KNOTS('',3,(#50081,#50082,#50083,#50084),
 .UNSPECIFIED.,.F.,.F.,(4,4),(191.637151868977,191.873336125493),
 .UNSPECIFIED.);
#1229=B_SPLINE_CURVE_WITH_KNOTS('',3,(#50090,#50091,#50092,#50093,#50094,
#50095,#50096,#50097,#50098,#50099,#50100,#50101,#50102,#50103,#50104,#50105,
#50106),.UNSPECIFIED.,.F.,.F.,(4,1,1,1,1,1,1,1,1,1,1,1,1,1,4),(185.353966561798,
185.479290014144,185.97746840144,186.475646788737,186.973825176033,187.472003563329,
187.970181950625,188.468360337921,188.966538725217,189.464717112513,189.962895499809,
190.461073887105,190.959252274401,191.457430661697,191.637151868977),
 .UNSPECIFIED.);
#1230=B_SPLINE_CURVE_WITH_KNOTS('',3,(#50109,#50110,#50111,#50112,#50113,
#50114,#50115,#50116,#50117,#50118,#50119,#50120,#50121,#50122),
 .UNSPECIFIED.,.F.,.F.,(4,1,1,1,1,1,1,1,1,1,1,4),(185.353966561798,185.652635132025,
186.150813519321,186.648991906617,187.147170293913,187.645348681209,188.143527068505,
188.641705455801,189.139883843097,189.638062230393,190.136240617689,190.634419004985),
 .UNSPECIFIED.);
#1231=B_SPLINE_CURVE_WITH_KNOTS('',3,(#50127,#50128,#50129,#50130,#50131,
#50132,#50133,#50134,#50135,#50136,#50137,#50138,#50139,#50140,#50141,#50142),
 .UNSPECIFIED.,.F.,.F.,(4,1,1,1,1,1,1,1,1,1,1,1,1,4),(179.070781254618,
179.501149366592,179.999327753888,180.497506141184,180.99568452848,181.493862915776,
181.992041303072,182.490219690368,182.988398077664,183.48657646496,183.984754852256,
184.482933239552,184.981111626848,185.353966561798),.UNSPECIFIED.);
#1232=B_SPLINE_CURVE_WITH_KNOTS('',3,(#50143,#50144,#50145,#50146,#50147,
#50148,#50149,#50150,#50151,#50152,#50153,#50154,#50155,#50156,#50157,#50158,
#50159),.UNSPECIFIED.,.F.,.F.,(4,1,1,1,1,1,1,1,1,1,1,1,1,1,4),(179.070781254618,
179.176316097176,179.674494484472,180.172672871768,180.670851259064,181.16902964636,
181.667208033656,182.165386420952,182.663564808248,183.161743195545,183.659921582841,
184.158099970137,184.656278357433,185.154456744729,185.353966561798),
 .UNSPECIFIED.);
#1233=B_SPLINE_CURVE_WITH_KNOTS('',3,(#50164,#50165,#50166,#50167,#50168,
#50169,#50170,#50171,#50172,#50173,#50174,#50175,#50176,#50177,#50178,#50179,
#50180),.UNSPECIFIED.,.F.,.F.,(4,1,1,1,1,1,1,1,1,1,1,1,1,1,4),(172.787595947439,
173.024830331743,173.523008719039,174.021187106335,174.519365493631,175.017543880927,
175.515722268223,176.013900655519,176.512079042815,177.010257430111,177.508435817407,
178.006614204703,178.504792592,179.002970979296,179.070781254618),
 .UNSPECIFIED.);
#1234=B_SPLINE_CURVE_WITH_KNOTS('',3,(#50181,#50182,#50183,#50184,#50185,
#50186,#50187,#50188,#50189,#50190,#50191,#50192,#50193,#50194,#50195,#50196),
 .UNSPECIFIED.,.F.,.F.,(4,1,1,1,1,1,1,1,1,1,1,1,1,4),(172.787595947439,
173.198175449623,173.696353836919,174.194532224215,174.692710611511,175.190888998808,
175.689067386104,176.1872457734,176.685424160696,177.183602547992,177.681780935288,
178.179959322584,178.67813770988,179.070781254618),.UNSPECIFIED.);
#1235=B_SPLINE_CURVE_WITH_KNOTS('',3,(#50201,#50202,#50203,#50204,#50205,
#50206,#50207,#50208,#50209,#50210,#50211,#50212,#50213,#50214,#50215,#50216,
#50217),.UNSPECIFIED.,.F.,.F.,(4,1,1,1,1,1,1,1,1,1,1,1,1,1,4),(166.504410640259,
166.548511296894,167.04668968419,167.544868071486,168.043046458782,168.541224846078,
169.039403233374,169.53758162067,170.035760007966,170.533938395263,171.032116782559,
171.530295169855,172.028473557151,172.526651944447,172.787595947439),
 .UNSPECIFIED.);
#1236=B_SPLINE_CURVE_WITH_KNOTS('',3,(#50218,#50219,#50220,#50221,#50222,
#50223,#50224,#50225,#50226,#50227,#50228,#50229,#50230,#50231,#50232,#50233,
#50234),.UNSPECIFIED.,.F.,.F.,(4,1,1,1,1,1,1,1,1,1,1,1,1,1,4),(166.504410640259,
166.721856414774,167.220034802071,167.718213189367,168.216391576663,168.714569963959,
169.212748351255,169.710926738551,170.209105125847,170.707283513143,171.205461900439,
171.703640287735,172.201818675031,172.699997062327,172.787595947439),
 .UNSPECIFIED.);
#1237=B_SPLINE_CURVE_WITH_KNOTS('',3,(#50239,#50240,#50241,#50242,#50243,
#50244,#50245,#50246,#50247,#50248,#50249,#50250,#50251,#50252,#50253,#50254),
 .UNSPECIFIED.,.F.,.F.,(4,1,1,1,1,1,1,1,1,1,1,1,1,4),(160.22122533308,160.570370649341,
161.068549036637,161.566727423933,162.064905811229,162.563084198526,163.061262585822,
163.559440973118,164.057619360414,164.55579774771,165.053976135006,165.552154522302,
166.050332909598,166.504410640259),.UNSPECIFIED.);
#1238=B_SPLINE_CURVE_WITH_KNOTS('',3,(#50255,#50256,#50257,#50258,#50259,
#50260,#50261,#50262,#50263,#50264,#50265,#50266,#50267,#50268,#50269,#50270,
#50271),.UNSPECIFIED.,.F.,.F.,(4,1,1,1,1,1,1,1,1,1,1,1,1,1,4),(160.22122533308,
160.245537379926,160.743715767222,161.241894154518,161.740072541814,162.23825092911,
162.736429316406,163.234607703702,163.732786090998,164.230964478294,164.72914286559,
165.227321252886,165.725499640182,166.223678027478,166.504410640259),
 .UNSPECIFIED.);
#1239=B_SPLINE_CURVE_WITH_KNOTS('',3,(#50276,#50277,#50278,#50279,#50280,
#50281,#50282,#50283,#50284,#50285,#50286,#50287,#50288,#50289,#50290,#50291,
#50292),.UNSPECIFIED.,.F.,.F.,(4,1,1,1,1,1,1,1,1,1,1,1,1,1,4),(153.9380400259,
154.094051614492,154.592230001789,155.090408389085,155.588586776381,156.086765163677,
156.584943550973,157.083121938269,157.581300325565,158.079478712861,158.577657100157,
159.075835487453,159.574013874749,160.072192262045,160.22122533308),
 .UNSPECIFIED.);
#1240=B_SPLINE_CURVE_WITH_KNOTS('',3,(#50293,#50294,#50295,#50296,#50297,
#50298,#50299,#50300,#50301,#50302,#50303,#50304,#50305,#50306,#50307,#50308),
 .UNSPECIFIED.,.F.,.F.,(4,1,1,1,1,1,1,1,1,1,1,1,1,4),(153.9380400259,154.267396732373,
154.765575119669,155.263753506965,155.761931894261,156.260110281557,156.758288668853,
157.256467056149,157.754645443445,158.252823830741,158.751002218037,159.249180605333,
159.74735899263,160.22122533308),.UNSPECIFIED.);
#1241=B_SPLINE_CURVE_WITH_KNOTS('',3,(#50313,#50314,#50315,#50316,#50317,
#50318,#50319,#50320,#50321,#50322,#50323,#50324,#50325,#50326,#50327,#50328),
 .UNSPECIFIED.,.F.,.F.,(4,1,1,1,1,1,1,1,1,1,1,1,1,4),(147.65485471872,148.11591096694,
148.614089354236,149.112267741532,149.610446128828,150.108624516124,150.60680290342,
151.104981290716,151.603159678012,152.101338065308,152.599516452604,153.0976948399,
153.595873227196,153.9380400259),.UNSPECIFIED.);
#1242=B_SPLINE_CURVE_WITH_KNOTS('',3,(#50329,#50330,#50331,#50332,#50333,
#50334,#50335,#50336,#50337,#50338,#50339,#50340,#50341,#50342,#50343,#50344,
#50345),.UNSPECIFIED.,.F.,.F.,(4,1,1,1,1,1,1,1,1,1,1,1,1,1,4),(147.65485471872,
147.791077697524,148.28925608482,148.787434472116,149.285612859412,149.783791246708,
150.281969634004,150.7801480213,151.278326408596,151.776504795893,152.274683183189,
152.772861570485,153.271039957781,153.769218345077,153.9380400259),
 .UNSPECIFIED.);
#1243=B_SPLINE_CURVE_WITH_KNOTS('',3,(#50350,#50351,#50352,#50353,#50354,
#50355,#50356,#50357,#50358,#50359,#50360,#50361,#50362,#50363,#50364,#50365,
#50366),.UNSPECIFIED.,.F.,.F.,(4,1,1,1,1,1,1,1,1,1,1,1,1,1,4),(141.371669411541,
141.639591932091,142.137770319387,142.635948706683,143.134127093979,143.632305481275,
144.130483868571,144.628662255867,145.126840643163,145.625019030459,146.123197417755,
146.621375805052,147.119554192348,147.617732579644,147.65485471872),
 .UNSPECIFIED.);
#1244=B_SPLINE_CURVE_WITH_KNOTS('',3,(#50367,#50368,#50369,#50370,#50371,
#50372,#50373,#50374,#50375,#50376,#50377,#50378,#50379,#50380,#50381,#50382),
 .UNSPECIFIED.,.F.,.F.,(4,1,1,1,1,1,1,1,1,1,1,1,1,4),(141.371669411541,
141.812937049971,142.311115437267,142.809293824563,143.307472211859,143.805650599156,
144.303828986452,144.802007373748,145.300185761044,145.79836414834,146.296542535636,
146.794720922932,147.292899310228,147.65485471872),.UNSPECIFIED.);
#1245=B_SPLINE_CURVE_WITH_KNOTS('',3,(#50387,#50388,#50389,#50390,#50391,
#50392,#50393,#50394,#50395,#50396,#50397,#50398,#50399,#50400,#50401,#50402,
#50403),.UNSPECIFIED.,.F.,.F.,(4,1,1,1,1,1,1,1,1,1,1,1,1,1,4),(135.088484104361,
135.163272897242,135.661451284538,136.159629671834,136.65780805913,137.155986446426,
137.654164833722,138.152343221018,138.650521608314,139.148699995611,139.646878382907,
140.145056770203,140.643235157499,141.141413544795,141.371669411541),
 .UNSPECIFIED.);
#1246=B_SPLINE_CURVE_WITH_KNOTS('',3,(#50404,#50405,#50406,#50407,#50408,
#50409,#50410,#50411,#50412,#50413,#50414,#50415,#50416,#50417,#50418,#50419,
#50420),.UNSPECIFIED.,.F.,.F.,(4,1,1,1,1,1,1,1,1,1,1,1,1,1,4),(135.088484104361,
135.336618015122,135.834796402419,136.332974789715,136.831153177011,137.329331564307,
137.827509951603,138.325688338899,138.823866726195,139.322045113491,139.820223500787,
140.318401888083,140.816580275379,141.314758662675,141.371669411541),
 .UNSPECIFIED.);
#1247=B_SPLINE_CURVE_WITH_KNOTS('',3,(#50425,#50426,#50427,#50428,#50429,
#50430,#50431,#50432,#50433,#50434,#50435,#50436,#50437,#50438,#50439,#50440),
 .UNSPECIFIED.,.F.,.F.,(4,1,1,1,1,1,1,1,1,1,1,1,1,4),(128.805298797182,
129.185132249689,129.683310636985,130.181489024281,130.679667411577,131.177845798874,
131.67602418617,132.174202573466,132.672380960762,133.170559348058,133.668737735354,
134.16691612265,134.665094509946,135.088484104361),.UNSPECIFIED.);
#1248=B_SPLINE_CURVE_WITH_KNOTS('',3,(#50441,#50442,#50443,#50444,#50445,
#50446,#50447,#50448,#50449,#50450,#50451,#50452,#50453,#50454,#50455,#50456,
#50457),.UNSPECIFIED.,.F.,.F.,(4,1,1,1,1,1,1,1,1,1,1,1,1,1,4),(128.805298797182,
128.860298980274,129.35847736757,129.856655754866,130.354834142162,130.853012529458,
131.351190916754,131.84936930405,132.347547691346,132.845726078642,133.343904465938,
133.842082853234,134.34026124053,134.838439627826,135.088484104361),
 .UNSPECIFIED.);
#1249=B_SPLINE_CURVE_WITH_KNOTS('',3,(#50462,#50463,#50464,#50465,#50466,
#50467,#50468,#50469,#50470,#50471,#50472,#50473,#50474,#50475,#50476,#50477,
#50478),.UNSPECIFIED.,.F.,.F.,(4,1,1,1,1,1,1,1,1,1,1,1,1,1,4),(122.522113490002,
122.70881321484,123.206991602137,123.705169989433,124.203348376729,124.701526764025,
125.199705151321,125.697883538617,126.196061925913,126.694240313209,127.192418700505,
127.690597087801,128.188775475097,128.686953862393,128.805298797182),
 .UNSPECIFIED.);
#1250=B_SPLINE_CURVE_WITH_KNOTS('',3,(#50479,#50480,#50481,#50482,#50483,
#50484,#50485,#50486,#50487,#50488,#50489,#50490,#50491,#50492,#50493,#50494),
 .UNSPECIFIED.,.F.,.F.,(4,1,1,1,1,1,1,1,1,1,1,1,1,4),(122.522113490002,
122.882158332721,123.380336720017,123.878515107313,124.376693494609,124.874871881905,
125.373050269201,125.871228656497,126.369407043793,126.867585431089,127.365763818385,
127.863942205682,128.362120592978,128.805298797182),.UNSPECIFIED.);
#1251=B_SPLINE_CURVE_WITH_KNOTS('',3,(#50499,#50500,#50501,#50502,#50503,
#50504,#50505,#50506,#50507,#50508,#50509,#50510,#50511,#50512,#50513,#50514),
 .UNSPECIFIED.,.F.,.F.,(4,1,1,1,1,1,1,1,1,1,1,1,1,4),(116.238928182823,
116.730672567288,117.228850954584,117.72702934188,118.225207729176,118.723386116472,
119.221564503768,119.719742891064,120.21792127836,120.716099665656,121.214278052952,
121.712456440248,122.210634827544,122.522113490002),.UNSPECIFIED.);
#1252=B_SPLINE_CURVE_WITH_KNOTS('',3,(#50515,#50516,#50517,#50518,#50519,
#50520,#50521,#50522,#50523,#50524,#50525,#50526,#50527,#50528,#50529,#50530,
#50531),.UNSPECIFIED.,.F.,.F.,(4,1,1,1,1,1,1,1,1,1,1,1,1,1,4),(116.238928182823,
116.405839297872,116.904017685168,117.402196072464,117.90037445976,118.398552847056,
118.896731234352,119.394909621648,119.893088008945,120.391266396241,120.889444783537,
121.387623170833,121.885801558129,122.383979945425,122.522113490002),
 .UNSPECIFIED.);
#1253=B_SPLINE_CURVE_WITH_KNOTS('',3,(#50536,#50537,#50538,#50539,#50540,
#50541,#50542,#50543,#50544,#50545,#50546,#50547,#50548,#50549,#50550,#50551,
#50552),.UNSPECIFIED.,.F.,.F.,(4,1,1,1,1,1,1,1,1,1,1,1,1,1,4),(109.955742875643,
110.254353532439,110.752531919735,111.250710307031,111.748888694327,112.247067081623,
112.745245468919,113.243423856215,113.741602243511,114.239780630807,114.737959018103,
115.2361374054,115.734315792696,116.232494179992,116.238928182823),
 .UNSPECIFIED.);
#1254=B_SPLINE_CURVE_WITH_KNOTS('',3,(#50553,#50554,#50555,#50556,#50557,
#50558,#50559,#50560,#50561,#50562,#50563,#50564,#50565,#50566,#50567,#50568),
 .UNSPECIFIED.,.F.,.F.,(4,1,1,1,1,1,1,1,1,1,1,1,1,4),(109.955742875643,
110.427698650319,110.925877037615,111.424055424911,111.922233812207,112.420412199504,
112.9185905868,113.416768974096,113.914947361392,114.413125748688,114.911304135984,
115.40948252328,115.907660910576,116.238928182823),.UNSPECIFIED.);
#1255=B_SPLINE_CURVE_WITH_KNOTS('',3,(#50573,#50574,#50575,#50576,#50577,
#50578,#50579,#50580,#50581,#50582,#50583,#50584,#50585,#50586,#50587,#50588,
#50589),.UNSPECIFIED.,.F.,.F.,(4,1,1,1,1,1,1,1,1,1,1,1,1,1,4),(103.672557568463,
103.77803449759,104.276212884886,104.774391272182,105.272569659478,105.770748046774,
106.26892643407,106.767104821366,107.265283208663,107.763461595959,108.261639983255,
108.759818370551,109.257996757847,109.756175145143,109.955742875643),
 .UNSPECIFIED.);
#1256=B_SPLINE_CURVE_WITH_KNOTS('',3,(#50590,#50591,#50592,#50593,#50594,
#50595,#50596,#50597,#50598,#50599,#50600,#50601,#50602,#50603,#50604,#50605,
#50606),.UNSPECIFIED.,.F.,.F.,(4,1,1,1,1,1,1,1,1,1,1,1,1,1,4),(103.672557568463,
103.95137961547,104.449558002767,104.947736390063,105.445914777359,105.944093164655,
106.442271551951,106.940449939247,107.438628326543,107.936806713839,108.434985101135,
108.933163488431,109.431341875727,109.929520263023,109.955742875643),
 .UNSPECIFIED.);
#1257=B_SPLINE_CURVE_WITH_KNOTS('',3,(#50611,#50612,#50613,#50614,#50615,
#50616,#50617,#50618,#50619,#50620,#50621,#50622,#50623,#50624,#50625,#50626),
 .UNSPECIFIED.,.F.,.F.,(4,1,1,1,1,1,1,1,1,1,1,1,1,4),(97.3893722612837,
97.7998938500373,98.2980722373334,98.7962506246294,99.2944290119255,99.7926073992216,
100.290785786518,100.788964173814,101.28714256111,101.785320948406,102.283499335702,
102.781677722998,103.279856110294,103.672557568463),.UNSPECIFIED.);
#1258=B_SPLINE_CURVE_WITH_KNOTS('',3,(#50627,#50628,#50629,#50630,#50631,
#50632,#50633,#50634,#50635,#50636,#50637,#50638,#50639,#50640,#50641,#50642,
#50643),.UNSPECIFIED.,.F.,.F.,(4,1,1,1,1,1,1,1,1,1,1,1,1,1,4),(97.3893722612837,
97.4750605806217,97.9732389679177,98.4714173552138,98.9695957425099,99.4677741298059,
99.965952517102,100.464130904398,100.962309291694,101.46048767899,101.958666066286,
102.456844453582,102.955022840878,103.453201228174,103.672557568463),
 .UNSPECIFIED.);
#1259=B_SPLINE_CURVE_WITH_KNOTS('',3,(#50648,#50649,#50650,#50651,#50652,
#50653,#50654,#50655,#50656,#50657,#50658,#50659,#50660,#50661,#50662,#50663,
#50664),.UNSPECIFIED.,.F.,.F.,(4,1,1,1,1,1,1,1,1,1,1,1,1,1,4),(91.1061869541041,
91.3235748151885,91.8217532024846,92.3199315897806,92.8181099770767,93.3162883643727,
93.8144667516688,94.3126451389649,94.8108235262609,95.309001913557,95.8071803008531,
96.3053586881491,96.8035370754452,97.3017154627413,97.3893722612837),
 .UNSPECIFIED.);
#1260=B_SPLINE_CURVE_WITH_KNOTS('',3,(#50665,#50666,#50667,#50668,#50669,
#50670,#50671,#50672,#50673,#50674,#50675,#50676,#50677,#50678,#50679,#50680),
 .UNSPECIFIED.,.F.,.F.,(4,1,1,1,1,1,1,1,1,1,1,1,1,4),(91.1061869541041,
91.4969199330689,91.995098320365,92.493276707661,92.9914550949571,93.4896334822532,
93.9878118695492,94.4859902568453,94.9841686441413,95.4823470314374,95.9805254187335,
96.4787038060295,96.9768821933256,97.3893722612837),.UNSPECIFIED.);
#1261=B_SPLINE_CURVE_WITH_KNOTS('',3,(#50685,#50686,#50687,#50688,#50689,
#50690,#50691,#50692,#50693,#50694,#50695,#50696,#50697,#50698,#50699,#50700,
#50701),.UNSPECIFIED.,.F.,.F.,(4,1,1,1,1,1,1,1,1,1,1,1,1,1,4),(84.8230016469245,
84.8472557803397,85.3454341676357,85.8436125549318,86.3417909422279,86.8399693295239,
87.33814771682,87.8363261041161,88.3345044914121,88.8326828787082,89.3308612660042,
89.8290396533003,90.3272180405964,90.8253964278924,91.1061869541041),
 .UNSPECIFIED.);
#1262=B_SPLINE_CURVE_WITH_KNOTS('',3,(#50702,#50703,#50704,#50705,#50706,
#50707,#50708,#50709,#50710,#50711,#50712,#50713,#50714,#50715,#50716,#50717,
#50718),.UNSPECIFIED.,.F.,.F.,(4,1,1,1,1,1,1,1,1,1,1,1,1,1,4),(84.8230016469245,
85.0206008982201,85.5187792855161,86.0169576728122,86.5151360601083,87.0133144474043,
87.5114928347004,88.0096712219965,88.5078496092925,89.0060279965886,89.5042063838847,
90.0023847711807,90.5005631584768,90.9987415457728,91.1061869541041),
 .UNSPECIFIED.);
#1263=B_SPLINE_CURVE_WITH_KNOTS('',3,(#50723,#50724,#50725,#50726,#50727,
#50728,#50729,#50730,#50731,#50732,#50733,#50734,#50735,#50736,#50737,#50738),
 .UNSPECIFIED.,.F.,.F.,(4,1,1,1,1,1,1,1,1,1,1,1,1,4),(78.539816339745,78.8691151327869,
79.367293520083,79.865471907379,80.3636502946751,80.8618286819712,81.3600070692672,
81.8581854565633,82.3563638438594,82.8545422311554,83.3527206184515,83.8508990057476,
84.3490773930436,84.8230016469245),.UNSPECIFIED.);
#1264=B_SPLINE_CURVE_WITH_KNOTS('',3,(#50739,#50740,#50741,#50742,#50743,
#50744,#50745,#50746,#50747,#50748,#50749,#50750,#50751,#50752,#50753,#50754,
#50755),.UNSPECIFIED.,.F.,.F.,(4,1,1,1,1,1,1,1,1,1,1,1,1,1,4),(78.539816339745,
78.5442818633713,79.0424602506673,79.5406386379634,80.0388170252594,80.5369954125555,
81.0351737998516,81.5333521871476,82.0315305744437,82.5297089617398,83.0278873490358,
83.5260657363319,84.024244123628,84.522422510924,84.8230016469245),
 .UNSPECIFIED.);
#1265=B_SPLINE_CURVE_WITH_KNOTS('',3,(#50760,#50761,#50762,#50763,#50764,
#50765,#50766,#50767,#50768,#50769,#50770,#50771,#50772,#50773,#50774,#50775,
#50776),.UNSPECIFIED.,.F.,.F.,(4,1,1,1,1,1,1,1,1,1,1,1,1,1,4),(72.2566310325654,
72.3927960979381,72.8909744852342,73.3891528725302,73.8873312598263,74.3855096471223,
74.8836880344184,75.3818664217145,75.8800448090105,76.3782231963066,76.8764015836027,
77.3745799708987,77.8727583581948,78.3709367454909,78.539816339745),
 .UNSPECIFIED.);
#1266=B_SPLINE_CURVE_WITH_KNOTS('',3,(#50777,#50778,#50779,#50780,#50781,
#50782,#50783,#50784,#50785,#50786,#50787,#50788,#50789,#50790,#50791,#50792),
 .UNSPECIFIED.,.F.,.F.,(4,1,1,1,1,1,1,1,1,1,1,1,1,4),(72.2566310325654,
72.5661412158185,73.0643196031146,73.5624979904106,74.0606763777067,74.5588547650028,
75.0570331522988,75.5552115395949,76.053389926891,76.551568314187,77.0497467014831,
77.5479250887791,78.0461034760752,78.539816339745),.UNSPECIFIED.);
#1267=B_SPLINE_CURVE_WITH_KNOTS('',3,(#50797,#50798,#50799,#50800,#50801,
#50802,#50803,#50804,#50805,#50806,#50807,#50808,#50809,#50810,#50811,#50812),
 .UNSPECIFIED.,.F.,.F.,(4,1,1,1,1,1,1,1,1,1,1,1,1,4),(65.9734457253858,
66.4146554503853,66.9128338376814,67.4110122249775,67.9091906122735,68.4073689995696,
68.9055473868656,69.4037257741617,69.9019041614578,70.4000825487538,70.8982609360499,
71.396439323346,71.894617710642,72.2566310325654),.UNSPECIFIED.);
#1268=B_SPLINE_CURVE_WITH_KNOTS('',3,(#50813,#50814,#50815,#50816,#50817,
#50818,#50819,#50820,#50821,#50822,#50823,#50824,#50825,#50826,#50827,#50828,
#50829),.UNSPECIFIED.,.F.,.F.,(4,1,1,1,1,1,1,1,1,1,1,1,1,1,4),(65.9734457253858,
66.0898221809697,66.5880005682658,67.0861789555618,67.5843573428579,68.0825357301539,
68.58071411745,69.0788925047461,69.5770708920421,70.0752492793382,70.5734276666342,
71.0716060539303,71.5697844412264,72.0679628285224,72.2566310325654),
 .UNSPECIFIED.);
#1269=B_SPLINE_CURVE_WITH_KNOTS('',3,(#50834,#50835,#50836,#50837,#50838,
#50839,#50840,#50841,#50842,#50843,#50844,#50845,#50846,#50847,#50848,#50849,
#50850),.UNSPECIFIED.,.F.,.F.,(4,1,1,1,1,1,1,1,1,1,1,1,1,1,4),(59.6902604182062,
59.9383364155365,60.4365148028326,60.9346931901286,61.4328715774247,61.9310499647208,
62.4292283520168,62.9274067393129,63.425585126609,63.923763513905,64.4219419012011,
64.9201202884971,65.4182986757932,65.9164770630893,65.9734457253858),
 .UNSPECIFIED.);
#1270=B_SPLINE_CURVE_WITH_KNOTS('',3,(#50851,#50852,#50853,#50854,#50855,
#50856,#50857,#50858,#50859,#50860,#50861,#50862,#50863,#50864,#50865,#50866),
 .UNSPECIFIED.,.F.,.F.,(4,1,1,1,1,1,1,1,1,1,1,1,1,4),(59.6902604182062,
60.1116815334169,60.609859920713,61.108038308009,61.6062166953051,62.1043950826012,
62.6025734698972,63.1007518571933,63.5989302444894,64.0971086317854,64.5952870190815,
65.0934654063776,65.5916437936736,65.9734457253858),.UNSPECIFIED.);
#1271=B_SPLINE_CURVE_WITH_KNOTS('',3,(#50871,#50872,#50873,#50874,#50875,
#50876,#50877,#50878,#50879,#50880,#50881,#50882,#50883,#50884,#50885,#50886,
#50887),.UNSPECIFIED.,.F.,.F.,(4,1,1,1,1,1,1,1,1,1,1,1,1,1,4),(53.4070751110266,
53.4620173806877,53.9601957679837,54.4583741552798,54.9565525425759,55.4547309298719,
55.952909317168,56.4510877044641,56.9492660917601,57.4474444790562,57.9456228663523,
58.4438012536483,58.9419796409444,59.4401580282404,59.6902604182062),
 .UNSPECIFIED.);
#1272=B_SPLINE_CURVE_WITH_KNOTS('',3,(#50888,#50889,#50890,#50891,#50892,
#50893,#50894,#50895,#50896,#50897,#50898,#50899,#50900,#50901,#50902,#50903,
#50904),.UNSPECIFIED.,.F.,.F.,(4,1,1,1,1,1,1,1,1,1,1,1,1,1,4),(53.4070751110266,
53.6353624985681,54.1335408858642,54.6317192731602,55.1298976604563,55.6280760477524,
56.1262544350484,56.6244328223445,57.1226112096405,57.6207895969366,58.1189679842327,
58.6171463715287,59.1153247588248,59.6135031461209,59.6902604182062),
 .UNSPECIFIED.);
#1273=B_SPLINE_CURVE_WITH_KNOTS('',3,(#50909,#50910,#50911,#50912,#50913,
#50914,#50915,#50916,#50917,#50918,#50919,#50920,#50921,#50922,#50923,#50924),
 .UNSPECIFIED.,.F.,.F.,(4,1,1,1,1,1,1,1,1,1,1,1,1,4),(47.123889803847,47.4838767331349,
47.982055120431,48.480233507727,48.9784118950231,49.4765902823192,49.9747686696152,
50.4729470569113,50.9711254442074,51.4693038315034,51.9674822187995,52.4656606060956,
52.9638389933916,53.4070751110266),.UNSPECIFIED.);
#1274=B_SPLINE_CURVE_WITH_KNOTS('',3,(#50925,#50926,#50927,#50928,#50929,
#50930,#50931,#50932,#50933,#50934,#50935,#50936,#50937,#50938,#50939,#50940,
#50941),.UNSPECIFIED.,.F.,.F.,(4,1,1,1,1,1,1,1,1,1,1,1,1,1,4),(47.123889803847,
47.1590434637193,47.6572218510153,48.1554002383114,48.6535786256075,49.1517570129035,
49.6499354001996,50.1481137874957,50.6462921747917,51.1444705620878,51.6426489493839,
52.1408273366799,52.639005723976,53.137184111272,53.4070751110266),
 .UNSPECIFIED.);
#1275=B_SPLINE_CURVE_WITH_KNOTS('',3,(#50946,#50947,#50948,#50949,#50950,
#50951,#50952,#50953,#50954,#50955,#50956,#50957,#50958,#50959,#50960,#50961,
#50962),.UNSPECIFIED.,.F.,.F.,(4,1,1,1,1,1,1,1,1,1,1,1,1,1,4),(40.8407044966674,
41.0075576982861,41.5057360855822,42.0039144728782,42.5020928601743,43.0002712474704,
43.4984496347664,43.9966280220625,44.4948064093585,44.9929847966546,45.4911631839507,
45.9893415712467,46.4875199585428,46.9856983458389,47.123889803847),
 .UNSPECIFIED.);
#1276=B_SPLINE_CURVE_WITH_KNOTS('',3,(#50963,#50964,#50965,#50966,#50967,
#50968,#50969,#50970,#50971,#50972,#50973,#50974,#50975,#50976,#50977,#50978),
 .UNSPECIFIED.,.F.,.F.,(4,1,1,1,1,1,1,1,1,1,1,1,1,4),(40.8407044966674,
41.1809028161665,41.6790812034626,42.1772595907587,42.6754379780547,43.1736163653508,
43.6717947526468,44.1699731399429,44.668151527239,45.166329914535,45.6645083018311,
46.1626866891272,46.6608650764232,47.123889803847),.UNSPECIFIED.);
#1277=B_SPLINE_CURVE_WITH_KNOTS('',3,(#50983,#50984,#50985,#50986,#50987,
#50988,#50989,#50990,#50991,#50992,#50993,#50994,#50995,#50996,#50997,#50998),
 .UNSPECIFIED.,.F.,.F.,(4,1,1,1,1,1,1,1,1,1,1,1,1,4),(34.5575191894878,
35.0294170507333,35.5275954380294,36.0257738253255,36.5239522126215,37.0221305999176,
37.5203089872137,38.0184873745097,38.5166657618058,39.0148441491019,39.5130225363979,
40.011200923694,40.50937931099,40.8407044966674),.UNSPECIFIED.);
#1278=B_SPLINE_CURVE_WITH_KNOTS('',3,(#50999,#51000,#51001,#51002,#51003,
#51004,#51005,#51006,#51007,#51008,#51009,#51010,#51011,#51012,#51013,#51014,
#51015),.UNSPECIFIED.,.F.,.F.,(4,1,1,1,1,1,1,1,1,1,1,1,1,1,4),(34.5575191894878,
34.7045837813177,35.2027621686138,35.7009405559098,36.1991189432059,36.697297330502,
37.195475717798,37.6936541050941,38.1918324923901,38.6900108796862,39.1881892669823,
39.6863676542783,40.1845460415744,40.6827244288705,40.8407044966674),
 .UNSPECIFIED.);
#1279=B_SPLINE_CURVE_WITH_KNOTS('',3,(#51020,#51021,#51022,#51023,#51024,
#51025,#51026,#51027,#51028,#51029,#51030,#51031,#51032,#51033,#51034,#51035,
#51036),.UNSPECIFIED.,.F.,.F.,(4,1,1,1,1,1,1,1,1,1,1,1,1,1,4),(28.2743338823082,
28.5530980158845,29.0512764031806,29.5494547904767,30.0476331777727,30.5458115650688,
31.0439899523648,31.5421683396609,32.040346726957,32.538525114253,33.0367035015491,
33.5348818888452,34.0330602761412,34.5312386634373,34.5575191894878),
 .UNSPECIFIED.);
#1280=B_SPLINE_CURVE_WITH_KNOTS('',3,(#51037,#51038,#51039,#51040,#51041,
#51042,#51043,#51044,#51045,#51046,#51047,#51048,#51049,#51050,#51051,#51052),
 .UNSPECIFIED.,.F.,.F.,(4,1,1,1,1,1,1,1,1,1,1,1,1,4),(28.2743338823082,
28.7264431337649,29.224621521061,29.7227999083571,30.2209782956531,30.7191566829492,
31.2173350702453,31.7155134575413,32.2136918448374,32.7118702321334,33.2100486194295,
33.7082270067256,34.2064053940216,34.5575191894878),.UNSPECIFIED.);
#1281=B_SPLINE_CURVE_WITH_KNOTS('',3,(#51057,#51058,#51059,#51060,#51061,
#51062,#51063,#51064,#51065,#51066,#51067,#51068,#51069,#51070,#51071,#51072,
#51073),.UNSPECIFIED.,.F.,.F.,(4,1,1,1,1,1,1,1,1,1,1,1,1,1,4),(21.9911485751286,
22.0767789810357,22.5749573683318,23.0731357556278,23.5713141429239,24.06949253022,
24.567670917516,25.0658493048121,25.5640276921081,26.0622060794042,26.5603844667003,
27.0585628539963,27.5567412412924,28.0549196285885,28.2743338823082),
 .UNSPECIFIED.);
#1282=B_SPLINE_CURVE_WITH_KNOTS('',3,(#51074,#51075,#51076,#51077,#51078,
#51079,#51080,#51081,#51082,#51083,#51084,#51085,#51086,#51087,#51088,#51089,
#51090),.UNSPECIFIED.,.F.,.F.,(4,1,1,1,1,1,1,1,1,1,1,1,1,1,4),(21.9911485751286,
22.2501240989161,22.7483024862122,23.2464808735082,23.7446592608043,24.2428376481004,
24.7410160353964,25.2391944226925,25.7373728099886,26.2355511972846,26.7337295845807,
27.2319079718768,27.7300863591728,28.2282647464689,28.2743338823082),
 .UNSPECIFIED.);
#1283=B_SPLINE_CURVE_WITH_KNOTS('',3,(#51095,#51096,#51097,#51098,#51099,
#51100,#51101,#51102,#51103,#51104,#51105,#51106,#51107,#51108,#51109,#51110),
 .UNSPECIFIED.,.F.,.F.,(4,1,1,1,1,1,1,1,1,1,1,1,1,4),(15.707963267949,16.0986383334829,
16.596816720779,17.0949951080751,17.5931734953711,18.0913518826672,18.5895302699633,
19.0877086572593,19.5858870445554,20.0840654318515,20.5822438191475,21.0804222064436,
21.5786005937396,21.9911485751286),.UNSPECIFIED.);
#1284=B_SPLINE_CURVE_WITH_KNOTS('',3,(#51111,#51112,#51113,#51114,#51115,
#51116,#51117,#51118,#51119,#51120,#51121,#51122,#51123,#51124,#51125,#51126,
#51127),.UNSPECIFIED.,.F.,.F.,(4,1,1,1,1,1,1,1,1,1,1,1,1,1,4),(15.707963267949,
15.7738050640673,16.2719834513634,16.7701618386594,17.2683402259555,17.7665186132516,
18.2646970005476,18.7628753878437,19.2610537751397,19.7592321624358,20.2574105497319,
20.7555889370279,21.253767324324,21.7519457116201,21.9911485751286),
 .UNSPECIFIED.);
#1285=B_SPLINE_CURVE_WITH_KNOTS('',3,(#51130,#51131,#51132,#51133,#51134,
#51135,#51136,#51137,#51138,#51139,#51140,#51141,#51142,#51143,#51144,#51145,
#51146,#51147,#51148,#51149,#51150,#51151,#51152,#51153,#51154,#51155,#51156,
#51157,#51158,#51159,#51160,#51161,#51162,#51163,#51164,#51165,#51166,#51167,
#51168,#51169,#51170,#51171,#51172,#51173,#51174,#51175,#51176,#51177,#51178,
#51179,#51180,#51181,#51182,#51183,#51184,#51185,#51186,#51187,#51188,#51189,
#51190,#51191,#51192,#51193,#51194,#51195,#51196,#51197,#51198,#51199,#51200,
#51201,#51202),.UNSPECIFIED.,.F.,.F.,(4,3,3,3,3,3,3,3,3,3,3,3,3,3,3,3,3,
3,3,3,3,3,3,3,4),(-1.53373699248756,-1.47747305975871,-1.39029021397083,
-1.35774868938916,-1.33203786420062,-1.23038977040391,-1.19146538006595,
-1.16614143986796,-1.1287416766072,-1.02618547124656,-0.922698333606641,
-0.889977710189035,-0.867418444292481,-0.765890607100357,-0.67180537271053,
-0.617798901068506,-0.584547425353373,-0.476585692119078,-0.389549669541049,
-0.338521028541637,-0.310950996513903,-0.288719229766344,-0.179543753119938,
-0.0694757010746949,0.),.UNSPECIFIED.);
#1286=B_SPLINE_CURVE_WITH_KNOTS('',3,(#51207,#51208,#51209,#51210,#51211,
#51212,#51213,#51214,#51215,#51216,#51217,#51218,#51219,#51220,#51221,#51222,
#51223,#51224,#51225,#51226,#51227,#51228,#51229,#51230,#51231,#51232,#51233,
#51234,#51235,#51236,#51237,#51238,#51239,#51240,#51241,#51242,#51243,#51244,
#51245,#51246,#51247,#51248,#51249,#51250,#51251,#51252,#51253,#51254,#51255,
#51256,#51257,#51258,#51259,#51260,#51261,#51262,#51263,#51264,#51265,#51266,
#51267,#51268,#51269,#51270,#51271,#51272,#51273,#51274,#51275,#51276,#51277,
#51278,#51279,#51280,#51281,#51282),.UNSPECIFIED.,.F.,.F.,(4,3,3,3,3,3,
3,3,3,3,3,3,3,3,3,3,3,3,3,3,3,3,3,3,3,4),(-1.52870610664518,-1.46376476615558,
-1.36738223521408,-1.32958326055218,-1.30288468132391,-1.19055966185675,
-1.12214938319575,-1.0961569708181,-1.07823464238959,-0.971315082094603,
-0.865333221118986,-0.833428294780767,-0.811851541586676,-0.705424835001878,
-0.615550946694521,-0.567787651690986,-0.544829757697887,-0.521800305094042,
-0.419968998263115,-0.345929281772451,-0.297699082711072,-0.272424456165966,
-0.25356076098078,-0.153489816757136,-0.0552696732558858,0.),
 .UNSPECIFIED.);
#1287=B_SPLINE_CURVE_WITH_KNOTS('',3,(#52759,#52760,#52761,#52762,#52763,
#52764,#52765,#52766,#52767,#52768,#52769,#52770,#52771,#52772,#52773,#52774,
#52775,#52776,#52777,#52778,#52779,#52780),.UNSPECIFIED.,.F.,.F.,(4,3,3,
3,3,3,3,4),(177.052837307172,177.351505877399,177.849684264695,178.347862651991,
178.846041039287,179.344219426583,179.842397813879,180.258303277675),
 .UNSPECIFIED.);
#1288=B_SPLINE_CURVE_WITH_KNOTS('',3,(#52782,#52783,#52784,#52785,#52786,
#52787,#52788,#52789,#52790,#52791,#52792,#52793,#52794,#52795,#52796,#52797,
#52798,#52799,#52800,#52801,#52802,#52803,#52804,#52805,#52806,#52807,#52808,
#52809,#52810,#52811,#52812,#52813,#52814,#52815,#52816,#52817,#52818,#52819,
#52820,#52821,#52822,#52823,#52824,#52825,#52826,#52827,#52828,#52829,#52830,
#52831,#52832,#52833,#52834,#52835,#52836,#52837,#52838,#52839,#52840,#52841,
#52842,#52843,#52844,#52845,#52846,#52847,#52848,#52849,#52850,#52851,#52852,
#52853,#52854),.UNSPECIFIED.,.F.,.F.,(4,3,3,3,3,3,3,3,3,3,3,3,3,3,3,3,3,
3,3,3,3,3,3,3,4),(-1.53373699248745,-1.47747305975858,-1.39029021397072,
-1.35774869265005,-1.3320378699845,-1.23038977329582,-1.19146538262761,
-1.16614144091151,-1.12874167660715,-1.02618546806066,-0.922698329608141,
-0.889977692654673,-0.86741844172116,-0.765890607100252,-0.671805372710442,
-0.61779890472176,-0.584547424585698,-0.476585688325599,-0.389549669541011,
-0.338521026353068,-0.310950992013572,-0.28871922610837,-0.179543774302306,
-0.0694757077851898,0.),.UNSPECIFIED.);
#1289=B_SPLINE_CURVE_WITH_KNOTS('',3,(#52855,#52856,#52857,#52858,#52859,
#52860,#52861,#52862,#52863,#52864,#52865,#52866,#52867,#52868),
 .UNSPECIFIED.,.F.,.F.,(4,1,1,1,1,1,1,1,1,1,1,4),(10.3761157273103,10.7920211911067,
11.2901995784027,11.7883779656988,12.2865563529949,12.7847347402909,13.282913127587,
13.781091514883,14.2792699021791,14.7774482894752,15.2756266767712,15.707963267949),
 .UNSPECIFIED.);
#1290=B_SPLINE_CURVE_WITH_KNOTS('',3,(#52874,#52875,#52876,#52877,#52878,
#52879,#52880,#52881,#52882,#52883,#52884,#52885,#52886,#52887,#52888,#52889,
#52890,#52891,#52892,#52893,#52894,#52895,#52896,#52897,#52898,#52899,#52900,
#52901,#52902,#52903,#52904,#52905,#52906,#52907,#52908,#52909,#52910,#52911,
#52912,#52913,#52914,#52915,#52916,#52917,#52918,#52919,#52920,#52921,#52922,
#52923,#52924,#52925,#52926,#52927,#52928,#52929,#52930,#52931,#52932,#52933,
#52934,#52935,#52936,#52937,#52938,#52939,#52940,#52941,#52942,#52943,#52944,
#52945,#52946,#52947,#52948,#52949),.UNSPECIFIED.,.F.,.F.,(4,3,3,3,3,3,
3,3,3,3,3,3,3,3,3,3,3,3,3,3,3,3,3,3,3,4),(-1.52870610664516,-1.46376476615555,
-1.36738223521406,-1.32958325854658,-1.30288467919751,-1.19055966079354,
-1.12214938313862,-1.09615697088941,-1.07823464238957,-0.971315084120084,
-0.865333237336496,-0.833428218151789,-0.81185148451087,-0.705424835001883,
-0.615550946694523,-0.567787650900965,-0.544829752438311,-0.521800302803709,
-0.419968974496642,-0.345929281772446,-0.297699074379986,-0.272424429856221,
-0.253560731563668,-0.153489786788608,-0.0552696831557091,0.),
 .UNSPECIFIED.);
#1291=B_SPLINE_CURVE_WITH_KNOTS('',3,(#52952,#52953,#52954,#52955,#52956,
#52957,#52958,#52959,#52960,#52961,#52962,#52963),.UNSPECIFIED.,.F.,.F.,
(4,1,1,1,1,1,1,1,1,4),(11.6150328478184,12.1132112351144,12.6113896224105,
13.1095680097066,13.6077463970026,14.1059247842987,14.6041031715948,15.1022815588908,
15.6004599461869,15.707963267949),.UNSPECIFIED.);
#1292=B_SPLINE_CURVE_WITH_KNOTS('',3,(#54440,#54441,#54442,#54443,#54444,
#54445,#54446,#54447,#54448,#54449,#54450,#54451,#54452,#54453,#54454,#54455),
 .UNSPECIFIED.,.F.,.F.,(4,3,3,3,3,4),(-182.333289750359,-181.835111363063,
-181.336932975767,-180.838754588471,-180.340576201175,-180.022119021159),
 .UNSPECIFIED.);
#1293=B_SPLINE_CURVE_WITH_KNOTS('',3,(#54716,#54717,#54718,#54719,#54720,
#54721,#54722,#54723,#54724,#54725,#54726,#54727,#54728,#54729,#54730,#54731),
 .UNSPECIFIED.,.F.,.F.,(4,3,3,3,3,4),(-4.09293042013069,-3.98338122261878,
-3.48545856979143,-2.98753591696408,-2.48961326413674,-2.07498647268396),
 .UNSPECIFIED.);
#1294=B_SPLINE_CURVE_WITH_KNOTS('',3,(#54734,#54735,#54736,#54737,#54738,
#54739,#54740,#54741,#54742,#54743),.UNSPECIFIED.,.F.,.F.,(4,3,3,4),(0.,
0.497922652827334,0.99584530565469,1.12364870614302),.UNSPECIFIED.);
#1295=B_SPLINE_CURVE_WITH_KNOTS('',3,(#54748,#54749,#54750,#54751,#54752,
#54753,#54754,#54755,#54756,#54757,#54758,#54759,#54760,#54761,#54762,#54763,
#54764,#54765,#54766,#54767,#54768,#54769,#54770,#54771,#54772,#54773,#54774,
#54775,#54776,#54777,#54778,#54779,#54780,#54781,#54782,#54783,#54784,#54785,
#54786,#54787),.UNSPECIFIED.,.F.,.F.,(4,3,3,3,3,3,3,3,3,3,3,3,3,4),(-10.3761157273103,
-9.95845305654694,-9.46053040371959,-8.96260775089224,-8.4646850980649,
-7.96676244523755,-7.46883979241021,-6.97091713958286,-6.47299448675551,
-5.97507183392816,-5.47714918110082,-4.97922652827347,-4.48130387544612,
-4.09293042013069),.UNSPECIFIED.);
#1296=B_SPLINE_CURVE_WITH_KNOTS('',3,(#54788,#54789,#54790,#54791,#54792,
#54793,#54794,#54795,#54796,#54797,#54798,#54799,#54800,#54801,#54802,#54803,
#54804,#54805,#54806,#54807,#54808,#54809,#54810,#54811,#54812,#54813,#54814,
#54815,#54816,#54817,#54818,#54819,#54820,#54821,#54822,#54823,#54824,#54825,
#54826,#54827),.UNSPECIFIED.,.F.,.F.,(4,3,3,3,3,3,3,3,3,3,3,3,3,4),(1.12364870614302,
1.49376795848204,1.99169061130939,2.48961326413673,2.98753591696408,3.48545856979143,
3.98338122261877,4.48130387544612,4.97922652827347,5.47714918110082,5.97507183392816,
6.47299448675551,6.97091713958286,7.40683401332261),.UNSPECIFIED.);
#1297=B_SPLINE_CURVE_WITH_KNOTS('',3,(#54832,#54833,#54834,#54835,#54836,
#54837,#54838,#54839,#54840,#54841,#54842,#54843,#54844,#54845,#54846,#54847,
#54848,#54849,#54850,#54851,#54852,#54853,#54854,#54855,#54856,#54857,#54858,
#54859,#54860,#54861,#54862,#54863,#54864,#54865,#54866,#54867,#54868,#54869,
#54870,#54871,#54872,#54873,#54874),.UNSPECIFIED.,.F.,.F.,(4,3,3,3,3,3,
3,3,3,3,3,3,3,3,4),(-16.6593010344899,-16.4314475433024,-15.9335248904751,
-15.4356022376478,-14.9376795848204,-14.4397569319931,-13.9418342791657,
-13.4439116263384,-12.945988973511,-12.4480663206837,-11.9501436678563,
-11.452221015029,-10.9542983622016,-10.4563757093743,-10.3761157273103),
 .UNSPECIFIED.);
#1298=B_SPLINE_CURVE_WITH_KNOTS('',3,(#54875,#54876,#54877,#54878,#54879,
#54880,#54881,#54882,#54883,#54884,#54885,#54886,#54887,#54888,#54889,#54890,
#54891,#54892,#54893,#54894,#54895,#54896,#54897,#54898,#54899,#54900,#54901,
#54902,#54903,#54904,#54905,#54906,#54907,#54908,#54909,#54910,#54911,#54912,
#54913,#54914,#54915,#54916,#54917),.UNSPECIFIED.,.F.,.F.,(4,3,3,3,3,3,
3,3,3,3,3,3,3,3,4),(7.40683401332261,7.4688397924102,7.96676244523755,8.4646850980649,
8.96260775089224,9.46053040371959,9.95845305654694,10.4563757093743,10.9542983622016,
11.452221015029,11.9501436678563,12.4480663206837,12.945988973511,13.4439116263384,
13.6900193205022),.UNSPECIFIED.);
#1299=B_SPLINE_CURVE_WITH_KNOTS('',3,(#54922,#54923,#54924,#54925,#54926,
#54927,#54928,#54929,#54930,#54931,#54932,#54933,#54934,#54935,#54936,#54937,
#54938,#54939,#54940,#54941,#54942,#54943,#54944,#54945,#54946,#54947,#54948,
#54949,#54950,#54951,#54952,#54953,#54954,#54955,#54956,#54957,#54958,#54959,
#54960,#54961,#54962,#54963,#54964),.UNSPECIFIED.,.F.,.F.,(4,3,3,3,3,3,
3,3,3,3,3,3,3,3,4),(-22.9424863416694,-22.904442030058,-22.4065193772306,
-21.9085967244033,-21.4106740715759,-20.9127514187486,-20.4148287659212,
-19.9169061130939,-19.4189834602665,-18.9210608074392,-18.4231381546118,
-17.9252155017845,-17.4272928489571,-16.9293701961298,-16.6593010344899),
 .UNSPECIFIED.);
#1300=B_SPLINE_CURVE_WITH_KNOTS('',3,(#54965,#54966,#54967,#54968,#54969,
#54970,#54971,#54972,#54973,#54974,#54975,#54976,#54977,#54978,#54979,#54980,
#54981,#54982,#54983,#54984,#54985,#54986,#54987,#54988,#54989,#54990,#54991,
#54992,#54993,#54994,#54995,#54996,#54997,#54998,#54999,#55000,#55001,#55002,
#55003,#55004,#55005,#55006,#55007),.UNSPECIFIED.,.F.,.F.,(4,3,3,3,3,3,
3,3,3,3,3,3,3,3,4),(13.6900193205022,13.9418342791657,14.4397569319931,
14.9376795848204,15.4356022376478,15.9335248904751,16.4314475433025,16.9293701961298,
17.4272928489571,17.9252155017845,18.4231381546118,18.9210608074392,19.4189834602665,
19.9169061130939,19.9732046276818),.UNSPECIFIED.);
#1301=B_SPLINE_CURVE_WITH_KNOTS('',3,(#55012,#55013,#55014,#55015,#55016,
#55017,#55018,#55019,#55020,#55021,#55022,#55023,#55024,#55025,#55026,#55027,
#55028,#55029,#55030,#55031,#55032,#55033,#55034,#55035,#55036,#55037,#55038,
#55039,#55040,#55041,#55042,#55043,#55044,#55045,#55046,#55047,#55048,#55049,
#55050,#55051),.UNSPECIFIED.,.F.,.F.,(4,3,3,3,3,3,3,3,3,3,3,3,3,4),(-29.225671648849,
-28.8795138639861,-28.3815912111588,-27.8836685583314,-27.3857459055041,
-26.8878232526767,-26.3899005998494,-25.891977947022,-25.3940552941947,
-24.8961326413673,-24.39820998854,-23.9002873357127,-23.4023646828853,-22.9424863416694),
 .UNSPECIFIED.);
#1302=B_SPLINE_CURVE_WITH_KNOTS('',3,(#55052,#55053,#55054,#55055,#55056,
#55057,#55058,#55059,#55060,#55061,#55062,#55063,#55064,#55065,#55066,#55067,
#55068,#55069,#55070,#55071,#55072,#55073,#55074,#55075,#55076,#55077,#55078,
#55079,#55080,#55081,#55082,#55083,#55084,#55085,#55086,#55087,#55088,#55089,
#55090,#55091),.UNSPECIFIED.,.F.,.F.,(4,3,3,3,3,3,3,3,3,3,3,3,3,4),(19.9732046276818,
20.4148287659212,20.9127514187486,21.4106740715759,21.9085967244033,22.4065193772306,
22.904442030058,23.4023646828853,23.9002873357127,24.39820998854,24.8961326413673,
25.3940552941947,25.891977947022,26.2563899348614),.UNSPECIFIED.);
#1303=B_SPLINE_CURVE_WITH_KNOTS('',3,(#55096,#55097,#55098,#55099,#55100,
#55101,#55102,#55103,#55104,#55105,#55106,#55107,#55108,#55109,#55110,#55111,
#55112,#55113,#55114,#55115,#55116,#55117,#55118,#55119,#55120,#55121,#55122,
#55123,#55124,#55125,#55126,#55127,#55128,#55129,#55130,#55131,#55132,#55133,
#55134,#55135,#55136,#55137,#55138),.UNSPECIFIED.,.F.,.F.,(4,3,3,3,3,3,
3,3,3,3,3,3,3,3,4),(-35.5088569560286,-35.3525083507416,-34.8545856979143,
-34.3566630450869,-33.8587403922596,-33.3608177394322,-32.8628950866049,
-32.3649724337776,-31.8670497809502,-31.3691271281229,-30.8712044752955,
-30.3732818224682,-29.8753591696408,-29.3774365168135,-29.225671648849),
 .UNSPECIFIED.);
#1304=B_SPLINE_CURVE_WITH_KNOTS('',3,(#55139,#55140,#55141,#55142,#55143,
#55144,#55145,#55146,#55147,#55148,#55149,#55150,#55151,#55152,#55153,#55154,
#55155,#55156,#55157,#55158,#55159,#55160,#55161,#55162,#55163,#55164,#55165,
#55166,#55167,#55168,#55169,#55170,#55171,#55172,#55173,#55174,#55175,#55176,
#55177,#55178,#55179,#55180,#55181),.UNSPECIFIED.,.F.,.F.,(4,3,3,3,3,3,
3,3,3,3,3,3,3,3,4),(26.2563899348614,26.3899005998494,26.8878232526767,
27.3857459055041,27.8836685583314,28.3815912111588,28.8795138639861,29.3774365168135,
29.8753591696408,30.3732818224682,30.8712044752955,31.3691271281229,31.8670497809502,
32.3649724337775,32.5395752420409),.UNSPECIFIED.);
#1305=B_SPLINE_CURVE_WITH_KNOTS('',3,(#55186,#55187,#55188,#55189,#55190,
#55191,#55192,#55193,#55194,#55195,#55196,#55197,#55198,#55199,#55200,#55201,
#55202,#55203,#55204,#55205,#55206,#55207,#55208,#55209,#55210,#55211,#55212,
#55213,#55214,#55215,#55216,#55217,#55218,#55219,#55220,#55221,#55222,#55223,
#55224,#55225),.UNSPECIFIED.,.F.,.F.,(4,3,3,3,3,3,3,3,3,3,3,3,3,4),(-41.7920422632082,
-41.3275801846698,-40.8296575318424,-40.3317348790151,-39.8338122261878,
-39.3358895733604,-38.8379669205331,-38.3400442677057,-37.8421216148784,
-37.344198962051,-36.8462763092237,-36.3483536563963,-35.850431003569,-35.5088569560286),
 .UNSPECIFIED.);
#1306=B_SPLINE_CURVE_WITH_KNOTS('',3,(#55226,#55227,#55228,#55229,#55230,
#55231,#55232,#55233,#55234,#55235,#55236,#55237,#55238,#55239,#55240,#55241,
#55242,#55243,#55244,#55245,#55246,#55247,#55248,#55249,#55250,#55251,#55252,
#55253,#55254,#55255,#55256,#55257,#55258,#55259,#55260,#55261,#55262,#55263,
#55264,#55265),.UNSPECIFIED.,.F.,.F.,(4,3,3,3,3,3,3,3,3,3,3,3,3,4),(32.5395752420409,
32.8628950866049,33.3608177394322,33.8587403922596,34.3566630450869,34.8545856979143,
35.3525083507416,35.850431003569,36.3483536563963,36.8462763092237,37.344198962051,
37.8421216148784,38.3400442677057,38.8227605492205),.UNSPECIFIED.);
#1307=B_SPLINE_CURVE_WITH_KNOTS('',3,(#55270,#55271,#55272,#55273,#55274,
#55275,#55276,#55277,#55278,#55279,#55280,#55281,#55282,#55283,#55284,#55285,
#55286,#55287,#55288,#55289,#55290,#55291,#55292,#55293,#55294,#55295,#55296,
#55297,#55298,#55299,#55300,#55301,#55302,#55303,#55304,#55305,#55306,#55307,
#55308,#55309,#55310,#55311,#55312),.UNSPECIFIED.,.F.,.F.,(4,3,3,3,3,3,
3,3,3,3,3,3,3,3,4),(-48.0752275703878,-47.8005746714253,-47.302652018598,
-46.8047293657706,-46.3068067129433,-45.8088840601159,-45.3109614072886,
-44.8130387544612,-44.3151161016339,-43.8171934488065,-43.3192707959792,
-42.8213481431518,-42.3234254903245,-41.8255028374971,-41.7920422632082),
 .UNSPECIFIED.);
#1308=B_SPLINE_CURVE_WITH_KNOTS('',3,(#55313,#55314,#55315,#55316,#55317,
#55318,#55319,#55320,#55321,#55322,#55323,#55324,#55325,#55326,#55327,#55328,
#55329,#55330,#55331,#55332,#55333,#55334,#55335,#55336,#55337,#55338,#55339,
#55340,#55341,#55342,#55343,#55344,#55345,#55346,#55347,#55348,#55349,#55350,
#55351,#55352,#55353,#55354,#55355),.UNSPECIFIED.,.F.,.F.,(4,3,3,3,3,3,
3,3,3,3,3,3,3,3,4),(38.8227605492205,38.8379669205331,39.3358895733604,
39.8338122261878,40.3317348790151,40.8296575318425,41.3275801846698,41.8255028374971,
42.3234254903245,42.8213481431518,43.3192707959792,43.8171934488065,44.3151161016339,
44.8130387544612,45.1059458564001),.UNSPECIFIED.);
#1309=B_SPLINE_CURVE_WITH_KNOTS('',3,(#55360,#55361,#55362,#55363,#55364,
#55365,#55366,#55367,#55368,#55369,#55370,#55371,#55372,#55373,#55374,#55375,
#55376,#55377,#55378,#55379,#55380,#55381,#55382,#55383,#55384,#55385,#55386,
#55387,#55388,#55389,#55390,#55391,#55392,#55393,#55394,#55395,#55396,#55397,
#55398,#55399,#55400,#55401,#55402),.UNSPECIFIED.,.F.,.F.,(4,3,3,3,3,3,
3,3,3,3,3,3,3,3,4),(-54.3584128775674,-54.2735691581808,-53.7756465053535,
-53.2777238525261,-52.7798011996988,-52.2818785468714,-51.7839558940441,
-51.2860332412167,-50.7881105883894,-50.290187935562,-49.7922652827347,
-49.2943426299073,-48.79641997708,-48.2984973242527,-48.0752275703878),
 .UNSPECIFIED.);
#1310=B_SPLINE_CURVE_WITH_KNOTS('',3,(#55403,#55404,#55405,#55406,#55407,
#55408,#55409,#55410,#55411,#55412,#55413,#55414,#55415,#55416,#55417,#55418,
#55419,#55420,#55421,#55422,#55423,#55424,#55425,#55426,#55427,#55428,#55429,
#55430,#55431,#55432,#55433,#55434,#55435,#55436,#55437,#55438,#55439,#55440,
#55441,#55442,#55443,#55444,#55445),.UNSPECIFIED.,.F.,.F.,(4,3,3,3,3,3,
3,3,3,3,3,3,3,3,4),(45.1059458564001,45.3109614072886,45.8088840601159,
46.3068067129433,46.8047293657706,47.302652018598,47.8005746714253,48.2984973242527,
48.79641997708,49.2943426299074,49.7922652827347,50.2901879355621,50.7881105883894,
51.2860332412167,51.3891311635797),.UNSPECIFIED.);
#1311=B_SPLINE_CURVE_WITH_KNOTS('',3,(#55450,#55451,#55452,#55453,#55454,
#55455,#55456,#55457,#55458,#55459,#55460,#55461,#55462,#55463,#55464,#55465,
#55466,#55467,#55468,#55469,#55470,#55471,#55472,#55473,#55474,#55475,#55476,
#55477,#55478,#55479,#55480,#55481,#55482,#55483,#55484,#55485,#55486,#55487,
#55488,#55489),.UNSPECIFIED.,.F.,.F.,(4,3,3,3,3,3,3,3,3,3,3,3,3,4),(-60.641598184747,
-60.248640992109,-59.7507183392816,-59.2527956864543,-58.754873033627,-58.2569503807996,
-57.7590277279723,-57.2611050751449,-56.7631824223175,-56.2652597694902,
-55.7673371166629,-55.2694144638355,-54.7714918110082,-54.3584128775674),
 .UNSPECIFIED.);
#1312=B_SPLINE_CURVE_WITH_KNOTS('',3,(#55490,#55491,#55492,#55493,#55494,
#55495,#55496,#55497,#55498,#55499,#55500,#55501,#55502,#55503,#55504,#55505,
#55506,#55507,#55508,#55509,#55510,#55511,#55512,#55513,#55514,#55515,#55516,
#55517,#55518,#55519,#55520,#55521,#55522,#55523,#55524,#55525,#55526,#55527,
#55528,#55529),.UNSPECIFIED.,.F.,.F.,(4,3,3,3,3,3,3,3,3,3,3,3,3,4),(51.3891311635797,
51.7839558940441,52.2818785468714,52.7798011996988,53.2777238525261,53.7756465053535,
54.2735691581808,54.7714918110082,55.2694144638355,55.7673371166629,56.2652597694902,
56.7631824223176,57.2611050751449,57.6723164707593),.UNSPECIFIED.);
#1313=B_SPLINE_CURVE_WITH_KNOTS('',3,(#55534,#55535,#55536,#55537,#55538,
#55539,#55540,#55541,#55542,#55543,#55544,#55545,#55546,#55547,#55548,#55549,
#55550,#55551,#55552,#55553,#55554,#55555,#55556,#55557,#55558,#55559,#55560,
#55561,#55562,#55563,#55564,#55565,#55566,#55567,#55568,#55569,#55570,#55571,
#55572,#55573,#55574,#55575,#55576),.UNSPECIFIED.,.F.,.F.,(4,3,3,3,3,3,
3,3,3,3,3,3,3,3,4),(-66.9247834919266,-66.7216354788645,-66.2237128260371,
-65.7257901732098,-65.2278675203824,-64.7299448675551,-64.2320222147278,
-63.7340995619004,-63.2361769090731,-62.7382542562457,-62.2403316034184,
-61.742408950591,-61.2444862977637,-60.7465636449363,-60.641598184747),
 .UNSPECIFIED.);
#1314=B_SPLINE_CURVE_WITH_KNOTS('',3,(#55577,#55578,#55579,#55580,#55581,
#55582,#55583,#55584,#55585,#55586,#55587,#55588,#55589,#55590,#55591,#55592,
#55593,#55594,#55595,#55596,#55597,#55598,#55599,#55600,#55601,#55602,#55603,
#55604,#55605,#55606,#55607,#55608,#55609,#55610,#55611,#55612,#55613,#55614,
#55615,#55616,#55617,#55618,#55619),.UNSPECIFIED.,.F.,.F.,(4,3,3,3,3,3,
3,3,3,3,3,3,3,3,4),(57.6723164707593,57.7590277279723,58.2569503807996,
58.754873033627,59.2527956864543,59.7507183392817,60.248640992109,60.7465636449363,
61.2444862977637,61.742408950591,62.2403316034184,62.7382542562457,63.2361769090731,
63.7340995619004,63.9555017779389),.UNSPECIFIED.);
#1315=B_SPLINE_CURVE_WITH_KNOTS('',3,(#55624,#55625,#55626,#55627,#55628,
#55629,#55630,#55631,#55632,#55633,#55634,#55635,#55636,#55637,#55638,#55639,
#55640,#55641,#55642,#55643,#55644,#55645,#55646,#55647,#55648,#55649,#55650,
#55651,#55652,#55653,#55654,#55655,#55656,#55657,#55658,#55659,#55660,#55661,
#55662,#55663,#55664,#55665,#55666),.UNSPECIFIED.,.F.,.F.,(4,3,3,3,3,3,
3,3,3,3,3,3,3,3,4),(-73.2079687991062,-73.19462996562,-72.6967073127926,
-72.1987846599653,-71.700862007138,-71.2029393543106,-70.7050167014833,
-70.2070940486559,-69.7091713958286,-69.2112487430012,-68.7133260901739,
-68.2154034373465,-67.7174807845192,-67.2195581316918,-66.9247834919266),
 .UNSPECIFIED.);
#1316=B_SPLINE_CURVE_WITH_KNOTS('',3,(#55667,#55668,#55669,#55670,#55671,
#55672,#55673,#55674,#55675,#55676,#55677,#55678,#55679,#55680,#55681,#55682,
#55683,#55684,#55685,#55686,#55687,#55688,#55689,#55690,#55691,#55692,#55693,
#55694,#55695,#55696,#55697,#55698,#55699,#55700,#55701,#55702,#55703,#55704,
#55705,#55706,#55707,#55708,#55709),.UNSPECIFIED.,.F.,.F.,(4,3,3,3,3,3,
3,3,3,3,3,3,3,3,4),(63.9555017779389,64.2320222147278,64.7299448675551,
65.2278675203825,65.7257901732098,66.2237128260372,66.7216354788645,67.2195581316918,
67.7174807845192,68.2154034373465,68.7133260901739,69.2112487430012,69.7091713958286,
70.2070940486559,70.2386870851185),.UNSPECIFIED.);
#1317=B_SPLINE_CURVE_WITH_KNOTS('',3,(#55714,#55715,#55716,#55717,#55718,
#55719,#55720,#55721,#55722,#55723,#55724,#55725,#55726,#55727,#55728,#55729,
#55730,#55731,#55732,#55733,#55734,#55735,#55736,#55737,#55738,#55739,#55740,
#55741,#55742,#55743,#55744,#55745,#55746,#55747,#55748,#55749,#55750,#55751,
#55752,#55753),.UNSPECIFIED.,.F.,.F.,(4,3,3,3,3,3,3,3,3,3,3,3,3,4),(-79.4911541062858,
-79.1697017995482,-78.6717791467208,-78.1738564938935,-77.6759338410661,
-77.1780111882388,-76.6800885354114,-76.1821658825841,-75.6842432297567,
-75.1863205769294,-74.688397924102,-74.1904752712747,-73.6925526184473,
-73.2079687991062),.UNSPECIFIED.);
#1318=B_SPLINE_CURVE_WITH_KNOTS('',3,(#55754,#55755,#55756,#55757,#55758,
#55759,#55760,#55761,#55762,#55763,#55764,#55765,#55766,#55767,#55768,#55769,
#55770,#55771,#55772,#55773,#55774,#55775,#55776,#55777,#55778,#55779,#55780,
#55781,#55782,#55783,#55784,#55785,#55786,#55787,#55788,#55789,#55790,#55791,
#55792,#55793),.UNSPECIFIED.,.F.,.F.,(4,3,3,3,3,3,3,3,3,3,3,3,3,4),(70.2386870851185,
70.7050167014833,71.2029393543106,71.700862007138,72.1987846599653,72.6967073127927,
73.19462996562,73.6925526184474,74.1904752712747,74.688397924102,75.1863205769294,
75.6842432297567,76.1821658825841,76.5218723922981),.UNSPECIFIED.);
#1319=B_SPLINE_CURVE_WITH_KNOTS('',3,(#55798,#55799,#55800,#55801,#55802,
#55803,#55804,#55805,#55806,#55807,#55808,#55809,#55810,#55811,#55812,#55813,
#55814,#55815,#55816,#55817,#55818,#55819,#55820,#55821,#55822,#55823,#55824,
#55825,#55826,#55827,#55828,#55829,#55830,#55831,#55832,#55833,#55834,#55835,
#55836,#55837,#55838,#55839,#55840),.UNSPECIFIED.,.F.,.F.,(4,3,3,3,3,3,
3,3,3,3,3,3,3,3,4),(-85.7743394134654,-85.6426962863037,-85.1447736334763,
-84.646850980649,-84.1489283278216,-83.6510056749943,-83.153083022167,-82.6551603693396,
-82.1572377165122,-81.6593150636849,-81.1613924108575,-80.6634697580302,
-80.1655471052028,-79.6676244523755,-79.4911541062858),.UNSPECIFIED.);
#1320=B_SPLINE_CURVE_WITH_KNOTS('',3,(#55841,#55842,#55843,#55844,#55845,
#55846,#55847,#55848,#55849,#55850,#55851,#55852,#55853,#55854,#55855,#55856,
#55857,#55858,#55859,#55860,#55861,#55862,#55863,#55864,#55865,#55866,#55867,
#55868,#55869,#55870,#55871,#55872,#55873,#55874,#55875,#55876,#55877,#55878,
#55879,#55880,#55881,#55882,#55883),.UNSPECIFIED.,.F.,.F.,(4,3,3,3,3,3,
3,3,3,3,3,3,3,3,4),(76.5218723922981,76.6800885354114,77.1780111882388,
77.6759338410661,78.1738564938935,78.6717791467208,79.1697017995482,79.6676244523755,
80.1655471052028,80.6634697580302,81.1613924108576,81.6593150636849,82.1572377165122,
82.6551603693396,82.8050576994777),.UNSPECIFIED.);
#1321=B_SPLINE_CURVE_WITH_KNOTS('',3,(#55888,#55889,#55890,#55891,#55892,
#55893,#55894,#55895,#55896,#55897,#55898,#55899,#55900,#55901,#55902,#55903,
#55904,#55905,#55906,#55907,#55908,#55909,#55910,#55911,#55912,#55913,#55914,
#55915,#55916,#55917,#55918,#55919,#55920,#55921,#55922,#55923,#55924,#55925,
#55926,#55927),.UNSPECIFIED.,.F.,.F.,(4,3,3,3,3,3,3,3,3,3,3,3,3,4),(-92.057524720645,
-91.6177681202318,-91.1198454674045,-90.6219228145771,-90.1240001617498,
-89.6260775089224,-89.1281548560951,-88.6302322032678,-88.1323095504404,
-87.6343868976131,-87.1364642447857,-86.6385415919584,-86.140618939131,
-85.7743394134654),.UNSPECIFIED.);
#1322=B_SPLINE_CURVE_WITH_KNOTS('',3,(#55928,#55929,#55930,#55931,#55932,
#55933,#55934,#55935,#55936,#55937,#55938,#55939,#55940,#55941,#55942,#55943,
#55944,#55945,#55946,#55947,#55948,#55949,#55950,#55951,#55952,#55953,#55954,
#55955,#55956,#55957,#55958,#55959,#55960,#55961,#55962,#55963,#55964,#55965,
#55966,#55967),.UNSPECIFIED.,.F.,.F.,(4,3,3,3,3,3,3,3,3,3,3,3,3,4),(82.8050576994777,
83.1530830221669,83.6510056749943,84.1489283278216,84.646850980649,85.1447736334763,
85.6426962863037,86.140618939131,86.6385415919584,87.1364642447857,87.6343868976131,
88.1323095504404,88.6302322032678,89.0882430066573),.UNSPECIFIED.);
#1323=B_SPLINE_CURVE_WITH_KNOTS('',3,(#55972,#55973,#55974,#55975,#55976,
#55977,#55978,#55979,#55980,#55981,#55982,#55983,#55984,#55985,#55986,#55987,
#55988,#55989,#55990,#55991,#55992,#55993,#55994,#55995,#55996,#55997,#55998,
#55999,#56000,#56001,#56002,#56003,#56004,#56005,#56006,#56007,#56008,#56009,
#56010,#56011,#56012,#56013,#56014),.UNSPECIFIED.,.F.,.F.,(4,3,3,3,3,3,
3,3,3,3,3,3,3,3,4),(-98.3407100278245,-98.0907626069873,-97.59283995416,
-97.0949173013326,-96.5969946485053,-96.099071995678,-95.6011493428506,
-95.1032266900232,-94.6053040371959,-94.1073813843686,-93.6094587315412,
-93.1115360787139,-92.6136134258865,-92.1156907730592,-92.057524720645),
 .UNSPECIFIED.);
#1324=B_SPLINE_CURVE_WITH_KNOTS('',3,(#56015,#56016,#56017,#56018,#56019,
#56020,#56021,#56022,#56023,#56024,#56025,#56026,#56027,#56028,#56029,#56030,
#56031,#56032,#56033,#56034,#56035,#56036,#56037,#56038,#56039,#56040,#56041,
#56042,#56043,#56044,#56045,#56046,#56047,#56048,#56049,#56050,#56051,#56052,
#56053,#56054,#56055,#56056,#56057),.UNSPECIFIED.,.F.,.F.,(4,3,3,3,3,3,
3,3,3,3,3,3,3,3,4),(89.0882430066573,89.1281548560951,89.6260775089225,
90.1240001617498,90.6219228145772,91.1198454674045,91.6177681202318,92.1156907730592,
92.6136134258865,93.1115360787139,93.6094587315412,94.1073813843686,94.6053040371959,
95.1032266900233,95.3714283138369),.UNSPECIFIED.);
#1325=B_SPLINE_CURVE_WITH_KNOTS('',3,(#56062,#56063,#56064,#56065,#56066,
#56067,#56068,#56069,#56070,#56071,#56072,#56073,#56074,#56075,#56076,#56077,
#56078,#56079,#56080,#56081,#56082,#56083,#56084,#56085,#56086,#56087,#56088,
#56089,#56090,#56091,#56092,#56093,#56094,#56095,#56096,#56097,#56098,#56099,
#56100,#56101,#56102,#56103,#56104),.UNSPECIFIED.,.F.,.F.,(4,3,3,3,3,3,
3,3,3,3,3,3,3,3,4),(-104.623895335004,-104.563757093743,-104.065834440916,
-103.567911788088,-103.069989135261,-102.572066482433,-102.074143829606,
-101.576221176779,-101.078298523951,-100.580375871124,-100.082453218297,
-99.5845305654694,-99.086607912642,-98.5886852598147,-98.3407100278245),
 .UNSPECIFIED.);
#1326=B_SPLINE_CURVE_WITH_KNOTS('',3,(#56105,#56106,#56107,#56108,#56109,
#56110,#56111,#56112,#56113,#56114,#56115,#56116,#56117,#56118,#56119,#56120,
#56121,#56122,#56123,#56124,#56125,#56126,#56127,#56128,#56129,#56130,#56131,
#56132,#56133,#56134,#56135,#56136,#56137,#56138,#56139,#56140,#56141,#56142,
#56143,#56144,#56145,#56146,#56147),.UNSPECIFIED.,.F.,.F.,(4,3,3,3,3,3,
3,3,3,3,3,3,3,3,4),(95.3714283138369,95.6011493428506,96.099071995678,96.5969946485053,
97.0949173013327,97.59283995416,98.0907626069874,98.5886852598147,99.0866079126421,
99.5845305654694,100.082453218297,100.580375871124,101.078298523951,101.576221176779,
101.654613621016),.UNSPECIFIED.);
#1327=B_SPLINE_CURVE_WITH_KNOTS('',3,(#56152,#56153,#56154,#56155,#56156,
#56157,#56158,#56159,#56160,#56161,#56162,#56163,#56164,#56165,#56166,#56167,
#56168,#56169,#56170,#56171,#56172,#56173,#56174,#56175,#56176,#56177,#56178,
#56179,#56180,#56181,#56182,#56183,#56184,#56185,#56186,#56187,#56188,#56189,
#56190,#56191),.UNSPECIFIED.,.F.,.F.,(4,3,3,3,3,3,3,3,3,3,3,3,3,4),(-110.907080642184,
-110.538828927671,-110.040906274844,-109.542983622016,-109.045060969189,
-108.547138316362,-108.049215663534,-107.551293010707,-107.05337035788,
-106.555447705052,-106.057525052225,-105.559602399398,-105.06167974657,
-104.623895335004),.UNSPECIFIED.);
#1328=B_SPLINE_CURVE_WITH_KNOTS('',3,(#56192,#56193,#56194,#56195,#56196,
#56197,#56198,#56199,#56200,#56201,#56202,#56203,#56204,#56205,#56206,#56207,
#56208,#56209,#56210,#56211,#56212,#56213,#56214,#56215,#56216,#56217,#56218,
#56219,#56220,#56221,#56222,#56223,#56224,#56225,#56226,#56227,#56228,#56229,
#56230,#56231),.UNSPECIFIED.,.F.,.F.,(4,3,3,3,3,3,3,3,3,3,3,3,3,4),(101.654613621016,
102.074143829606,102.572066482433,103.069989135261,103.567911788088,104.065834440916,
104.563757093743,105.06167974657,105.559602399398,106.057525052225,106.555447705052,
107.05337035788,107.551293010707,107.937798928196),.UNSPECIFIED.);
#1329=B_SPLINE_CURVE_WITH_KNOTS('',3,(#56236,#56237,#56238,#56239,#56240,
#56241,#56242,#56243,#56244,#56245,#56246,#56247,#56248,#56249,#56250,#56251,
#56252,#56253,#56254,#56255,#56256,#56257,#56258,#56259,#56260,#56261,#56262,
#56263,#56264,#56265,#56266,#56267,#56268,#56269,#56270,#56271,#56272,#56273,
#56274,#56275,#56276,#56277,#56278),.UNSPECIFIED.,.F.,.F.,(4,3,3,3,3,3,
3,3,3,3,3,3,3,3,4),(-117.190265949363,-117.011823414427,-116.513900761599,
-116.015978108772,-115.518055455944,-115.020132803117,-114.52221015029,
-114.024287497462,-113.526364844635,-113.028442191808,-112.53051953898,
-112.032596886153,-111.534674233326,-111.036751580498,-110.907080642184),
 .UNSPECIFIED.);
#1330=B_SPLINE_CURVE_WITH_KNOTS('',3,(#56279,#56280,#56281,#56282,#56283,
#56284,#56285,#56286,#56287,#56288,#56289,#56290,#56291,#56292,#56293,#56294,
#56295,#56296,#56297,#56298,#56299,#56300,#56301,#56302,#56303,#56304,#56305,
#56306,#56307,#56308,#56309,#56310,#56311,#56312,#56313,#56314,#56315,#56316,
#56317,#56318,#56319,#56320,#56321),.UNSPECIFIED.,.F.,.F.,(4,3,3,3,3,3,
3,3,3,3,3,3,3,3,4),(107.937798928196,108.049215663534,108.547138316362,
109.045060969189,109.542983622016,110.040906274844,110.538828927671,111.036751580498,
111.534674233326,112.032596886153,112.53051953898,113.028442191808,113.526364844635,
114.024287497462,114.220984235376),.UNSPECIFIED.);
#1331=B_SPLINE_CURVE_WITH_KNOTS('',3,(#56327,#56328,#56329,#56330),
 .UNSPECIFIED.,.F.,.F.,(4,4),(128.805298797182,129.041483053697),
 .UNSPECIFIED.);
#1332=B_SPLINE_CURVE_WITH_KNOTS('',3,(#56336,#56337,#56338,#56339,#56340,
#56341,#56342,#56343,#56344,#56345,#56346,#56347,#56348,#56349,#56350,#56351,
#56352),.UNSPECIFIED.,.F.,.F.,(4,1,1,1,1,1,1,1,1,1,1,1,1,1,4),(122.522113490002,
122.651784428317,123.149707081144,123.647629733971,124.145552386799,124.643475039626,
125.141397692453,125.639320345281,126.137242998108,126.635165650935,127.133088303763,
127.63101095659,128.128933609417,128.626856262245,128.805298797182),
 .UNSPECIFIED.);
#1333=B_SPLINE_CURVE_WITH_KNOTS('',3,(#56355,#56356,#56357,#56358,#56359,
#56360,#56361,#56362,#56363,#56364,#56365,#56366,#56367,#56368),
 .UNSPECIFIED.,.F.,.F.,(4,1,1,1,1,1,1,1,1,1,1,4),(122.522113490002,122.823339404916,
123.321262057743,123.819184710571,124.317107363398,124.815030016225,125.312952669053,
125.81087532188,126.308797974707,126.806720627535,127.304643280362,127.802565933189),
 .UNSPECIFIED.);
#1334=B_SPLINE_CURVE_WITH_KNOTS('',3,(#56373,#56374,#56375,#56376,#56377,
#56378,#56379,#56380,#56381,#56382,#56383,#56384,#56385,#56386,#56387,#56388),
 .UNSPECIFIED.,.F.,.F.,(4,1,1,1,1,1,1,1,1,1,1,1,1,4),(116.238928182822,
116.676712594388,117.174635247216,117.672557900043,118.17048055287,118.668403205698,
119.166325858525,119.664248511352,120.16217116418,120.660093817007,121.158016469834,
121.655939122662,122.153861775489,122.522113490002),.UNSPECIFIED.);
#1335=B_SPLINE_CURVE_WITH_KNOTS('',3,(#56389,#56390,#56391,#56392,#56393,
#56394,#56395,#56396,#56397,#56398,#56399,#56400,#56401,#56402,#56403,#56404,
#56405),.UNSPECIFIED.,.F.,.F.,(4,1,1,1,1,1,1,1,1,1,1,1,1,1,4),(116.238928182822,
116.35034491816,116.848267570988,117.346190223815,117.844112876642,118.34203552947,
118.839958182297,119.337880835125,119.835803487952,120.333726140779,120.831648793607,
121.329571446434,121.827494099261,122.325416752089,122.522113490002),
 .UNSPECIFIED.);
#1336=B_SPLINE_CURVE_WITH_KNOTS('',3,(#56410,#56411,#56412,#56413,#56414,
#56415,#56416,#56417,#56418,#56419,#56420,#56421,#56422,#56423,#56424,#56425,
#56426),.UNSPECIFIED.,.F.,.F.,(4,1,1,1,1,1,1,1,1,1,1,1,1,1,4),(109.955742875643,
110.203718107633,110.70164076046,111.199563413288,111.697486066115,112.195408718942,
112.69333137177,113.191254024597,113.689176677424,114.187099330252,114.685021983079,
115.182944635906,115.680867288734,116.178789941561,116.238928182822),
 .UNSPECIFIED.);
#1337=B_SPLINE_CURVE_WITH_KNOTS('',3,(#56427,#56428,#56429,#56430,#56431,
#56432,#56433,#56434,#56435,#56436,#56437,#56438,#56439,#56440,#56441,#56442),
 .UNSPECIFIED.,.F.,.F.,(4,1,1,1,1,1,1,1,1,1,1,1,1,4),(109.955742875643,
110.375273084232,110.87319573706,111.371118389887,111.869041042714,112.366963695542,
112.864886348369,113.362809001196,113.860731654024,114.358654306851,114.856576959678,
115.354499612506,115.852422265333,116.238928182822),.UNSPECIFIED.);
#1338=B_SPLINE_CURVE_WITH_KNOTS('',3,(#56447,#56448,#56449,#56450,#56451,
#56452,#56453,#56454,#56455,#56456,#56457,#56458,#56459,#56460,#56461,#56462,
#56463),.UNSPECIFIED.,.F.,.F.,(4,1,1,1,1,1,1,1,1,1,1,1,1,1,4),(103.672557568463,
103.730723620877,104.228646273705,104.726568926532,105.224491579359,105.722414232187,
106.220336885014,106.718259537841,107.216182190669,107.714104843496,108.212027496323,
108.709950149151,109.207872801978,109.705795454805,109.955742875643),
 .UNSPECIFIED.);
#1339=B_SPLINE_CURVE_WITH_KNOTS('',3,(#56464,#56465,#56466,#56467,#56468,
#56469,#56470,#56471,#56472,#56473,#56474,#56475,#56476,#56477,#56478,#56479,
#56480),.UNSPECIFIED.,.F.,.F.,(4,1,1,1,1,1,1,1,1,1,1,1,1,1,4),(103.672557568463,
103.902278597477,104.400201250304,104.898123903131,105.396046555959,105.893969208786,
106.391891861613,106.889814514441,107.387737167268,107.885659820096,108.383582472923,
108.88150512575,109.379427778578,109.877350431405,109.955742875643),
 .UNSPECIFIED.);
#1340=B_SPLINE_CURVE_WITH_KNOTS('',3,(#56485,#56486,#56487,#56488,#56489,
#56490,#56491,#56492,#56493,#56494,#56495,#56496,#56497,#56498,#56499,#56500),
 .UNSPECIFIED.,.F.,.F.,(4,1,1,1,1,1,1,1,1,1,1,1,1,4),(97.3893722612835,
97.7556517869492,98.2535744397765,98.7514970926039,99.2494197454312,99.7473423982586,
100.245265051086,100.743187703913,101.241110356741,101.739033009568,102.236955662395,
102.734878315223,103.23280096805,103.672557568463),.UNSPECIFIED.);
#1341=B_SPLINE_CURVE_WITH_KNOTS('',3,(#56501,#56502,#56503,#56504,#56505,
#56506,#56507,#56508,#56509,#56510,#56511,#56512,#56513,#56514,#56515,#56516,
#56517),.UNSPECIFIED.,.F.,.F.,(4,1,1,1,1,1,1,1,1,1,1,1,1,1,4),(97.3893722612835,
97.4292841107213,97.9272067635486,98.4251294163759,98.9230520692033,99.4209747220306,
99.918897374858,100.416820027685,100.914742680513,101.41266533334,101.910587986167,
102.408510638995,102.906433291822,103.404355944649,103.672557568463),
 .UNSPECIFIED.);
#1342=B_SPLINE_CURVE_WITH_KNOTS('',3,(#56522,#56523,#56524,#56525,#56526,
#56527,#56528,#56529,#56530,#56531,#56532,#56533,#56534,#56535,#56536,#56537,
#56538),.UNSPECIFIED.,.F.,.F.,(4,1,1,1,1,1,1,1,1,1,1,1,1,1,4),(91.106186954104,
91.2826573001937,91.780579953021,92.2785026058484,92.7764252586757,93.2743479115031,
93.7722705643304,94.2701932171578,94.7681158699851,95.2660385228125,95.7639611756398,
96.2618838284671,96.7598064812945,97.2577291341218,97.3893722612835),
 .UNSPECIFIED.);
#1343=B_SPLINE_CURVE_WITH_KNOTS('',3,(#56539,#56540,#56541,#56542,#56543,
#56544,#56545,#56546,#56547,#56548,#56549,#56550,#56551,#56552,#56553,#56554),
 .UNSPECIFIED.,.F.,.F.,(4,1,1,1,1,1,1,1,1,1,1,1,1,4),(91.106186954104,91.4542122767931,
91.9521349296204,92.4500575824478,92.9479802352751,93.4459028881025,93.9438255409298,
94.4417481937572,94.9396708465845,95.4375934994119,95.9355161522392,96.4334388050665,
96.9313614578939,97.3893722612835),.UNSPECIFIED.);
#1344=B_SPLINE_CURVE_WITH_KNOTS('',3,(#56559,#56560,#56561,#56562,#56563,
#56564,#56565,#56566,#56567,#56568,#56569,#56570,#56571,#56572,#56573,#56574),
 .UNSPECIFIED.,.F.,.F.,(4,1,1,1,1,1,1,1,1,1,1,1,1,4),(84.8230016469244,
85.3075854662655,85.8055081190928,86.3034307719202,86.8013534247476,87.2992760775749,
87.7971987304022,88.2951213832296,88.7930440360569,89.2909666888843,89.7888893417116,
90.286811994539,90.7847346473663,91.106186954104),.UNSPECIFIED.);
#1345=B_SPLINE_CURVE_WITH_KNOTS('',3,(#56575,#56576,#56577,#56578,#56579,
#56580,#56581,#56582,#56583,#56584,#56585,#56586,#56587,#56588,#56589,#56590,
#56591),.UNSPECIFIED.,.F.,.F.,(4,1,1,1,1,1,1,1,1,1,1,1,1,1,4),(84.8230016469244,
84.9812177900376,85.4791404428649,85.9770630956923,86.4749857485196,86.972908401347,
87.4708310541743,87.9687537070017,88.466676359829,88.9645990126564,89.4625216654837,
89.960444318311,90.4583669711384,90.9562896239657,91.106186954104),
 .UNSPECIFIED.);
#1346=B_SPLINE_CURVE_WITH_KNOTS('',3,(#56596,#56597,#56598,#56599,#56600,
#56601,#56602,#56603,#56604,#56605,#56606,#56607,#56608,#56609,#56610,#56611,
#56612),.UNSPECIFIED.,.F.,.F.,(4,1,1,1,1,1,1,1,1,1,1,1,1,1,4),(78.5398163397448,
78.83459097951,79.3325136323374,79.8304362851647,80.328358937992,80.8262815908194,
81.3242042436467,81.8221268964741,82.3200495493014,82.8179722021288,83.3158948549561,
83.8138175077835,84.3117401606108,84.8096628134382,84.8230016469244),
 .UNSPECIFIED.);
#1347=B_SPLINE_CURVE_WITH_KNOTS('',3,(#56613,#56614,#56615,#56616,#56617,
#56618,#56619,#56620,#56621,#56622,#56623,#56624,#56625,#56626,#56627,#56628),
 .UNSPECIFIED.,.F.,.F.,(4,1,1,1,1,1,1,1,1,1,1,1,1,4),(78.5398163397448,
79.0061459561094,79.5040686089368,80.0019912617641,80.4999139145914,80.9978365674188,
81.4957592202462,81.9936818730735,82.4916045259008,82.9895271787282,83.4874498315555,
83.9853724843829,84.4832951372102,84.8230016469244),.UNSPECIFIED.);
#1348=B_SPLINE_CURVE_WITH_KNOTS('',3,(#56633,#56634,#56635,#56636,#56637,
#56638,#56639,#56640,#56641,#56642,#56643,#56644,#56645,#56646,#56647,#56648,
#56649),.UNSPECIFIED.,.F.,.F.,(4,1,1,1,1,1,1,1,1,1,1,1,1,1,4),(72.2566310325652,
72.3615964927545,72.8595191455818,73.3574417984092,73.8553644512365,74.3532871040639,
74.8512097568912,75.3491324097186,75.8470550625459,76.3449777153733,76.8429003682006,
77.340823021028,77.8387456738553,78.3366683266827,78.5398163397448),
 .UNSPECIFIED.);
#1349=B_SPLINE_CURVE_WITH_KNOTS('',3,(#56650,#56651,#56652,#56653,#56654,
#56655,#56656,#56657,#56658,#56659,#56660,#56661,#56662,#56663,#56664,#56665,
#56666),.UNSPECIFIED.,.F.,.F.,(4,1,1,1,1,1,1,1,1,1,1,1,1,1,4),(72.2566310325652,
72.5331514693539,73.0310741221813,73.5289967750086,74.0269194278359,74.5248420806633,
75.0227647334906,75.520687386318,76.0186100391453,76.5165326919727,77.0144553448,
77.5123779976274,78.0103006504547,78.5082233032821,78.5398163397448),
 .UNSPECIFIED.);
#1350=B_SPLINE_CURVE_WITH_KNOTS('',3,(#56671,#56672,#56673,#56674,#56675,
#56676,#56677,#56678,#56679,#56680,#56681,#56682,#56683,#56684,#56685,#56686),
 .UNSPECIFIED.,.F.,.F.,(4,1,1,1,1,1,1,1,1,1,1,1,1,4),(65.9734457253856,
66.3865246588263,66.8844473116537,67.382369964481,67.8802926173084,68.3782152701357,
68.8761379229631,69.3740605757904,69.8719832286178,70.3699058814451,70.8678285342725,
71.3657511870998,71.8636738399271,72.2566310325652),.UNSPECIFIED.);
#1351=B_SPLINE_CURVE_WITH_KNOTS('',3,(#56687,#56688,#56689,#56690,#56691,
#56692,#56693,#56694,#56695,#56696,#56697,#56698,#56699,#56700,#56701,#56702,
#56703),.UNSPECIFIED.,.F.,.F.,(4,1,1,1,1,1,1,1,1,1,1,1,1,1,4),(65.9734457253856,
66.0601569825984,66.5580796354257,67.0560022882531,67.5539249410804,68.0518475939078,
68.5497702467351,69.0476928995625,69.5456155523898,70.0435382052172,70.5414608580445,
71.0393835108719,71.5373061636992,72.0352288165266,72.2566310325652),
 .UNSPECIFIED.);
#1352=B_SPLINE_CURVE_WITH_KNOTS('',3,(#56708,#56709,#56710,#56711,#56712,
#56713,#56714,#56715,#56716,#56717,#56718,#56719,#56720,#56721,#56722,#56723,
#56724),.UNSPECIFIED.,.F.,.F.,(4,1,1,1,1,1,1,1,1,1,1,1,1,1,4),(59.690260418206,
59.9135301720708,60.4114528248982,60.9093754777255,61.4072981305529,61.9052207833802,
62.4031434362076,62.9010660890349,63.3989887418622,63.8969113946896,64.3948340475169,
64.8927567003443,65.3906793531716,65.888602005999,65.9734457253856),
 .UNSPECIFIED.);
#1353=B_SPLINE_CURVE_WITH_KNOTS('',3,(#56725,#56726,#56727,#56728,#56729,
#56730,#56731,#56732,#56733,#56734,#56735,#56736,#56737,#56738,#56739,#56740),
 .UNSPECIFIED.,.F.,.F.,(4,1,1,1,1,1,1,1,1,1,1,1,1,4),(59.690260418206,60.0850851486702,
60.5830078014976,61.0809304543249,61.5788531071523,62.0767757599796,62.574698412807,
63.0726210656343,63.5705437184617,64.068466371289,64.5663890241163,65.0643116769437,
65.562234329771,65.9734457253856),.UNSPECIFIED.);
#1354=B_SPLINE_CURVE_WITH_KNOTS('',3,(#56745,#56746,#56747,#56748,#56749,
#56750,#56751,#56752,#56753,#56754,#56755,#56756,#56757,#56758,#56759,#56760,
#56761),.UNSPECIFIED.,.F.,.F.,(4,1,1,1,1,1,1,1,1,1,1,1,1,1,4),(53.4070751110264,
53.4405356853153,53.9384583381427,54.43638099097,54.9343036437973,55.4322262966247,
55.930148949452,56.4280716022794,56.9259942551067,57.4239169079341,57.9218395607614,
58.4197622135888,58.9176848664161,59.4156075192435,59.690260418206),
 .UNSPECIFIED.);
#1355=B_SPLINE_CURVE_WITH_KNOTS('',3,(#56762,#56763,#56764,#56765,#56766,
#56767,#56768,#56769,#56770,#56771,#56772,#56773,#56774,#56775,#56776,#56777,
#56778),.UNSPECIFIED.,.F.,.F.,(4,1,1,1,1,1,1,1,1,1,1,1,1,1,4),(53.4070751110264,
53.6120906619147,54.1100133147421,54.6079359675694,55.1058586203968,55.6037812732241,
56.1017039260515,56.5996265788788,57.0975492317061,57.5954718845335,58.0933945373608,
58.5913171901882,59.0892398430155,59.5871624958429,59.690260418206),
 .UNSPECIFIED.);
#1356=B_SPLINE_CURVE_WITH_KNOTS('',3,(#56783,#56784,#56785,#56786,#56787,
#56788,#56789,#56790,#56791,#56792,#56793,#56794,#56795,#56796,#56797,#56798),
 .UNSPECIFIED.,.F.,.F.,(4,1,1,1,1,1,1,1,1,1,1,1,1,4),(47.1238898038468,
47.4654638513871,47.9633865042145,48.4613091570418,48.9592318098692,49.4571544626965,
49.9550771155239,50.4529997683512,50.9509224211786,51.4488450740059,51.9467677268333,
52.4446903796606,52.942613032488,53.4070751110264),.UNSPECIFIED.);
#1357=B_SPLINE_CURVE_WITH_KNOTS('',3,(#56799,#56800,#56801,#56802,#56803,
#56804,#56805,#56806,#56807,#56808,#56809,#56810,#56811,#56812,#56813,#56814,
#56815),.UNSPECIFIED.,.F.,.F.,(4,1,1,1,1,1,1,1,1,1,1,1,1,1,4),(47.1238898038468,
47.1390961751592,47.6370188279866,48.1349414808139,48.6328641336412,49.1307867864686,
49.6287094392959,50.1266320921233,50.6245547449506,51.122477397778,51.6204000506053,
52.1183227034327,52.61624535626,53.1141680090874,53.4070751110264),
 .UNSPECIFIED.);
#1358=B_SPLINE_CURVE_WITH_KNOTS('',3,(#56820,#56821,#56822,#56823,#56824,
#56825,#56826,#56827,#56828,#56829,#56830,#56831,#56832,#56833,#56834,#56835,
#56836),.UNSPECIFIED.,.F.,.F.,(4,1,1,1,1,1,1,1,1,1,1,1,1,1,4),(40.8407044966672,
40.9924693646316,41.490392017459,41.9883146702863,42.4862373231137,42.984159975941,
43.4820826287684,43.9800052815957,44.4779279344231,44.9758505872504,45.4737732400778,
45.9716958929051,46.4696185457325,46.9675411985598,47.1238898038468),
 .UNSPECIFIED.);
#1359=B_SPLINE_CURVE_WITH_KNOTS('',3,(#56837,#56838,#56839,#56840,#56841,
#56842,#56843,#56844,#56845,#56846,#56847,#56848,#56849,#56850,#56851,#56852),
 .UNSPECIFIED.,.F.,.F.,(4,1,1,1,1,1,1,1,1,1,1,1,1,4),(40.8407044966672,
41.164024341231,41.6619469940584,42.1598696468857,42.6577922997131,43.1557149525404,
43.6536376053678,44.1515602581951,44.6494829110225,45.1474055638498,45.6453282166772,
46.1432508695045,46.6411735223319,47.1238898038468),.UNSPECIFIED.);
#1360=B_SPLINE_CURVE_WITH_KNOTS('',3,(#56857,#56858,#56859,#56860,#56861,
#56862,#56863,#56864,#56865,#56866,#56867,#56868,#56869,#56870,#56871,#56872),
 .UNSPECIFIED.,.F.,.F.,(4,1,1,1,1,1,1,1,1,1,1,1,1,4),(34.5575191894876,
35.0173975307035,35.5153201835308,36.0132428363582,36.5111654891855,37.0090881420129,
37.5070107948402,38.0049334476676,38.5028561004949,39.0007787533223,39.4987014061496,
39.9966240589769,40.4945467118043,40.8407044966672),.UNSPECIFIED.);
#1361=B_SPLINE_CURVE_WITH_KNOTS('',3,(#56873,#56874,#56875,#56876,#56877,
#56878,#56879,#56880,#56881,#56882,#56883,#56884,#56885,#56886,#56887,#56888,
#56889),.UNSPECIFIED.,.F.,.F.,(4,1,1,1,1,1,1,1,1,1,1,1,1,1,4),(34.5575191894876,
34.6910298544755,35.1889525073029,35.6868751601302,36.1847978129576,36.6827204657849,
37.1806431186123,37.6785657714396,38.176488424267,38.6744110770943,39.1723337299217,
39.670256382749,40.1681790355763,40.6661016884037,40.8407044966672),
 .UNSPECIFIED.);
#1362=B_SPLINE_CURVE_WITH_KNOTS('',3,(#56894,#56895,#56896,#56897,#56898,
#56899,#56900,#56901,#56902,#56903,#56904,#56905,#56906,#56907,#56908,#56909,
#56910),.UNSPECIFIED.,.F.,.F.,(4,1,1,1,1,1,1,1,1,1,1,1,1,1,4),(28.274333882308,
28.544403043948,29.0423256967753,29.5402483496027,30.03817100243,30.5360936552574,
31.0340163080847,31.5319389609121,32.0298616137394,32.5277842665667,33.0257069193941,
33.5236295722214,34.0215522250488,34.5194748778761,34.5575191894876),
 .UNSPECIFIED.);
#1363=B_SPLINE_CURVE_WITH_KNOTS('',3,(#56911,#56912,#56913,#56914,#56915,
#56916,#56917,#56918,#56919,#56920,#56921,#56922,#56923,#56924,#56925,#56926),
 .UNSPECIFIED.,.F.,.F.,(4,1,1,1,1,1,1,1,1,1,1,1,1,4),(28.274333882308,28.7159580205474,
29.2138806733747,29.7118033262021,30.2097259790294,30.7076486318568,31.2055712846841,
31.7034939375114,32.2014165903388,32.6993392431661,33.1972618959935,33.6951845488208,
34.1931072016482,34.5575191894876),.UNSPECIFIED.);
#1364=B_SPLINE_CURVE_WITH_KNOTS('',3,(#56931,#56932,#56933,#56934,#56935,
#56936,#56937,#56938,#56939,#56940,#56941,#56942,#56943,#56944,#56945,#56946,
#56947),.UNSPECIFIED.,.F.,.F.,(4,1,1,1,1,1,1,1,1,1,1,1,1,1,4),(21.9911485751285,
22.0714085571925,22.5693312100198,23.0672538628472,23.5651765156745,24.0630991685018,
24.5610218213292,25.0589444741565,25.5568671269839,26.0547897798112,26.5527124326386,
27.0506350854659,27.5485577382933,28.0464803911206,28.274333882308),
 .UNSPECIFIED.);
#1365=B_SPLINE_CURVE_WITH_KNOTS('',3,(#56948,#56949,#56950,#56951,#56952,
#56953,#56954,#56955,#56956,#56957,#56958,#56959,#56960,#56961,#56962,#56963,
#56964),.UNSPECIFIED.,.F.,.F.,(4,1,1,1,1,1,1,1,1,1,1,1,1,1,4),(21.9911485751284,
22.2429635337919,22.7408861866192,23.2388088394466,23.7367314922739,24.2346541451012,
24.7325767979286,25.2304994507559,25.7284221035833,26.2263447564106,26.724267409238,
27.2221900620653,27.7201127148927,28.21803536772,28.274333882308),
 .UNSPECIFIED.);
#1366=B_SPLINE_CURVE_WITH_KNOTS('',3,(#56969,#56970,#56971,#56972,#56973,
#56974,#56975,#56976,#56977,#56978,#56979,#56980,#56981,#56982,#56983,#56984),
 .UNSPECIFIED.,.F.,.F.,(4,1,1,1,1,1,1,1,1,1,1,1,1,4),(15.7079632679489,
16.0963367232643,16.5942593760916,17.092182028919,17.5901046817463,18.0880273345737,
18.585949987401,19.0838726402284,19.5817952930557,20.0797179458831,20.5776405987104,
21.0755632515378,21.5734859043651,21.9911485751285),.UNSPECIFIED.);
#1367=B_SPLINE_CURVE_WITH_KNOTS('',3,(#56985,#56986,#56987,#56988,#56989,
#56990,#56991,#56992,#56993,#56994,#56995,#56996,#56997,#56998,#56999,#57000,
#57001),.UNSPECIFIED.,.F.,.F.,(4,1,1,1,1,1,1,1,1,1,1,1,1,1,4),(15.7079632679489,
15.7699690470363,16.2678916998637,16.765814352691,17.2637370055184,17.7616596583457,
18.2595823111731,18.7575049640004,19.2554276168278,19.7533502696551,20.2512729224825,
20.7491955753098,21.2471182281372,21.7450408809645,21.9911485751284),
 .UNSPECIFIED.);
#1368=B_SPLINE_CURVE_WITH_KNOTS('',3,(#57004,#57005,#57006,#57007,#57008,
#57009,#57010,#57011,#57012,#57013,#57014,#57015,#57016,#57017,#57018,#57019,
#57020,#57021,#57022,#57023,#57024,#57025,#57026,#57027,#57028,#57029,#57030,
#57031,#57032,#57033,#57034,#57035,#57036,#57037,#57038,#57039,#57040,#57041,
#57042,#57043,#57044,#57045,#57046,#57047,#57048,#57049,#57050,#57051,#57052,
#57053,#57054,#57055,#57056,#57057,#57058,#57059,#57060,#57061,#57062,#57063,
#57064,#57065,#57066,#57067,#57068,#57069,#57070,#57071,#57072,#57073,#57074,
#57075,#57076),.UNSPECIFIED.,.F.,.F.,(4,3,3,3,3,3,3,3,3,3,3,3,3,3,3,3,3,
3,3,3,3,3,3,3,4),(-1.5337369924875,-1.47677061263148,-1.38962639938855,
-1.35507536526616,-1.32724414064724,-1.22771895015351,-1.18711717053979,
-1.15068880045998,-1.12819375965977,-1.025630033795,-0.956371897287304,
-0.903212019653327,-0.873016070576496,-0.765510661060737,-0.671471231953964,
-0.617073852749348,-0.584769201911625,-0.476808850183147,-0.389352944633647,
-0.338455007564916,-0.310839780970012,-0.288641127038734,-0.179465062927756,
-0.0693975027893272,0.),.UNSPECIFIED.);
#1369=B_SPLINE_CURVE_WITH_KNOTS('',3,(#57081,#57082,#57083,#57084,#57085,
#57086,#57087,#57088,#57089,#57090,#57091,#57092,#57093,#57094,#57095,#57096,
#57097,#57098,#57099,#57100,#57101,#57102,#57103,#57104,#57105,#57106,#57107,
#57108,#57109,#57110,#57111,#57112,#57113,#57114,#57115,#57116,#57117,#57118,
#57119,#57120,#57121,#57122,#57123,#57124,#57125,#57126,#57127,#57128,#57129,
#57130,#57131,#57132,#57133,#57134,#57135,#57136,#57137,#57138,#57139,#57140,
#57141,#57142,#57143,#57144,#57145,#57146,#57147,#57148,#57149,#57150,#57151,
#57152,#57153,#57154,#57155,#57156),.UNSPECIFIED.,.F.,.F.,(4,3,3,3,3,3,
3,3,3,3,3,3,3,3,3,3,3,3,3,3,3,3,3,3,3,4),(-1.52870610664523,-1.46295898258929,
-1.36663193757431,-1.32703526012654,-1.2997044260243,-1.18867761427683,
-1.11943990274735,-1.09574005239823,-1.07765080252936,-0.970731016244023,
-0.864758172879583,-0.827864567613179,-0.806080610019377,-0.705048430139015,
-0.615223349572955,-0.566959037307119,-0.545377495328381,-0.521920092205195,
-0.420087461813239,-0.345748107874776,-0.297592979860876,-0.272101849578479,
-0.253166135873108,-0.153094666311387,-0.0548803280409424,0.),
 .UNSPECIFIED.);
#1370=B_SPLINE_CURVE_WITH_KNOTS('',3,(#58129,#58130,#58131,#58132,#58133,
#58134,#58135,#58136,#58137,#58138,#58139,#58140,#58141,#58142,#58143,#58144,
#58145,#58146,#58147,#58148,#58149,#58150),.UNSPECIFIED.,.F.,.F.,(4,3,3,
3,3,3,3,4),(114.220984235376,114.52221015029,115.020132803117,115.518055455945,
116.015978108772,116.513900761599,117.011823414427,117.426450205879),
 .UNSPECIFIED.);
#1371=B_SPLINE_CURVE_WITH_KNOTS('',3,(#58152,#58153,#58154,#58155,#58156,
#58157,#58158,#58159,#58160,#58161,#58162,#58163,#58164,#58165,#58166,#58167,
#58168,#58169,#58170,#58171,#58172,#58173,#58174,#58175,#58176,#58177,#58178,
#58179,#58180,#58181,#58182,#58183,#58184,#58185,#58186,#58187,#58188,#58189,
#58190,#58191,#58192,#58193,#58194,#58195,#58196,#58197,#58198,#58199,#58200,
#58201,#58202,#58203,#58204,#58205,#58206,#58207,#58208,#58209,#58210,#58211,
#58212,#58213,#58214,#58215,#58216,#58217,#58218,#58219,#58220,#58221,#58222,
#58223,#58224),.UNSPECIFIED.,.F.,.F.,(4,3,3,3,3,3,3,3,3,3,3,3,3,3,3,3,3,
3,3,3,3,3,3,3,4),(-1.53373699248749,-1.47677061263144,-1.38962639938852,
-1.35507537101752,-1.32724414240614,-1.22771895103294,-1.18711716909541,
-1.15068880119813,-1.12819375965975,-1.02563002916522,-0.95637190842141,
-0.903212033779905,-0.873016068995821,-0.765510661060749,-0.671471231953977,
-0.617073858764053,-0.584769201584582,-0.476808845396831,-0.389352944633662,
-0.338455004320312,-0.310839774199194,-0.288641121416588,-0.179465094293374,
-0.0693975125282933,0.),.UNSPECIFIED.);
#1372=B_SPLINE_CURVE_WITH_KNOTS('',3,(#58225,#58226,#58227,#58228,#58229,
#58230,#58231,#58232,#58233,#58234,#58235,#58236,#58237,#58238),
 .UNSPECIFIED.,.F.,.F.,(4,1,1,1,1,1,1,1,1,1,1,4),(10.3761157273101,10.7907425187629,
11.2886651715902,11.7865878244176,12.2845104772449,12.7824331300723,13.2803557828996,
13.778278435727,14.2762010885543,14.7741237413817,15.272046394209,15.7079632679489),
 .UNSPECIFIED.);
#1373=B_SPLINE_CURVE_WITH_KNOTS('',3,(#58244,#58245,#58246,#58247,#58248,
#58249,#58250,#58251,#58252,#58253,#58254,#58255,#58256,#58257,#58258,#58259,
#58260,#58261,#58262,#58263,#58264,#58265,#58266,#58267,#58268,#58269,#58270,
#58271,#58272,#58273,#58274,#58275,#58276,#58277,#58278,#58279,#58280,#58281,
#58282,#58283,#58284,#58285,#58286,#58287,#58288,#58289,#58290,#58291,#58292,
#58293,#58294,#58295,#58296,#58297,#58298,#58299,#58300,#58301,#58302,#58303,
#58304,#58305,#58306,#58307,#58308,#58309,#58310,#58311,#58312,#58313,#58314,
#58315,#58316,#58317,#58318,#58319),.UNSPECIFIED.,.F.,.F.,(4,3,3,3,3,3,
3,3,3,3,3,3,3,3,3,3,3,3,3,3,3,3,3,3,3,4),(-1.52870610664511,-1.46295898258918,
-1.36663193757421,-1.32703525676065,-1.29970441890487,-1.18867761071707,
-1.11943990050039,-1.09574005213221,-1.07765080252928,-0.970731019336594,
-0.864758197089689,-0.827864489400151,-0.806080595680503,-0.705048430138953,
-0.615223349572903,-0.566959036424461,-0.545377489997276,-0.521920089539238,
-0.420087427185088,-0.345748107874755,-0.297592967728844,-0.272101809436843,
-0.253166083083881,-0.153094612893034,-0.0548803342925537,0.),
 .UNSPECIFIED.);
#1374=B_SPLINE_CURVE_WITH_KNOTS('',3,(#58322,#58323,#58324,#58325,#58326,
#58327,#58328,#58329,#58330,#58331,#58332,#58333),.UNSPECIFIED.,.F.,.F.,
(4,1,1,1,1,1,1,1,1,4),(11.6150328478182,12.1129555006455,12.6108781534729,
13.1088008063002,13.6067234591276,14.1046461119549,14.6025687647823,15.1004914176096,
15.5984140704369,15.7079632679489),.UNSPECIFIED.);
#1375=B_SPLINE_CURVE_WITH_KNOTS('',3,(#59306,#59307,#59308,#59309,#59310,
#59311,#59312,#59313,#59314,#59315,#59316,#59317,#59318,#59319,#59320,#59321),
 .UNSPECIFIED.,.F.,.F.,(4,3,3,3,3,4),(-119.501436678563,-119.003514025736,
-118.505591372909,-118.007668720081,-117.509746067254,-117.190265949363),
 .UNSPECIFIED.);
#1376=B_SPLINE_CURVE_WITH_KNOTS('',3,(#59671,#59672,#59673,#59674,#59675,
#59676,#59677,#59678,#59679,#59680,#59681,#59682,#59683,#59684,#59685,#59686,
#59687,#59688,#59689,#59690,#59691,#59692,#59693,#59694,#59695,#59696,#59697,
#59698,#59699,#59700,#59701,#59702,#59703,#59704,#59705,#59706,#59707,#59708,
#59709,#59710,#59711,#59712,#59713,#59714,#59715,#59716),.UNSPECIFIED.,
 .T.,.F.,(4,1,1,1,1,1,1,1,1,1,1,1,1,1,1,1,1,1,1,1,1,1,1,1,1,1,1,1,1,1,1,
1,1,1,1,1,1,1,1,1,1,1,1,4),(0.,0.434952646357303,0.869905292714605,1.08738161589326,
1.30485793907191,1.73981058542921,2.17476323178651,2.39223955496516,2.50097771655449,
2.55534679734915,2.60971587814382,3.04466852450112,3.15340668609044,3.47962117085842,
3.51586722472153,3.55211327858464,3.62460538631086,3.76958960176329,4.05955803266816,
4.34952646357303,4.6394948944779,4.92946332538276,5.21943175628763,5.5094001871925,
5.72687651037115,5.79936861809737,6.37930547990711,6.66927391081198,6.95924234171684,
7.24921077262171,7.53917920352658,7.82914763443145,8.11911606533632,8.26410028078875,
8.69905292714605,8.98902135805092,9.27898978895579,9.85892665076553,10.4388635125753,
10.8738161589326,10.9825543205219,11.3087688052899,11.7437214516472,12.1786740980045),
 .UNSPECIFIED.);
#1377=B_SPLINE_CURVE_WITH_KNOTS('',3,(#59717,#59718,#59719,#59720,#59721,
#59722,#59723,#59724,#59725,#59726,#59727,#59728,#59729,#59730,#59731,#59732,
#59733,#59734,#59735,#59736,#59737,#59738,#59739,#59740,#59741,#59742,#59743,
#59744,#59745,#59746,#59747,#59748,#59749,#59750,#59751,#59752,#59753,#59754,
#59755,#59756,#59757,#59758,#59759,#59760,#59761,#59762),.UNSPECIFIED.,
 .T.,.F.,(4,1,1,1,1,1,1,1,1,1,1,1,1,1,1,1,1,1,1,1,1,1,1,1,1,1,1,1,1,1,1,
1,1,1,1,1,1,1,1,1,1,1,1,4),(-12.1786740980045,-11.7437214516472,-11.3087688052899,
-10.9825543205219,-10.8738161589326,-10.4388635125753,-9.85892665076553,
-9.27898978895579,-8.98902135805092,-8.69905292714605,-8.26410028078875,
-8.11911606533632,-7.82914763443145,-7.53917920352658,-7.24921077262171,
-6.95924234171684,-6.66927391081198,-6.37930547990711,-5.79936861809737,
-5.72687651037115,-5.5094001871925,-5.21943175628763,-4.92946332538276,
-4.6394948944779,-4.34952646357303,-4.05955803266816,-3.76958960176329,
-3.62460538631086,-3.55211327858464,-3.51586722472153,-3.47962117085842,
-3.15340668609044,-3.04466852450112,-2.60971587814382,-2.55534679734915,
-2.50097771655449,-2.39223955496516,-2.17476323178651,-1.73981058542921,
-1.30485793907191,-1.08738161589326,-0.869905292714605,-0.434952646357303,
0.),.UNSPECIFIED.);
#1378=B_SPLINE_CURVE_WITH_KNOTS('',3,(#59770,#59771,#59772,#59773,#59774,
#59775,#59776,#59777,#59778,#59779,#59780,#59781,#59782,#59783,#59784,#59785,
#59786,#59787,#59788,#59789,#59790,#59791,#59792,#59793,#59794,#59795,#59796,
#59797,#59798,#59799,#59800,#59801,#59802,#59803,#59804,#59805,#59806,#59807,
#59808,#59809,#59810,#59811,#59812,#59813,#59814,#59815,#59816,#59817,#59818,
#59819,#59820,#59821,#59822,#59823),.UNSPECIFIED.,.T.,.F.,(4,1,1,1,1,1,
1,1,1,1,1,1,1,1,1,1,1,1,1,1,1,1,1,1,1,1,1,1,1,1,1,1,1,1,1,1,1,1,1,1,1,1,
1,1,1,1,1,1,1,1,1,4),(-12.1786740980045,-11.7437214516472,-11.3087688052899,
-10.9825543205219,-10.8738161589326,-10.4388635125753,-9.85892665076553,
-9.64145032758688,-9.27898978895579,-8.98902135805092,-8.69905292714606,
-8.55406871169362,-8.11911606533632,-7.82914763443145,-7.53917920352658,
-7.24921077262171,-7.03173444944306,-6.95924234171684,-6.37930547990711,
-6.08933704900224,-6.01684494127602,-5.79936861809737,-5.5094001871925,
-5.21943175628763,-4.92946332538276,-4.85697121765655,-4.6394948944779,
-4.34952646357303,-4.05955803266816,-3.87832776335262,-3.76958960176329,
-3.62460538631086,-3.55211327858464,-3.52492873818731,-3.51586722472153,
-3.47962117085842,-3.04466852450112,-2.88156128211713,-2.60971587814382,
-2.58253133774649,-2.55534679734915,-2.51456998675316,-2.50097771655449,
-2.39223955496517,-2.17476323178651,-1.84854874701854,-1.73981058542921,
-1.30485793907191,-1.08738161589326,-0.869905292714606,-0.434952646357303,
0.),.UNSPECIFIED.);
#1379=B_SPLINE_CURVE_WITH_KNOTS('',3,(#59825,#59826,#59827,#59828,#59829,
#59830,#59831,#59832,#59833,#59834,#59835,#59836,#59837,#59838,#59839,#59840,
#59841,#59842,#59843,#59844,#59845,#59846,#59847,#59848,#59849,#59850,#59851,
#59852,#59853,#59854,#59855,#59856,#59857,#59858,#59859,#59860,#59861,#59862,
#59863,#59864,#59865,#59866,#59867,#59868,#59869,#59870,#59871,#59872,#59873,
#59874,#59875,#59876,#59877,#59878,#59879,#59880,#59881,#59882),
 .UNSPECIFIED.,.T.,.F.,(4,1,1,1,1,1,1,1,1,1,1,1,1,1,1,1,1,1,1,1,1,1,1,1,
1,1,1,1,1,1,1,1,1,1,1,1,1,1,1,1,1,1,1,1,1,1,1,1,1,1,1,1,1,1,1,4),(-4.85574113812961,
-4.50890248540607,-4.42219282222518,-4.37883799063474,-4.35716057483952,
-4.33548315904429,-4.16206383268252,-4.07535416950164,-3.98864450632075,
-3.90193484313987,-3.85858001154942,-3.8369025957542,-3.82606388785659,
-3.81522517995898,-3.64180585359721,-3.46838652723544,-3.46296717328663,
-3.45754781933783,-3.44670911144021,-3.4358704035426,-3.42503169564499,
-3.40335427984977,-3.39251557195216,-3.38167686405455,-3.29496720087366,
-3.20825753769278,-3.12154787451189,-2.94812854815012,-2.77470922178835,
-2.65909633754717,-2.60128989542658,-2.57238667436628,-2.54348345330599,
-2.31225768482362,-2.28335446376333,-2.25445124270303,-2.19664480058244,
-2.13883835846185,-2.10993513740156,-2.08103191634126,-1.8498061478589,
-1.73419326361772,-1.61858037937654,-1.50296749513536,-1.44516105301476,
-1.41625783195447,-1.38735461089417,-1.04051595817063,-0.997161126580188,
-0.953806294989745,-0.867096631808859,-0.693677305447087,-0.520257979085315,
-0.346838652723544,-0.173419326361772,0.),.UNSPECIFIED.);
#1380=B_SPLINE_CURVE_WITH_KNOTS('',3,(#59886,#59887,#59888,#59889,#59890,
#59891,#59892,#59893,#59894,#59895,#59896,#59897,#59898,#59899,#59900,#59901,
#59902,#59903,#59904,#59905,#59906,#59907,#59908,#59909,#59910,#59911,#59912,
#59913,#59914,#59915,#59916,#59917,#59918,#59919,#59920,#59921,#59922,#59923,
#59924,#59925,#59926,#59927,#59928,#59929,#59930,#59931,#59932,#59933,#59934,
#59935,#59936,#59937,#59938,#59939),.UNSPECIFIED.,.T.,.F.,(4,1,1,1,1,1,
1,1,1,1,1,1,1,1,1,1,1,1,1,1,1,1,1,1,1,1,1,1,1,1,1,1,1,1,1,1,1,1,1,1,1,1,
1,1,1,1,1,1,1,1,1,4),(0.,0.434952646357303,0.869905292714606,1.08738161589326,
1.30485793907191,1.73981058542921,1.84854874701854,2.17476323178651,2.39223955496517,
2.50097771655449,2.51456998675316,2.55534679734915,2.58253133774649,2.60971587814382,
2.88156128211713,3.04466852450112,3.47962117085842,3.51586722472153,3.52492873818731,
3.55211327858464,3.62460538631086,3.76958960176329,3.87832776335262,4.05955803266816,
4.34952646357303,4.6394948944779,4.85697121765655,4.92946332538276,5.21943175628763,
5.5094001871925,5.79936861809737,6.01684494127602,6.08933704900224,6.37930547990711,
6.95924234171684,7.03173444944306,7.24921077262171,7.53917920352658,7.82914763443145,
8.11911606533632,8.55406871169362,8.69905292714606,8.98902135805092,9.27898978895579,
9.64145032758688,9.85892665076553,10.4388635125753,10.8738161589326,10.9825543205219,
11.3087688052899,11.7437214516472,12.1786740980045),.UNSPECIFIED.);
#1381=B_SPLINE_CURVE_WITH_KNOTS('',3,(#59944,#59945,#59946,#59947,#59948,
#59949,#59950,#59951,#59952),.UNSPECIFIED.,.F.,.F.,(4,1,1,1,1,1,4),(-5.09886318526994,
-4.84376308104545,-4.72085363669404,-4.51600456277503,-4.35212530363983,
-4.18824604450462,-4.17262768684822),.UNSPECIFIED.);
#1382=B_SPLINE_CURVE_WITH_KNOTS('',3,(#59955,#59956,#59957,#59958,#59959,
#59960,#59961,#59962,#59963,#59964),.UNSPECIFIED.,.F.,.F.,(4,1,1,1,1,1,
1,4),(-2.00844283647624,-1.91712585131231,-1.75323014222306,-1.58933443313382,
-1.42543872404457,-1.26154301495533,-1.09764730586608,-1.08195609140638),
 .UNSPECIFIED.);
#1383=B_SPLINE_CURVE_WITH_KNOTS('',3,(#60191,#60192,#60193,#60194,#60195,
#60196,#60197,#60198,#60199,#60200,#60201,#60202,#60203,#60204,#60205),
 .UNSPECIFIED.,.F.,.F.,(4,1,1,1,1,1,1,1,2,2,4),(0.442064469509103,0.769855887687593,
1.09764730586608,1.26154301495533,1.42543872404457,1.58933443313382,1.75323014222306,
1.91712585131231,2.08102156040155,2.14351932926336,2.6484237026181),
 .UNSPECIFIED.);
#1384=B_SPLINE_CURVE_WITH_KNOTS('',3,(#60209,#60210,#60211,#60212,#60213,
#60214,#60215,#60216,#60217,#60218,#60219,#60220,#60221,#60222),
 .UNSPECIFIED.,.F.,.F.,(4,1,1,1,1,1,1,2,2,4),(3.53272900796379,3.8604875262342,
4.18824604450462,4.35212530363983,4.51600456277503,4.72085363669404,4.84376308104545,
5.17152159931586,5.23401936817767,5.73877023945777),.UNSPECIFIED.);
#1385=B_SPLINE_CURVE_WITH_KNOTS('',3,(#60290,#60291,#60292,#60293,#60294,
#60295),.UNSPECIFIED.,.F.,.F.,(4,2,4),(0.,0.395295738561713,0.750556975338415),
 .UNSPECIFIED.);
#1386=B_SPLINE_CURVE_WITH_KNOTS('',3,(#60296,#60297,#60298,#60299,#60300,
#60301),.UNSPECIFIED.,.F.,.F.,(4,2,4),(0.,0.242165599626981,0.747632926534989),
 .UNSPECIFIED.);
#1387=B_SPLINE_CURVE_WITH_KNOTS('',3,(#60358,#60359,#60360,#60361,#60362,
#60363),.UNSPECIFIED.,.F.,.F.,(4,2,4),(0.,0.395285417853985,0.750556986687262),
 .UNSPECIFIED.);
#1388=B_SPLINE_CURVE_WITH_KNOTS('',3,(#60364,#60365,#60366,#60367,#60368,
#60369),.UNSPECIFIED.,.F.,.F.,(4,2,4),(0.,0.242119658779455,0.747632520146835),
 .UNSPECIFIED.);
#1389=B_SPLINE_CURVE_WITH_KNOTS('',3,(#60470,#60471,#60472,#60473,#60474,
#60475,#60476,#60477,#60478,#60479,#60480,#60481,#60482,#60483,#60484,#60485,
#60486,#60487,#60488,#60489,#60490),.UNSPECIFIED.,.F.,.F.,(4,1,1,1,1,2,
2,1,2,1,1,1,1,1,1,4),(-3.74583112016425,-3.27642035446956,-3.15906766304589,
-2.80700958877487,-2.33759882308018,-1.86818805738549,-1.79629199573878,
-1.50783982646145,-1.21938765718412,-0.911365009587737,-0.757353685789545,
-0.603342361991352,-0.295319714394966,-0.141308390596773,0.0127029332014201,
0.0186613584180625),.UNSPECIFIED.);
#1390=B_SPLINE_CURVE_WITH_KNOTS('',3,(#60491,#60492,#60493,#60494,#60495,
#60496,#60497),.UNSPECIFIED.,.F.,.F.,(4,1,1,1,4),(0.0186613584180625,0.320725580797806,
0.628748228394192,0.936770875990578,1.24479352358696),.UNSPECIFIED.);
#1391=B_SPLINE_CURVE_WITH_KNOTS('',3,(#60499,#60500,#60501,#60502,#60503,
#60504,#60505,#60506,#60507,#60508,#60509),.UNSPECIFIED.,.F.,.F.,(4,1,1,
1,1,1,1,1,4),(-1.24479352358696,-0.936770875990578,-0.628748228394192,-0.320725580797806,
-0.0127029332014201,0.141308390596773,0.295319714394966,0.603342361991352,
0.74818116877789),.UNSPECIFIED.);
#1392=B_SPLINE_CURVE_WITH_KNOTS('',3,(#60511,#60512,#60513,#60514,#60515,
#60516,#60517,#60518,#60519),.UNSPECIFIED.,.F.,.F.,(4,1,1,2,1,4),(0.74818116877789,
0.757353685789545,0.911365009587737,1.21938765718412,1.50783982646145,1.69059414559038),
 .UNSPECIFIED.);
#1393=B_SPLINE_CURVE_WITH_KNOTS('',3,(#60520,#60521,#60522,#60523,#60524,
#60525,#60526,#60527,#60528,#60529,#60530,#60531),.UNSPECIFIED.,.F.,.F.,
(4,2,2,1,1,1,1,4),(1.69059414559038,1.79629199573878,1.86818805738549,2.33759882308018,
2.80700958877487,3.15906766304589,3.27642035446956,3.74583112016425),
 .UNSPECIFIED.);
#1394=B_SPLINE_CURVE_WITH_KNOTS('',3,(#60534,#60535,#60536,#60537,#60538,
#60539,#60540,#60541,#60542,#60543,#60544,#60545,#60546,#60547,#60548,#60549,
#60550,#60551,#60552,#60553,#60554,#60555,#60556,#60557,#60558,#60559,#60560,
#60561,#60562,#60563,#60564,#60565,#60566,#60567,#60568,#60569,#60570,#60571,
#60572,#60573,#60574,#60575,#60576,#60577,#60578,#60579,#60580,#60581,#60582,
#60583,#60584,#60585,#60586,#60587,#60588,#60589,#60590,#60591),
 .UNSPECIFIED.,.T.,.F.,(4,1,1,1,1,1,1,1,1,1,1,1,1,1,1,1,1,1,1,1,1,1,1,1,
1,1,1,1,1,1,1,1,1,1,1,1,1,1,1,1,1,1,1,1,1,1,1,1,1,1,1,1,1,1,1,4),(0.,0.173419326361772,
0.346838652723544,0.520257979085315,0.693677305447087,0.867096631808859,
0.953806294989745,0.997161126580188,1.04051595817063,1.38735461089417,1.41625783195447,
1.44516105301476,1.50296749513536,1.61858037937654,1.73419326361772,1.8498061478589,
2.08103191634126,2.10993513740156,2.13883835846185,2.19664480058244,2.25445124270303,
2.28335446376333,2.31225768482362,2.54348345330599,2.57238667436628,2.60128989542658,
2.65909633754717,2.77470922178835,2.94812854815012,3.12154787451189,3.20825753769278,
3.29496720087366,3.38167686405455,3.39251557195216,3.40335427984977,3.42503169564499,
3.4358704035426,3.44670911144021,3.45754781933783,3.46296717328663,3.46838652723544,
3.64180585359721,3.81522517995898,3.82606388785659,3.8369025957542,3.85858001154942,
3.90193484313987,3.98864450632075,4.07535416950164,4.16206383268252,4.33548315904429,
4.35716057483952,4.37883799063474,4.42219282222518,4.50890248540607,4.85574113812961),
 .UNSPECIFIED.);
#1395=B_SPLINE_CURVE_WITH_KNOTS('',3,(#63561,#63562,#63563,#63564,#63565,
#63566,#63567,#63568,#63569,#63570,#63571,#63572,#63573),.UNSPECIFIED.,
 .F.,.F.,(4,1,1,1,1,1,1,1,1,1,4),(0.,0.176188248237271,0.352376496474541,
0.528564744711812,0.704752992949082,0.880941241186353,0.969035365304988,
1.01308242736431,1.03510595839396,1.05712948942362,1.23331773766089),
 .UNSPECIFIED.);
#1396=B_SPLINE_CURVE_WITH_KNOTS('',3,(#63574,#63575,#63576,#63577,#63578,
#63579,#63580,#63581,#63582,#63583,#63584,#63585,#63586,#63587,#63588,#63589,
#63590,#63591,#63592,#63593,#63594,#63595,#63596,#63597,#63598,#63599,#63600,
#63601,#63602,#63603,#63604),.UNSPECIFIED.,.F.,.F.,(4,1,1,1,1,1,1,1,1,1,
1,1,1,1,1,1,1,1,1,1,1,1,1,1,1,1,1,1,4),(1.23331773766089,1.40950598589816,
1.42418833991794,1.43887069393771,1.46823540197725,1.52696481805635,1.64442365021453,
1.76188248237271,1.87934131453089,2.11425897884725,2.17298839492634,2.23171781100543,
2.34917664316361,2.58409430747997,2.64282372355906,2.81901197179633,2.93647080395451,
3.05392963611269,3.17138846827087,3.28884730042905,3.52376496474541,3.64122379690359,
3.75868262906177,3.99360029337813,4.22851795769449,4.40470620593176,4.58089445416904,
4.75708270240631,4.93327095064358),.UNSPECIFIED.);
#1397=B_SPLINE_CURVE_WITH_KNOTS('',3,(#63605,#63606,#63607,#63608,#63609,
#63610,#63611,#63612,#63613,#63614,#63615,#63616,#63617,#63618,#63619,#63620,
#63621,#63622,#63623,#63624,#63625,#63626,#63627,#63628,#63629,#63630,#63631,
#63632,#63633,#63634,#63635,#63636,#63637,#63638,#63639,#63640,#63641,#63642,
#63643,#63644),.UNSPECIFIED.,.T.,.F.,(4,1,1,1,1,1,1,1,1,1,1,1,1,1,1,1,1,
1,1,1,1,1,1,1,1,1,1,1,1,1,1,1,1,1,1,1,1,4),(-4.93327095064358,-4.75708270240631,
-4.58089445416904,-4.40470620593176,-4.22851795769449,-3.99360029337813,
-3.75868262906177,-3.64122379690359,-3.52376496474541,-3.28884730042905,
-3.17138846827087,-3.05392963611269,-2.93647080395451,-2.81901197179633,
-2.64282372355906,-2.58409430747997,-2.34917664316361,-2.23171781100543,
-2.17298839492634,-2.11425897884725,-1.87934131453089,-1.76188248237271,
-1.64442365021453,-1.52696481805635,-1.46823540197725,-1.43887069393771,
-1.42418833991794,-1.40950598589816,-1.05712948942362,-1.03510595839396,
-1.01308242736431,-0.969035365304988,-0.880941241186353,-0.704752992949082,
-0.528564744711812,-0.352376496474541,-0.176188248237271,0.),
 .UNSPECIFIED.);
#1398=B_SPLINE_CURVE_WITH_KNOTS('',3,(#63938,#63939,#63940,#63941,#63942,
#63943,#63944,#63945,#63946,#63947,#63948,#63949),.UNSPECIFIED.,.F.,.F.,
(4,2,2,2,2,4),(-1.10588413989679,-1.10499782596143,-0.91656040147052,-0.772228700060969,
-0.6650055247649,-0.579920166124102),.UNSPECIFIED.);
#1399=B_SPLINE_CURVE_WITH_KNOTS('',3,(#63952,#63953,#63954,#63955,#63956,
#63957,#63958,#63959,#63960,#63961,#63962,#63963,#63964,#63965),
 .UNSPECIFIED.,.F.,.F.,(4,2,2,2,2,2,4),(-0.568877288175113,-0.484148554868537,
-0.388033769227592,-0.2597032346067,-0.133006563450214,0.,0.00108165162707012),
 .UNSPECIFIED.);
#1400=B_SPLINE_CURVE_WITH_KNOTS('',3,(#63974,#63975,#63976,#63977,#63978,
#63979,#63980,#63981,#63982,#63983,#63984,#63985),.UNSPECIFIED.,.F.,.F.,
(4,2,2,2,2,4),(-0.00108165162924514,0.,0.229967778999105,0.40610922702663,
0.536963676703178,0.64080128223702),.UNSPECIFIED.);
#1401=B_SPLINE_CURVE_WITH_KNOTS('',3,(#63996,#63997,#63998,#63999,#64000,
#64001,#64002,#64003,#64004,#64005,#64006,#64007,#64008,#64009),
 .UNSPECIFIED.,.F.,.F.,(4,2,2,2,2,2,4),(0.,0.0839640955338038,0.179211489526657,
0.306383900210746,0.431937192294976,0.563743432804494,0.564815323027158),
 .UNSPECIFIED.);
#1402=B_SPLINE_CURVE_WITH_KNOTS('',3,(#64272,#64273,#64274,#64275,#64276,
#64277,#64278,#64279,#64280,#64281),.UNSPECIFIED.,.F.,.F.,(4,2,2,2,4),(-0.454509794253164,
-0.340166127818439,-0.225822461383713,-0.112911230691856,0.),
 .UNSPECIFIED.);
#1403=B_SPLINE_CURVE_WITH_KNOTS('',3,(#64287,#64288,#64289,#64290,#64291,
#64292,#64293,#64294,#64295,#64296,#64297,#64298,#64299,#64300),
 .UNSPECIFIED.,.F.,.F.,(4,2,2,2,2,2,4),(0.896032537461048,1.25582804826943,
1.43572580367362,1.61562355907781,1.76667897073219,1.80865046008187,1.84248908085934),
 .UNSPECIFIED.);
#1404=B_SPLINE_CURVE_WITH_KNOTS('',3,(#64306,#64307,#64308,#64309,#64310,
#64311,#64312,#64313,#64314,#64315,#64316,#64317,#64318,#64319),
 .UNSPECIFIED.,.F.,.F.,(4,2,2,2,2,2,4),(-1.84248908085934,-1.80865046008187,
-1.76667897073219,-1.61562355907781,-1.43572580367362,-1.25582804826943,
-0.896032537461048),.UNSPECIFIED.);
#1405=B_SPLINE_CURVE_WITH_KNOTS('',3,(#64325,#64326,#64327,#64328,#64329,
#64330,#64331,#64332,#64333,#64334),.UNSPECIFIED.,.F.,.F.,(4,2,2,2,4),(0.910251315816355,
1.02316254650821,1.13607377720007,1.25041744363479,1.36476111006952),
 .UNSPECIFIED.);
#1406=B_SPLINE_CURVE_WITH_KNOTS('',3,(#64358,#64359,#64360,#64361,#64362,
#64363,#64364,#64365,#64366,#64367),.UNSPECIFIED.,.F.,.F.,(4,2,2,2,4),(0.45204596998448,
0.565054126336166,0.678062282687852,0.791068360433516,0.904074438179181),
 .UNSPECIFIED.);
#1407=B_SPLINE_CURVE_WITH_KNOTS('',3,(#64376,#64377,#64378,#64379,#64380,
#64381),.UNSPECIFIED.,.F.,.F.,(4,2,4),(1.02915974263557,1.15320944997464,
1.25900965381776),.UNSPECIFIED.);
#1408=B_SPLINE_CURVE_WITH_KNOTS('',3,(#64400,#64401,#64402,#64403,#64404,
#64405),.UNSPECIFIED.,.F.,.F.,(4,2,4),(1.70043874542,2.00091514457436,2.20444648124611),
 .UNSPECIFIED.);
#1409=B_SPLINE_CURVE_WITH_KNOTS('',3,(#64413,#64414,#64415,#64416,#64417,
#64418),.UNSPECIFIED.,.F.,.F.,(4,2,4),(1.92266359511738,1.95634912709283,
2.38915999737552),.UNSPECIFIED.);
#1410=B_SPLINE_CURVE_WITH_KNOTS('',3,(#64457,#64458,#64459,#64460,#64461,
#64462),.UNSPECIFIED.,.F.,.F.,(4,2,4),(0.941765464328093,1.04756566817122,
1.17161537551029),.UNSPECIFIED.);
#1411=B_SPLINE_CURVE_WITH_KNOTS('',3,(#64472,#64473,#64474,#64475,#64476,
#64477,#64478,#64479,#64480,#64481),.UNSPECIFIED.,.F.,.F.,(4,2,2,2,4),(1.80814887635836,
1.92115495410403,2.03416103184969,2.14716918820138,2.26017734455306),
 .UNSPECIFIED.);
#1412=B_SPLINE_CURVE_WITH_KNOTS('',3,(#64506,#64507,#64508,#64509,#64510,
#64511),.UNSPECIFIED.,.F.,.F.,(4,2,4),(1.52353825936373,1.95634912840093,
1.99003466162308),.UNSPECIFIED.);
#1413=B_SPLINE_CURVE_WITH_KNOTS('',3,(#64519,#64520,#64521,#64522,#64523,
#64524),.UNSPECIFIED.,.F.,.F.,(4,2,4),(1.79738380790266,2.00091514457441,
2.30139154372878),.UNSPECIFIED.);
#1414=B_SPLINE_CURVE_WITH_KNOTS('',3,(#64530,#64531,#64532,#64533,#64534,
#64535,#64536,#64537,#64538,#64539),.UNSPECIFIED.,.F.,.F.,(4,2,2,2,4),(-0.385669957148059,
-0.267638091880424,-0.132795783635376,0.,0.000970573886634806),
 .UNSPECIFIED.);
#1415=B_SPLINE_CURVE_WITH_KNOTS('',3,(#64542,#64543,#64544,#64545,#64546,
#64547,#64548,#64549,#64550,#64551),.UNSPECIFIED.,.F.,.F.,(4,2,2,2,4),(-0.384357938358326,
-0.383393117455112,-0.251376894581821,-0.117331137795169,-6.31601177111807E-6),
 .UNSPECIFIED.);
#1416=B_SPLINE_CURVE_WITH_KNOTS('',3,(#64554,#64555,#64556,#64557,#64558,
#64559),.UNSPECIFIED.,.F.,.F.,(4,2,4),(0.29237536973302,0.349212088502275,
0.491998450222318),.UNSPECIFIED.);
#1417=B_SPLINE_CURVE_WITH_KNOTS('',3,(#64566,#64567,#64568,#64569,#64570,
#64571),.UNSPECIFIED.,.F.,.F.,(4,2,4),(1.47810928760726,1.6208956493273,
1.67773236809654),.UNSPECIFIED.);
#1418=B_SPLINE_CURVE_WITH_KNOTS('',3,(#64629,#64630,#64631,#64632,#64633,
#64634,#64635,#64636,#64637,#64638),.UNSPECIFIED.,.F.,.F.,(4,2,2,2,4),(-0.00645513076503384,
0.,0.607350167241916,1.21470033231699,1.22115546305417),.UNSPECIFIED.);
#1419=B_SPLINE_CURVE_WITH_KNOTS('',3,(#64646,#64647,#64648,#64649,#64650,
#64651,#64652,#64653,#64654,#64655,#64656,#64657,#64658,#64659,#64660,#64661,
#64662,#64663),.UNSPECIFIED.,.F.,.F.,(4,2,2,2,2,2,2,2,4),(0.,0.753367592696705,
1.50673518539341,2.26010277809012,3.01347037078682,3.76683796348352,4.52020555618022,
5.27357314887692,6.02694074157362),.UNSPECIFIED.);
#1420=B_SPLINE_CURVE_WITH_KNOTS('',3,(#64674,#64675,#64676,#64677,#64678,
#64679,#64680,#64681,#64682,#64683,#64684,#64685,#64686,#64687,#64688,#64689,
#64690,#64691),.UNSPECIFIED.,.F.,.F.,(4,2,2,2,2,2,2,2,4),(-6.02694148316008,
-5.27373586786722,-4.52034502960047,-3.76695419133371,-3.01356335306695,
-2.26017251480021,-1.50678167653347,-0.753390838266739,0.),
 .UNSPECIFIED.);
#1421=B_SPLINE_CURVE_WITH_KNOTS('',3,(#64698,#64699,#64700,#64701,#64702,
#64703,#64704,#64705,#64706,#64707,#64708,#64709,#64710,#64711),
 .UNSPECIFIED.,.F.,.F.,(4,2,2,2,2,2,4),(-1.35055637186862,-1.34938170454602,
-1.1819777528807,-1.01919166368985,-0.865721094274056,-0.748962828335224,
-0.646651719983809),.UNSPECIFIED.);
#1422=B_SPLINE_CURVE_WITH_KNOTS('',3,(#64713,#64714,#64715,#64716,#64717,
#64718,#64719,#64720,#64721,#64722,#64723,#64724,#64725,#64726),
 .UNSPECIFIED.,.F.,.F.,(4,2,2,2,2,2,4),(-0.575633174348645,-0.491826207716573,
-0.3961850186411,-0.270471368845074,-0.13712701884174,0.,0.000962215215251001),
 .UNSPECIFIED.);
#1423=B_SPLINE_CURVE_WITH_KNOTS('',3,(#64768,#64769,#64770,#64771,#64772,
#64773,#64774,#64775,#64776,#64777,#64778,#64779,#64780,#64781),
 .UNSPECIFIED.,.F.,.F.,(4,2,2,2,2,2,4),(-1.35886617414881,-1.31800777766679,
-1.27191156834586,-1.14095894304151,-0.942079387318738,-0.807488859272477,
-0.672898331226217),.UNSPECIFIED.);
#1424=B_SPLINE_CURVE_WITH_KNOTS('',3,(#64785,#64786,#64787,#64788,#64789,
#64790,#64791,#64792,#64793,#64794,#64795,#64796,#64797,#64798),
 .UNSPECIFIED.,.F.,.F.,(4,2,2,2,2,2,4),(0.896032537461047,1.25582804826943,
1.43572580367362,1.61562355907781,1.76667897073219,1.80865046008187,1.84248908085934),
 .UNSPECIFIED.);
#1425=B_SPLINE_CURVE_WITH_KNOTS('',3,(#64814,#64815,#64816,#64817,#64818,
#64819,#64820,#64821,#64822,#64823,#64824,#64825,#64826,#64827),
 .UNSPECIFIED.,.F.,.F.,(4,2,2,2,2,2,4),(-1.84248908085934,-1.80865046008187,
-1.76667897073219,-1.61562355907781,-1.43572580367362,-1.25582804826943,
-0.896032537461046),.UNSPECIFIED.);
#1426=B_SPLINE_CURVE_WITH_KNOTS('',3,(#64830,#64831,#64832,#64833,#64834,
#64835,#64836,#64837,#64838,#64839,#64840,#64841,#64842,#64843),
 .UNSPECIFIED.,.F.,.F.,(4,2,2,2,2,2,4),(0.672898331226217,0.807488859272477,
0.942079387318738,1.14095894304151,1.27191156834586,1.31800777766679,1.35886617414881),
 .UNSPECIFIED.);
#1427=B_SPLINE_CURVE_WITH_KNOTS('',3,(#64924,#64925,#64926,#64927,#64928,
#64929),.UNSPECIFIED.,.F.,.F.,(4,2,4),(-0.154287651470972,-0.153320461931147,
-0.0301403351196061),.UNSPECIFIED.);
#1428=B_SPLINE_CURVE_WITH_KNOTS('',3,(#64933,#64934,#64935,#64936,#64937,
#64938),.UNSPECIFIED.,.F.,.F.,(4,2,4),(0.0301403351196109,0.153320461931147,
0.154287651470978),.UNSPECIFIED.);
#1429=B_SPLINE_CURVE_WITH_KNOTS('',3,(#65002,#65003,#65004,#65005),
 .UNSPECIFIED.,.F.,.F.,(4,4),(23.0837010026238,23.1300949206487),
 .UNSPECIFIED.);
#1430=B_SPLINE_CURVE_WITH_KNOTS('',3,(#65006,#65007,#65008,#65009,#65010,
#65011),.UNSPECIFIED.,.F.,.F.,(4,2,4),(-0.978411907643555,-0.753390838266736,
0.),.UNSPECIFIED.);
#1431=B_SPLINE_CURVE_WITH_KNOTS('',3,(#65020,#65021,#65022,#65023,#65024,
#65025,#65026,#65027,#65028,#65029),.UNSPECIFIED.,.F.,.F.,(4,2,2,2,4),(-6.02694148316005,
-5.27373586786722,-4.52034502960046,-3.7669541913337,-3.53970622743003),
 .UNSPECIFIED.);
#1432=B_SPLINE_CURVE_WITH_KNOTS('',2,(#65054,#65055,#65056),
 .UNSPECIFIED.,.F.,.F.,(3,3),(0.,1.),.UNSPECIFIED.);
#1433=B_SPLINE_CURVE_WITH_KNOTS('',2,(#65058,#65059,#65060),
 .UNSPECIFIED.,.F.,.F.,(3,3),(0.,1.),.UNSPECIFIED.);
#1434=B_SPLINE_CURVE_WITH_KNOTS('',2,(#65062,#65063,#65064),
 .UNSPECIFIED.,.F.,.F.,(3,3),(0.,1.),.UNSPECIFIED.);
#1435=B_SPLINE_CURVE_WITH_KNOTS('',2,(#65066,#65067,#65068),
 .UNSPECIFIED.,.F.,.F.,(3,3),(0.,1.),.UNSPECIFIED.);
#1436=B_SPLINE_CURVE_WITH_KNOTS('',2,(#65070,#65071,#65072),
 .UNSPECIFIED.,.F.,.F.,(3,3),(0.,1.),.UNSPECIFIED.);
#1437=B_SPLINE_CURVE_WITH_KNOTS('',2,(#65074,#65075,#65076),
 .UNSPECIFIED.,.F.,.F.,(3,3),(0.,1.),.UNSPECIFIED.);
#1438=B_SPLINE_CURVE_WITH_KNOTS('',2,(#65078,#65079,#65080),
 .UNSPECIFIED.,.F.,.F.,(3,3),(0.,1.),.UNSPECIFIED.);
#1439=B_SPLINE_CURVE_WITH_KNOTS('',2,(#65082,#65083,#65084),
 .UNSPECIFIED.,.F.,.F.,(3,3),(0.,1.),.UNSPECIFIED.);
#1440=B_SPLINE_CURVE_WITH_KNOTS('',2,(#65086,#65087,#65088),
 .UNSPECIFIED.,.F.,.F.,(3,3),(0.,1.),.UNSPECIFIED.);
#1441=B_SPLINE_CURVE_WITH_KNOTS('',2,(#65089,#65090,#65091),
 .UNSPECIFIED.,.F.,.F.,(3,3),(0.,1.),.UNSPECIFIED.);
#1442=B_SPLINE_CURVE_WITH_KNOTS('',2,(#65130,#65131,#65132),
 .UNSPECIFIED.,.F.,.F.,(3,3),(0.,1.),.UNSPECIFIED.);
#1443=B_SPLINE_CURVE_WITH_KNOTS('',2,(#65134,#65135,#65136),
 .UNSPECIFIED.,.F.,.F.,(3,3),(0.,1.),.UNSPECIFIED.);
#1444=B_SPLINE_CURVE_WITH_KNOTS('',2,(#65140,#65141,#65142),
 .UNSPECIFIED.,.F.,.F.,(3,3),(0.,1.),.UNSPECIFIED.);
#1445=B_SPLINE_CURVE_WITH_KNOTS('',2,(#65144,#65145,#65146),
 .UNSPECIFIED.,.F.,.F.,(3,3),(0.,1.),.UNSPECIFIED.);
#1446=B_SPLINE_CURVE_WITH_KNOTS('',3,(#65197,#65198,#65199,#65200,#65201,
#65202),.UNSPECIFIED.,.F.,.F.,(4,2,4),(0.,0.753367592696704,0.978410263145562),
 .UNSPECIFIED.);
#1447=B_SPLINE_CURVE_WITH_KNOTS('',3,(#65203,#65204,#65205,#65206),
 .UNSPECIFIED.,.F.,.F.,(4,4),(0.978410263146837,1.02480406428257),
 .UNSPECIFIED.);
#1448=B_SPLINE_CURVE_WITH_KNOTS('',3,(#65281,#65282,#65283,#65284,#65285,
#65286,#65287,#65288,#65289,#65290,#65291,#65292,#65293,#65294,#65295,#65296,
#65297,#65298,#65299,#65300),.UNSPECIFIED.,.F.,.F.,(4,2,2,2,2,2,2,2,2,4),
(0.,1.50665307727383,3.01330615454765,4.51995923182148,6.0266123090953,
7.53326538636832,9.03991846364135,10.5465715409144,12.0532246181874,12.0542197677389),
 .UNSPECIFIED.);
#1449=B_SPLINE_CURVE_WITH_KNOTS('',3,(#65302,#65303,#65304,#65305,#65306,
#65307,#65308,#65309,#65310,#65311,#65312,#65313,#65314,#65315,#65316,#65317,
#65318,#65319),.UNSPECIFIED.,.F.,.F.,(4,2,2,2,2,2,2,2,4),(-12.0542237737762,
-10.5474458020542,-9.04066783033219,-7.53388985861016,-6.02711188688813,
-4.5203339151661,-3.01355594344407,-1.50677797172204,0.),.UNSPECIFIED.);
#1450=B_SPLINE_CURVE_WITH_KNOTS('',3,(#65378,#65379,#65380,#65381,#65382,
#65383,#65384,#65385,#65386,#65387),.UNSPECIFIED.,.F.,.F.,(4,2,2,2,4),(3.5397019033151,
3.76683796348352,4.52020555618022,5.27357314887692,6.02694074157362),
 .UNSPECIFIED.);
#1451=B_SPLINE_CURVE_WITH_KNOTS('',3,(#65410,#65411,#65412,#65413,#65414,
#65415,#65416,#65417,#65418,#65419,#65420,#65421,#65422,#65423,#65424,#65425),
 .UNSPECIFIED.,.F.,.F.,(4,2,2,2,2,2,2,4),(0.,1.50665307727383,3.01330615454765,
4.51995923182148,6.02661230909531,7.53326538636833,9.03991846364136,9.06280469595813),
 .UNSPECIFIED.);
#1452=B_SPLINE_CURVE_WITH_KNOTS('',3,(#65431,#65432,#65433,#65434,#65435,
#65436,#65437,#65438,#65439,#65440,#65441,#65442,#65443,#65444,#65445,#65446),
 .UNSPECIFIED.,.F.,.F.,(4,2,2,2,2,2,2,4),(-9.06285135664527,-9.0406678303322,
-7.53388985861017,-6.02711188688814,-4.5203339151661,-3.01355594344407,
-1.50677797172204,0.),.UNSPECIFIED.);
#1453=B_SPLINE_CURVE_WITH_KNOTS('',2,(#65485,#65486,#65487),
 .UNSPECIFIED.,.F.,.F.,(3,3),(-1.,0.),.UNSPECIFIED.);
#1454=B_SPLINE_CURVE_WITH_KNOTS('',2,(#65496,#65497,#65498),
 .UNSPECIFIED.,.F.,.F.,(3,3),(-1.,0.),.UNSPECIFIED.);
#1455=B_SPLINE_CURVE_WITH_KNOTS('',2,(#65511,#65512,#65513),
 .UNSPECIFIED.,.F.,.F.,(3,3),(-1.,0.),.UNSPECIFIED.);
#1456=B_SPLINE_CURVE_WITH_KNOTS('',2,(#65522,#65523,#65524),
 .UNSPECIFIED.,.F.,.F.,(3,3),(-1.,0.),.UNSPECIFIED.);
#1457=B_SPLINE_CURVE_WITH_KNOTS('',2,(#65578,#65579,#65580),
 .UNSPECIFIED.,.F.,.F.,(3,3),(0.,1.),.UNSPECIFIED.);
#1458=B_SPLINE_CURVE_WITH_KNOTS('',2,(#65584,#65585,#65586),
 .UNSPECIFIED.,.F.,.F.,(3,3),(-1.,0.),.UNSPECIFIED.);
#1459=B_SPLINE_CURVE_WITH_KNOTS('',2,(#65595,#65596,#65597),
 .UNSPECIFIED.,.F.,.F.,(3,3),(0.,1.),.UNSPECIFIED.);
#1460=B_SPLINE_CURVE_WITH_KNOTS('',2,(#65599,#65600,#65601),
 .UNSPECIFIED.,.F.,.F.,(3,3),(-1.,0.),.UNSPECIFIED.);
#1461=B_SPLINE_CURVE_WITH_KNOTS('',2,(#65610,#65611,#65612),
 .UNSPECIFIED.,.F.,.F.,(3,3),(0.,1.),.UNSPECIFIED.);
#1462=B_SPLINE_CURVE_WITH_KNOTS('',2,(#65614,#65615,#65616),
 .UNSPECIFIED.,.F.,.F.,(3,3),(-1.,0.),.UNSPECIFIED.);
#1463=B_SPLINE_CURVE_WITH_KNOTS('',2,(#65625,#65626,#65627),
 .UNSPECIFIED.,.F.,.F.,(3,3),(0.,1.),.UNSPECIFIED.);
#1464=B_SPLINE_CURVE_WITH_KNOTS('',2,(#65629,#65630,#65631),
 .UNSPECIFIED.,.F.,.F.,(3,3),(-1.,0.),.UNSPECIFIED.);
#1465=B_SPLINE_CURVE_WITH_KNOTS('',2,(#65640,#65641,#65642),
 .UNSPECIFIED.,.F.,.F.,(3,3),(0.,1.),.UNSPECIFIED.);
#1466=B_SPLINE_CURVE_WITH_KNOTS('',2,(#65644,#65645,#65646),
 .UNSPECIFIED.,.F.,.F.,(3,3),(-1.,0.),.UNSPECIFIED.);
#1467=B_SPLINE_CURVE_WITH_KNOTS('',2,(#65655,#65656,#65657),
 .UNSPECIFIED.,.F.,.F.,(3,3),(0.,1.),.UNSPECIFIED.);
#1468=B_SPLINE_CURVE_WITH_KNOTS('',2,(#65659,#65660,#65661),
 .UNSPECIFIED.,.F.,.F.,(3,3),(-1.,0.),.UNSPECIFIED.);
#1469=B_SPLINE_CURVE_WITH_KNOTS('',2,(#65670,#65671,#65672),
 .UNSPECIFIED.,.F.,.F.,(3,3),(0.,1.),.UNSPECIFIED.);
#1470=B_SPLINE_CURVE_WITH_KNOTS('',2,(#65674,#65675,#65676),
 .UNSPECIFIED.,.F.,.F.,(3,3),(-1.,0.),.UNSPECIFIED.);
#1471=B_SPLINE_CURVE_WITH_KNOTS('',2,(#65684,#65685,#65686),
 .UNSPECIFIED.,.F.,.F.,(3,3),(0.,1.),.UNSPECIFIED.);
#1472=B_SPLINE_CURVE_WITH_KNOTS('',2,(#65687,#65688,#65689),
 .UNSPECIFIED.,.F.,.F.,(3,3),(-1.,0.),.UNSPECIFIED.);
#1473=B_SPLINE_CURVE_WITH_KNOTS('',2,(#65699,#65700,#65701),
 .UNSPECIFIED.,.F.,.F.,(3,3),(-1.,0.),.UNSPECIFIED.);
#1474=B_SPLINE_CURVE_WITH_KNOTS('',2,(#65710,#65711,#65712),
 .UNSPECIFIED.,.F.,.F.,(3,3),(-1.,0.),.UNSPECIFIED.);
#1475=B_SPLINE_CURVE_WITH_KNOTS('',2,(#65721,#65722,#65723),
 .UNSPECIFIED.,.F.,.F.,(3,3),(-1.,0.),.UNSPECIFIED.);
#1476=B_SPLINE_CURVE_WITH_KNOTS('',2,(#65732,#65733,#65734),
 .UNSPECIFIED.,.F.,.F.,(3,3),(-1.,0.),.UNSPECIFIED.);
#1477=B_SPLINE_CURVE_WITH_KNOTS('',2,(#65743,#65744,#65745),
 .UNSPECIFIED.,.F.,.F.,(3,3),(-1.,0.),.UNSPECIFIED.);
#1478=B_SPLINE_CURVE_WITH_KNOTS('',2,(#65754,#65755,#65756),
 .UNSPECIFIED.,.F.,.F.,(3,3),(-1.,0.),.UNSPECIFIED.);
#1479=B_SPLINE_CURVE_WITH_KNOTS('',2,(#65765,#65766,#65767),
 .UNSPECIFIED.,.F.,.F.,(3,3),(-1.,0.),.UNSPECIFIED.);
#1480=B_SPLINE_CURVE_WITH_KNOTS('',2,(#65776,#65777,#65778),
 .UNSPECIFIED.,.F.,.F.,(3,3),(-1.,0.),.UNSPECIFIED.);
#1481=B_SPLINE_CURVE_WITH_KNOTS('',2,(#65787,#65788,#65789),
 .UNSPECIFIED.,.F.,.F.,(3,3),(-1.,0.),.UNSPECIFIED.);
#1482=B_SPLINE_CURVE_WITH_KNOTS('',2,(#65797,#65798,#65799),
 .UNSPECIFIED.,.F.,.F.,(3,3),(-1.,0.),.UNSPECIFIED.);
#1483=B_SPLINE_CURVE_WITH_KNOTS('',3,(#66006,#66007,#66008,#66009,#66010,
#66011,#66012,#66013,#66014,#66015,#66016,#66017,#66018,#66019,#66020,#66021),
 .UNSPECIFIED.,.F.,.F.,(4,3,3,3,3,4),(-4.09293042013066,-3.98155737307842,
-3.48386270144362,-2.98616802980881,-2.48847335817401,-2.07498647268397),
 .UNSPECIFIED.);
#1484=B_SPLINE_CURVE_WITH_KNOTS('',3,(#66024,#66025,#66026,#66027,#66028,
#66029,#66030,#66031,#66032,#66033),.UNSPECIFIED.,.F.,.F.,(4,3,3,4),(0.,
0.497694671634796,0.995389343269607,1.12364870614303),.UNSPECIFIED.);
#1485=B_SPLINE_CURVE_WITH_KNOTS('',3,(#66038,#66039,#66040,#66041,#66042,
#66043,#66044,#66045,#66046,#66047,#66048,#66049,#66050,#66051,#66052,#66053,
#66054,#66055,#66056,#66057,#66058,#66059,#66060,#66061,#66062,#66063,#66064,
#66065,#66066,#66067,#66068,#66069,#66070,#66071,#66072,#66073,#66074,#66075,
#66076,#66077),.UNSPECIFIED.,.F.,.F.,(4,3,3,3,3,3,3,3,3,3,3,3,3,4),(-10.3761157273103,
-9.95389343269604,-9.45619876106124,-8.95850408942644,-8.46080941779164,
-7.96311474615684,-7.46542007452203,-6.96772540288723,-6.47003073125243,
-5.97233605961763,-5.47464138798282,-4.97694671634802,-4.47925204471322,
-4.09293042013066),.UNSPECIFIED.);
#1486=B_SPLINE_CURVE_WITH_KNOTS('',3,(#66078,#66079,#66080,#66081,#66082,
#66083,#66084,#66085,#66086,#66087,#66088,#66089,#66090,#66091,#66092,#66093,
#66094,#66095,#66096,#66097,#66098,#66099,#66100,#66101,#66102,#66103,#66104,
#66105,#66106,#66107,#66108,#66109,#66110,#66111,#66112,#66113,#66114,#66115,
#66116,#66117),.UNSPECIFIED.,.F.,.F.,(4,3,3,3,3,3,3,3,3,3,3,3,3,4),(1.12364870614303,
1.49308401490441,1.99077868653921,2.48847335817401,2.98616802980882,3.48386270144362,
3.98155737307842,4.47925204471322,4.97694671634802,5.47464138798283,5.97233605961763,
6.47003073125243,6.96772540288723,7.40683401332262),.UNSPECIFIED.);
#1487=B_SPLINE_CURVE_WITH_KNOTS('',3,(#66122,#66123,#66124,#66125,#66126,
#66127,#66128,#66129,#66130,#66131,#66132,#66133,#66134,#66135,#66136,#66137,
#66138,#66139,#66140,#66141,#66142,#66143,#66144,#66145,#66146,#66147,#66148,
#66149,#66150,#66151,#66152,#66153,#66154,#66155,#66156,#66157,#66158,#66159,
#66160,#66161,#66162,#66163,#66164),.UNSPECIFIED.,.F.,.F.,(4,3,3,3,3,3,
3,3,3,3,3,3,3,3,4),(-16.6593010344898,-16.4239241639485,-15.9262294923137,
-15.4285348206789,-14.9308401490441,-14.4331454774093,-13.9354508057745,
-13.4377561341397,-12.9400614625049,-12.4423667908701,-11.9446721192353,
-11.4469774476004,-10.9492827759657,-10.4515881043308,-10.3761157273103),
 .UNSPECIFIED.);
#1488=B_SPLINE_CURVE_WITH_KNOTS('',3,(#66165,#66166,#66167,#66168,#66169,
#66170,#66171,#66172,#66173,#66174,#66175,#66176,#66177,#66178,#66179,#66180,
#66181,#66182,#66183,#66184,#66185,#66186,#66187,#66188,#66189,#66190,#66191,
#66192,#66193,#66194,#66195,#66196,#66197,#66198,#66199,#66200,#66201,#66202,
#66203,#66204,#66205,#66206,#66207),.UNSPECIFIED.,.F.,.F.,(4,3,3,3,3,3,
3,3,3,3,3,3,3,3,4),(7.40683401332262,7.46542007452203,7.96311474615683,
8.46080941779163,8.95850408942644,9.45619876106124,9.95389343269604,10.4515881043308,
10.9492827759656,11.4469774476004,11.9446721192352,12.44236679087,12.9400614625048,
13.4377561341397,13.6900193205022),.UNSPECIFIED.);
#1489=B_SPLINE_CURVE_WITH_KNOTS('',3,(#66212,#66213,#66214,#66215,#66216,
#66217,#66218,#66219,#66220,#66221,#66222,#66223,#66224,#66225,#66226,#66227,
#66228,#66229,#66230,#66231,#66232,#66233,#66234,#66235,#66236,#66237,#66238,
#66239,#66240,#66241,#66242,#66243,#66244,#66245,#66246,#66247,#66248,#66249,
#66250,#66251,#66252,#66253,#66254),.UNSPECIFIED.,.F.,.F.,(4,3,3,3,3,3,
3,3,3,3,3,3,3,3,4),(-22.9424863416694,-22.8939548952009,-22.3962602235661,
-21.8985655519313,-21.4008708802965,-20.9031762086617,-20.4054815370269,
-19.9077868653921,-19.4100921937573,-18.9123975221225,-18.4147028504877,
-17.9170081788529,-17.4193135072181,-16.9216188355833,-16.6593010344898),
 .UNSPECIFIED.);
#1490=B_SPLINE_CURVE_WITH_KNOTS('',3,(#66255,#66256,#66257,#66258,#66259,
#66260,#66261,#66262,#66263,#66264,#66265,#66266,#66267,#66268,#66269,#66270,
#66271,#66272,#66273,#66274,#66275,#66276,#66277,#66278,#66279,#66280,#66281,
#66282,#66283,#66284,#66285,#66286,#66287,#66288,#66289,#66290,#66291,#66292,
#66293,#66294,#66295,#66296,#66297),.UNSPECIFIED.,.F.,.F.,(4,3,3,3,3,3,
3,3,3,3,3,3,3,3,4),(13.6900193205022,13.9354508057745,14.4331454774093,
14.9308401490441,15.4285348206789,15.9262294923137,16.4239241639485,16.9216188355833,
17.4193135072181,17.9170081788529,18.4147028504877,18.9123975221225,19.4100921937573,
19.9077868653921,19.9732046276818),.UNSPECIFIED.);
#1491=B_SPLINE_CURVE_WITH_KNOTS('',3,(#66302,#66303,#66304,#66305,#66306,
#66307,#66308,#66309,#66310,#66311,#66312,#66313,#66314,#66315,#66316,#66317,
#66318,#66319,#66320,#66321,#66322,#66323,#66324,#66325,#66326,#66327,#66328,
#66329,#66330,#66331,#66332,#66333,#66334,#66335,#66336,#66337,#66338,#66339,
#66340,#66341),.UNSPECIFIED.,.F.,.F.,(4,3,3,3,3,3,3,3,3,3,3,3,3,4),(-29.225671648849,
-28.8662909548185,-28.3685962831837,-27.8709016115489,-27.3732069399141,
-26.8755122682793,-26.3778175966445,-25.8801229250097,-25.3824282533749,
-24.8847335817401,-24.3870389101053,-23.8893442384705,-23.3916495668357,
-22.9424863416694),.UNSPECIFIED.);
#1492=B_SPLINE_CURVE_WITH_KNOTS('',3,(#66342,#66343,#66344,#66345,#66346,
#66347,#66348,#66349,#66350,#66351,#66352,#66353,#66354,#66355,#66356,#66357,
#66358,#66359,#66360,#66361,#66362,#66363,#66364,#66365,#66366,#66367,#66368,
#66369,#66370,#66371,#66372,#66373,#66374,#66375,#66376,#66377,#66378,#66379,
#66380,#66381),.UNSPECIFIED.,.F.,.F.,(4,3,3,3,3,3,3,3,3,3,3,3,3,4),(19.9732046276818,
20.4054815370269,20.9031762086617,21.4008708802965,21.8985655519313,22.3962602235661,
22.8939548952009,23.3916495668357,23.8893442384705,24.3870389101053,24.8847335817401,
25.3824282533749,25.8801229250097,26.2563899348614),.UNSPECIFIED.);
#1493=B_SPLINE_CURVE_WITH_KNOTS('',3,(#66386,#66387,#66388,#66389,#66390,
#66391,#66392,#66393,#66394,#66395,#66396,#66397,#66398,#66399,#66400,#66401,
#66402,#66403,#66404,#66405,#66406,#66407,#66408,#66409,#66410,#66411,#66412,
#66413,#66414,#66415,#66416,#66417,#66418,#66419,#66420,#66421,#66422,#66423,
#66424,#66425,#66426,#66427,#66428),.UNSPECIFIED.,.F.,.F.,(4,3,3,3,3,3,
3,3,3,3,3,3,3,3,4),(-35.5088569560286,-35.336321686071,-34.8386270144361,
-34.3409323428013,-33.8432376711666,-33.3455429995317,-32.8478483278969,
-32.3501536562621,-31.8524589846273,-31.3547643129925,-30.8570696413577,
-30.3593749697229,-29.8616802980881,-29.3639856264533,-29.225671648849),
 .UNSPECIFIED.);
#1494=B_SPLINE_CURVE_WITH_KNOTS('',3,(#66429,#66430,#66431,#66432,#66433,
#66434,#66435,#66436,#66437,#66438,#66439,#66440,#66441,#66442,#66443,#66444,
#66445,#66446,#66447,#66448,#66449,#66450,#66451,#66452,#66453,#66454,#66455,
#66456,#66457,#66458,#66459,#66460,#66461,#66462,#66463,#66464,#66465,#66466,
#66467,#66468,#66469,#66470,#66471),.UNSPECIFIED.,.F.,.F.,(4,3,3,3,3,3,
3,3,3,3,3,3,3,3,4),(26.2563899348614,26.3778175966445,26.8755122682793,
27.3732069399141,27.8709016115489,28.3685962831837,28.8662909548185,29.3639856264533,
29.8616802980881,30.3593749697229,30.8570696413577,31.3547643129925,31.8524589846273,
32.3501536562621,32.539575242041),.UNSPECIFIED.);
#1495=B_SPLINE_CURVE_WITH_KNOTS('',3,(#66476,#66477,#66478,#66479,#66480,
#66481,#66482,#66483,#66484,#66485,#66486,#66487,#66488,#66489,#66490,#66491,
#66492,#66493,#66494,#66495,#66496,#66497,#66498,#66499,#66500,#66501,#66502,
#66503,#66504,#66505,#66506,#66507,#66508,#66509,#66510,#66511,#66512,#66513,
#66514,#66515),.UNSPECIFIED.,.F.,.F.,(4,3,3,3,3,3,3,3,3,3,3,3,3,4),(-41.7920422632082,
-41.3086577456886,-40.8109630740538,-40.313268402419,-39.8155737307842,
-39.3178790591494,-38.8201843875146,-38.3224897158798,-37.824795044245,
-37.3271003726102,-36.8294057009754,-36.3317110293406,-35.8340163577058,
-35.5088569560286),.UNSPECIFIED.);
#1496=B_SPLINE_CURVE_WITH_KNOTS('',3,(#66516,#66517,#66518,#66519,#66520,
#66521,#66522,#66523,#66524,#66525,#66526,#66527,#66528,#66529,#66530,#66531,
#66532,#66533,#66534,#66535,#66536,#66537,#66538,#66539,#66540,#66541,#66542,
#66543,#66544,#66545,#66546,#66547,#66548,#66549,#66550,#66551,#66552,#66553,
#66554,#66555,#66556,#66557,#66558),.UNSPECIFIED.,.F.,.F.,(4,3,3,3,3,3,
3,3,3,3,3,3,3,3,4),(32.539575242041,32.8478483278969,33.3455429995317,33.8432376711665,
34.3409323428013,34.8386270144361,35.336321686071,35.8340163577058,36.3317110293406,
36.8294057009754,37.3271003726102,37.824795044245,38.3224897158798,38.8201843875146,
38.8227605492206),.UNSPECIFIED.);
#1497=B_SPLINE_CURVE_WITH_KNOTS('',3,(#66563,#66564,#66565,#66566,#66567,
#66568,#66569,#66570,#66571,#66572,#66573,#66574,#66575,#66576,#66577,#66578,
#66579,#66580,#66581,#66582,#66583,#66584,#66585,#66586,#66587,#66588,#66589,
#66590,#66591,#66592,#66593,#66594,#66595,#66596,#66597,#66598,#66599,#66600,
#66601,#66602,#66603,#66604,#66605),.UNSPECIFIED.,.F.,.F.,(4,3,3,3,3,3,
3,3,3,3,3,3,3,3,4),(-48.0752275703878,-47.778688476941,-47.2809938053062,
-46.7832991336714,-46.2856044620366,-45.7879097904018,-45.290215118767,
-44.7925204471322,-44.2948257754974,-43.7971311038626,-43.2994364322278,
-42.801741760593,-42.3040470889582,-41.8063524173234,-41.7920422632082),
 .UNSPECIFIED.);
#1498=B_SPLINE_CURVE_WITH_KNOTS('',3,(#66606,#66607,#66608,#66609,#66610,
#66611,#66612,#66613,#66614,#66615,#66616,#66617,#66618,#66619,#66620,#66621,
#66622,#66623,#66624,#66625,#66626,#66627,#66628,#66629,#66630,#66631,#66632,
#66633,#66634,#66635,#66636,#66637,#66638,#66639,#66640,#66641,#66642,#66643,
#66644,#66645),.UNSPECIFIED.,.F.,.F.,(4,3,3,3,3,3,3,3,3,3,3,3,3,4),(38.8227605492206,
39.3178790591494,39.8155737307842,40.313268402419,40.8109630740538,41.3086577456886,
41.8063524173234,42.3040470889582,42.801741760593,43.2994364322278,43.7971311038626,
44.2948257754974,44.7925204471322,45.1059458564002),.UNSPECIFIED.);
#1499=B_SPLINE_CURVE_WITH_KNOTS('',3,(#66650,#66651,#66652,#66653,#66654,
#66655,#66656,#66657,#66658,#66659,#66660,#66661,#66662,#66663,#66664,#66665,
#66666,#66667,#66668,#66669,#66670,#66671,#66672,#66673,#66674,#66675,#66676,
#66677,#66678,#66679,#66680,#66681,#66682,#66683,#66684,#66685,#66686,#66687,
#66688,#66689,#66690,#66691,#66692),.UNSPECIFIED.,.F.,.F.,(4,3,3,3,3,3,
3,3,3,3,3,3,3,3,4),(-54.3584128775674,-54.2487192081934,-53.7510245365586,
-53.2533298649238,-52.755635193289,-52.2579405216542,-51.7602458500194,
-51.2625511783846,-50.7648565067498,-50.267161835115,-49.7694671634802,
-49.2717724918454,-48.7740778202106,-48.2763831485758,-48.0752275703878),
 .UNSPECIFIED.);
#1500=B_SPLINE_CURVE_WITH_KNOTS('',3,(#66693,#66694,#66695,#66696,#66697,
#66698,#66699,#66700,#66701,#66702,#66703,#66704,#66705,#66706,#66707,#66708,
#66709,#66710,#66711,#66712,#66713,#66714,#66715,#66716,#66717,#66718,#66719,
#66720,#66721,#66722,#66723,#66724,#66725,#66726,#66727,#66728,#66729,#66730,
#66731,#66732,#66733,#66734,#66735),.UNSPECIFIED.,.F.,.F.,(4,3,3,3,3,3,
3,3,3,3,3,3,3,3,4),(45.1059458564002,45.290215118767,45.7879097904018,46.2856044620366,
46.7832991336714,47.2809938053062,47.778688476941,48.2763831485758,48.7740778202106,
49.2717724918454,49.7694671634802,50.267161835115,50.7648565067498,51.2625511783846,
51.3891311635797),.UNSPECIFIED.);
#1501=B_SPLINE_CURVE_WITH_KNOTS('',3,(#66740,#66741,#66742,#66743,#66744,
#66745,#66746,#66747,#66748,#66749,#66750,#66751,#66752,#66753,#66754,#66755,
#66756,#66757,#66758,#66759,#66760,#66761,#66762,#66763,#66764,#66765,#66766,
#66767,#66768,#66769,#66770,#66771,#66772,#66773,#66774,#66775,#66776,#66777,
#66778,#66779),.UNSPECIFIED.,.F.,.F.,(4,3,3,3,3,3,3,3,3,3,3,3,3,4),(-60.641598184747,
-60.2210552678111,-59.7233605961763,-59.2256659245415,-58.7279712529067,
-58.2302765812719,-57.732581909637,-57.2348872380022,-56.7371925663674,
-56.2394978947326,-55.7418032230978,-55.244108551463,-54.7464138798282,
-54.3584128775674),.UNSPECIFIED.);
#1502=B_SPLINE_CURVE_WITH_KNOTS('',3,(#66780,#66781,#66782,#66783,#66784,
#66785,#66786,#66787,#66788,#66789,#66790,#66791,#66792,#66793,#66794,#66795,
#66796,#66797,#66798,#66799,#66800,#66801,#66802,#66803,#66804,#66805,#66806,
#66807,#66808,#66809,#66810,#66811,#66812,#66813,#66814,#66815,#66816,#66817,
#66818,#66819),.UNSPECIFIED.,.F.,.F.,(4,3,3,3,3,3,3,3,3,3,3,3,3,4),(51.3891311635797,
51.7602458500194,52.2579405216542,52.755635193289,53.2533298649238,53.7510245365586,
54.2487192081934,54.7464138798282,55.244108551463,55.7418032230979,56.2394978947326,
56.7371925663674,57.2348872380022,57.6723164707593),.UNSPECIFIED.);
#1503=B_SPLINE_CURVE_WITH_KNOTS('',3,(#66824,#66825,#66826,#66827,#66828,
#66829,#66830,#66831,#66832,#66833,#66834,#66835,#66836,#66837,#66838,#66839,
#66840,#66841,#66842,#66843,#66844,#66845,#66846,#66847,#66848,#66849,#66850,
#66851,#66852,#66853,#66854,#66855,#66856,#66857,#66858,#66859,#66860,#66861,
#66862,#66863,#66864,#66865,#66866),.UNSPECIFIED.,.F.,.F.,(4,3,3,3,3,3,
3,3,3,3,3,3,3,3,4),(-66.9247834919266,-66.6910859990635,-66.1933913274287,
-65.6956966557939,-65.1980019841591,-64.7003073125243,-64.2026126408895,
-63.7049179692547,-63.2072232976199,-62.7095286259851,-62.2118339543503,
-61.7141392827155,-61.2164446110807,-60.7187499394459,-60.641598184747),
 .UNSPECIFIED.);
#1504=B_SPLINE_CURVE_WITH_KNOTS('',3,(#66867,#66868,#66869,#66870,#66871,
#66872,#66873,#66874,#66875,#66876,#66877,#66878,#66879,#66880,#66881,#66882,
#66883,#66884,#66885,#66886,#66887,#66888,#66889,#66890,#66891,#66892,#66893,
#66894,#66895,#66896,#66897,#66898,#66899,#66900,#66901,#66902,#66903,#66904,
#66905,#66906,#66907,#66908,#66909),.UNSPECIFIED.,.F.,.F.,(4,3,3,3,3,3,
3,3,3,3,3,3,3,3,4),(57.6723164707593,57.732581909637,58.2302765812718,58.7279712529066,
59.2256659245415,59.7233605961763,60.2210552678111,60.7187499394459,61.2164446110807,
61.7141392827155,62.2118339543503,62.7095286259851,63.2072232976199,63.7049179692547,
63.9555017779389),.UNSPECIFIED.);
#1505=B_SPLINE_CURVE_WITH_KNOTS('',3,(#66914,#66915,#66916,#66917,#66918,
#66919,#66920,#66921,#66922,#66923,#66924,#66925,#66926,#66927,#66928,#66929,
#66930,#66931,#66932,#66933,#66934,#66935,#66936,#66937,#66938,#66939,#66940,
#66941,#66942,#66943,#66944,#66945,#66946,#66947,#66948,#66949,#66950,#66951,
#66952,#66953,#66954,#66955,#66956),.UNSPECIFIED.,.F.,.F.,(4,3,3,3,3,3,
3,3,3,3,3,3,3,3,4),(-73.2079687991062,-73.1611167303159,-72.6634220586811,
-72.1657273870463,-71.6680327154115,-71.1703380437767,-70.6726433721419,
-70.1749487005071,-69.6772540288723,-69.1795593572375,-68.6818646856027,
-68.1841700139679,-67.6864753423331,-67.1887806706983,-66.9247834919266),
 .UNSPECIFIED.);
#1506=B_SPLINE_CURVE_WITH_KNOTS('',3,(#66957,#66958,#66959,#66960,#66961,
#66962,#66963,#66964,#66965,#66966,#66967,#66968,#66969,#66970,#66971,#66972,
#66973,#66974,#66975,#66976,#66977,#66978,#66979,#66980,#66981,#66982,#66983,
#66984,#66985,#66986,#66987,#66988,#66989,#66990,#66991,#66992,#66993,#66994,
#66995,#66996,#66997,#66998,#66999),.UNSPECIFIED.,.F.,.F.,(4,3,3,3,3,3,
3,3,3,3,3,3,3,3,4),(63.9555017779389,64.2026126408895,64.7003073125243,
65.1980019841591,65.6956966557939,66.1933913274287,66.6910859990635,67.1887806706983,
67.6864753423331,68.1841700139679,68.6818646856027,69.1795593572375,69.6772540288723,
70.1749487005071,70.2386870851185),.UNSPECIFIED.);
#1507=B_SPLINE_CURVE_WITH_KNOTS('',3,(#67004,#67005,#67006,#67007,#67008,
#67009,#67010,#67011,#67012,#67013,#67014,#67015,#67016,#67017,#67018,#67019,
#67020,#67021,#67022,#67023,#67024,#67025,#67026,#67027,#67028,#67029,#67030,
#67031,#67032,#67033,#67034,#67035,#67036,#67037,#67038,#67039,#67040,#67041,
#67042,#67043),.UNSPECIFIED.,.F.,.F.,(4,3,3,3,3,3,3,3,3,3,3,3,3,4),(-79.4911541062858,
-79.1334527899335,-78.6357581182987,-78.1380634466639,-77.6403687750291,
-77.1426741033943,-76.6449794317595,-76.1472847601247,-75.6495900884899,
-75.1518954168551,-74.6542007452203,-74.1565060735855,-73.6588114019507,
-73.2079687991062),.UNSPECIFIED.);
#1508=B_SPLINE_CURVE_WITH_KNOTS('',3,(#67044,#67045,#67046,#67047,#67048,
#67049,#67050,#67051,#67052,#67053,#67054,#67055,#67056,#67057,#67058,#67059,
#67060,#67061,#67062,#67063,#67064,#67065,#67066,#67067,#67068,#67069,#67070,
#67071,#67072,#67073,#67074,#67075,#67076,#67077,#67078,#67079,#67080,#67081,
#67082,#67083),.UNSPECIFIED.,.F.,.F.,(4,3,3,3,3,3,3,3,3,3,3,3,3,4),(70.2386870851185,
70.6726433721419,71.1703380437767,71.6680327154115,72.1657273870463,72.6634220586811,
73.1611167303159,73.6588114019507,74.1565060735855,74.6542007452203,75.1518954168551,
75.6495900884899,76.1472847601247,76.5218723922981),.UNSPECIFIED.);
#1509=B_SPLINE_CURVE_WITH_KNOTS('',3,(#67088,#67089,#67090,#67091,#67092,
#67093,#67094,#67095,#67096,#67097,#67098,#67099,#67100,#67101,#67102,#67103,
#67104,#67105,#67106,#67107,#67108,#67109,#67110,#67111,#67112,#67113,#67114,
#67115,#67116,#67117,#67118,#67119,#67120,#67121,#67122,#67123,#67124,#67125,
#67126,#67127,#67128,#67129,#67130),.UNSPECIFIED.,.F.,.F.,(4,3,3,3,3,3,
3,3,3,3,3,3,3,3,4),(-85.7743394134654,-85.603483521186,-85.1057888495512,
-84.6080941779164,-84.1103995062816,-83.6127048346468,-83.115010163012,
-82.6173154913772,-82.1196208197424,-81.6219261481075,-81.1242314764727,
-80.6265368048379,-80.1288421332031,-79.6311474615683,-79.4911541062858),
 .UNSPECIFIED.);
#1510=B_SPLINE_CURVE_WITH_KNOTS('',3,(#67131,#67132,#67133,#67134,#67135,
#67136,#67137,#67138,#67139,#67140,#67141,#67142,#67143,#67144,#67145,#67146,
#67147,#67148,#67149,#67150,#67151,#67152,#67153,#67154,#67155,#67156,#67157,
#67158,#67159,#67160,#67161,#67162,#67163,#67164,#67165,#67166,#67167,#67168,
#67169,#67170,#67171,#67172,#67173),.UNSPECIFIED.,.F.,.F.,(4,3,3,3,3,3,
3,3,3,3,3,3,3,3,4),(76.5218723922981,76.6449794317595,77.1426741033943,
77.6403687750291,78.1380634466639,78.6357581182987,79.1334527899335,79.6311474615683,
80.1288421332031,80.6265368048379,81.1242314764728,81.6219261481075,82.1196208197423,
82.6173154913771,82.8050576994777),.UNSPECIFIED.);
#1511=B_SPLINE_CURVE_WITH_KNOTS('',3,(#67180,#67181,#67182,#67183,#67184,
#67185,#67186,#67187,#67188,#67189,#67190,#67191,#67192,#67193,#67194,#67195,
#67196,#67197,#67198,#67199,#67200,#67201,#67202,#67203,#67204,#67205,#67206,
#67207,#67208,#67209,#67210,#67211,#67212,#67213,#67214,#67215,#67216),
 .UNSPECIFIED.,.F.,.F.,(4,3,3,3,3,3,3,3,3,3,3,3,4),(-91.5758195808036,-91.0781249091688,
-90.580430237534,-90.0827355658992,-89.5850408942644,-89.0873462226296,
-88.5896515509948,-88.09195687936,-87.5942622077252,-87.0965675360904,-86.5988728644556,
-86.1011781928208,-85.7743394134654),.UNSPECIFIED.);
#1512=B_SPLINE_CURVE_WITH_KNOTS('',3,(#67217,#67218,#67219,#67220,#67221,
#67222,#67223,#67224,#67225,#67226,#67227,#67228,#67229,#67230,#67231,#67232,
#67233,#67234,#67235,#67236,#67237,#67238,#67239,#67240,#67241,#67242,#67243,
#67244,#67245,#67246,#67247,#67248,#67249,#67250,#67251,#67252,#67253,#67254,
#67255,#67256),.UNSPECIFIED.,.F.,.F.,(4,3,3,3,3,3,3,3,3,3,3,3,3,4),(82.8050576994777,
83.1150101630119,83.6127048346467,84.1103995062816,84.6080941779164,85.1057888495512,
85.603483521186,86.1011781928208,86.5988728644556,87.0965675360904,87.5942622077252,
88.09195687936,88.5896515509948,89.0882430066573),.UNSPECIFIED.);
#1513=B_SPLINE_CURVE_WITH_KNOTS('',3,(#67262,#67263,#67264,#67265,#67266,
#67267,#67268,#67269,#67270,#67271,#67272),.UNSPECIFIED.,.F.,.F.,(4,1,1,
1,1,1,1,1,4),(97.3893722612836,97.716211040639,98.2139057122738,98.7116003839086,
99.2092950555434,99.7069897271782,100.204684398813,100.702379070448,101.115865955938),
 .UNSPECIFIED.);
#1514=B_SPLINE_CURVE_WITH_KNOTS('',3,(#67275,#67276,#67277,#67278,#67279,
#67280,#67281,#67282),.UNSPECIFIED.,.F.,.F.,(4,1,1,1,1,4),(97.3893722612836,
97.8861701488906,98.3838648205254,98.8815594921602,99.379254163795,99.8769488354298),
 .UNSPECIFIED.);
#1515=B_SPLINE_CURVE_WITH_KNOTS('',3,(#67287,#67288,#67289,#67290,#67291,
#67292,#67293,#67294,#67295,#67296,#67297,#67298,#67299,#67300,#67301,#67302,
#67303),.UNSPECIFIED.,.F.,.F.,(4,1,1,1,1,1,1,1,1,1,1,1,1,1,4),(91.106186954104,
91.2461803093866,91.7438749810213,92.2415696526562,92.739264324291,93.2369589959258,
93.7346536675606,94.2323483391954,94.7300430108302,95.227737682465,95.7254323540998,
96.2231270257346,96.7208216973694,97.2185163690042,97.3893722612836),
 .UNSPECIFIED.);
#1516=B_SPLINE_CURVE_WITH_KNOTS('',3,(#67304,#67305,#67306,#67307,#67308,
#67309,#67310,#67311,#67312,#67313,#67314,#67315,#67316,#67317,#67318,#67319,
#67320),.UNSPECIFIED.,.F.,.F.,(4,1,1,1,1,1,1,1,1,1,1,1,1,1,4),(91.106186954104,
91.4161394176381,91.9138340892729,92.4115287609077,92.9092234325425,93.4069181041774,
93.9046127758121,94.4023074474469,94.9000021190817,95.3976967907166,95.8953914623514,
96.3930861339862,96.890780805621,97.3884754772558,97.3893722612836),
 .UNSPECIFIED.);
#1517=B_SPLINE_CURVE_WITH_KNOTS('',3,(#67325,#67326,#67327,#67328,#67329,
#67330,#67331,#67332,#67333,#67334,#67335,#67336,#67337,#67338,#67339,#67340),
 .UNSPECIFIED.,.F.,.F.,(4,1,1,1,1,1,1,1,1,1,1,1,1,4),(84.8230016469244,
85.2738442497689,85.7715389214037,86.2692335930385,86.7669282646733,87.2646229363081,
87.7623176079429,88.2600122795777,88.7577069512125,89.2554016228473,89.7530962944821,
90.250790966117,90.7484856377518,91.106186954104),.UNSPECIFIED.);
#1518=B_SPLINE_CURVE_WITH_KNOTS('',3,(#67341,#67342,#67343,#67344,#67345,
#67346,#67347,#67348,#67349,#67350,#67351,#67352,#67353,#67354,#67355,#67356,
#67357),.UNSPECIFIED.,.F.,.F.,(4,1,1,1,1,1,1,1,1,1,1,1,1,1,4),(84.8230016469244,
84.9461086863857,85.4438033580205,85.9414980296553,86.4391927012901,86.9368873729249,
87.4345820445597,87.9322767161945,88.4299713878293,88.9276660594641,89.4253607310989,
89.9230554027337,90.4207500743685,90.9184447460033,91.106186954104),
 .UNSPECIFIED.);
#1519=B_SPLINE_CURVE_WITH_KNOTS('',3,(#67362,#67363,#67364,#67365,#67366,
#67367,#67368,#67369,#67370,#67371,#67372,#67373,#67374,#67375,#67376,#67377,
#67378),.UNSPECIFIED.,.F.,.F.,(4,1,1,1,1,1,1,1,1,1,1,1,1,1,4),(78.5398163397448,
78.8038135185165,79.3015081901513,79.7992028617861,80.2968975334209,80.7945922050557,
81.2922868766905,81.7899815483253,82.2876762199601,82.7853708915949,83.2830655632297,
83.7807602348645,84.2784549064993,84.7761495781341,84.8230016469244),
 .UNSPECIFIED.);
#1520=B_SPLINE_CURVE_WITH_KNOTS('',3,(#67379,#67380,#67381,#67382,#67383,
#67384,#67385,#67386,#67387,#67388,#67389,#67390,#67391,#67392,#67393,#67394),
 .UNSPECIFIED.,.F.,.F.,(4,1,1,1,1,1,1,1,1,1,1,1,1,4),(78.5398163397448,
78.9737726267681,79.4714672984029,79.9691619700377,80.4668566416725,80.9645513133073,
81.4622459849421,81.9599406565769,82.4576353282117,82.9553299998465,83.4530246714813,
83.9507193431161,84.4484140147509,84.8230016469244),.UNSPECIFIED.);
#1521=B_SPLINE_CURVE_WITH_KNOTS('',3,(#67399,#67400,#67401,#67402,#67403,
#67404,#67405,#67406,#67407,#67408,#67409,#67410,#67411,#67412,#67413,#67414,
#67415),.UNSPECIFIED.,.F.,.F.,(4,1,1,1,1,1,1,1,1,1,1,1,1,1,4),(72.2566310325652,
72.3337827872641,72.8314774588989,73.3291721305337,73.8268668021685,74.3245614738033,
74.8222561454381,75.3199508170729,75.8176454887077,76.3153401603425,76.8130348319773,
77.3107295036121,77.8084241752469,78.3061188468817,78.5398163397448),
 .UNSPECIFIED.);
#1522=B_SPLINE_CURVE_WITH_KNOTS('',3,(#67416,#67417,#67418,#67419,#67420,
#67421,#67422,#67423,#67424,#67425,#67426,#67427,#67428,#67429,#67430,#67431,
#67432),.UNSPECIFIED.,.F.,.F.,(4,1,1,1,1,1,1,1,1,1,1,1,1,1,4),(72.2566310325652,
72.5037418955157,73.0014365671505,73.4991312387853,73.9968259104201,74.4945205820549,
74.9922152536897,75.4899099253245,75.9876045969593,76.4852992685941,76.9829939402289,
77.4806886118637,77.9783832834985,78.4760779551333,78.5398163397448),
 .UNSPECIFIED.);
#1523=B_SPLINE_CURVE_WITH_KNOTS('',3,(#67437,#67438,#67439,#67440,#67441,
#67442,#67443,#67444,#67445,#67446,#67447,#67448,#67449,#67450,#67451,#67452),
 .UNSPECIFIED.,.F.,.F.,(4,1,1,1,1,1,1,1,1,1,1,1,1,4),(65.9734457253856,
66.3614467276465,66.8591413992813,67.3568360709161,67.8545307425508,68.3522254141857,
68.8499200858205,69.3476147574553,69.8453094290901,70.3430041007249,70.8406987723597,
71.3383934439945,71.8360881156293,72.2566310325652),.UNSPECIFIED.);
#1524=B_SPLINE_CURVE_WITH_KNOTS('',3,(#67453,#67454,#67455,#67456,#67457,
#67458,#67459,#67460,#67461,#67462,#67463,#67464,#67465,#67466,#67467,#67468,
#67469),.UNSPECIFIED.,.F.,.F.,(4,1,1,1,1,1,1,1,1,1,1,1,1,1,4),(65.9734457253856,
66.0337111642632,66.531405835898,67.0291005075328,67.5267951791676,68.0244898508024,
68.5221845224372,69.019879194072,69.5175738657069,70.0152685373416,70.5129632089764,
71.0106578806112,71.5083525522461,72.0060472238809,72.2566310325652),
 .UNSPECIFIED.);
#1525=B_SPLINE_CURVE_WITH_KNOTS('',3,(#67474,#67475,#67476,#67477,#67478,
#67479,#67480,#67481,#67482,#67483,#67484,#67485,#67486,#67487,#67488,#67489,
#67490),.UNSPECIFIED.,.F.,.F.,(4,1,1,1,1,1,1,1,1,1,1,1,1,1,4),(59.690260418206,
59.891415996394,60.3891106680288,60.8868053396636,61.3845000112984,61.8821946829332,
62.379889354568,62.8775840262028,63.3752786978376,63.8729733694724,64.3706680411072,
64.868362712742,65.3660573843768,65.8637520560116,65.9734457253856),
 .UNSPECIFIED.);
#1526=B_SPLINE_CURVE_WITH_KNOTS('',3,(#67491,#67492,#67493,#67494,#67495,
#67496,#67497,#67498,#67499,#67500,#67501,#67502,#67503,#67504,#67505,#67506),
 .UNSPECIFIED.,.F.,.F.,(4,1,1,1,1,1,1,1,1,1,1,1,1,4),(59.690260418206,60.0613751046456,
60.5590697762804,61.0567644479152,61.55445911955,62.0521537911848,62.5498484628196,
63.0475431344544,63.5452378060892,64.042932477724,64.5406271493588,65.0383218209936,
65.5360164926284,65.9734457253856),.UNSPECIFIED.);
#1527=B_SPLINE_CURVE_WITH_KNOTS('',3,(#67511,#67512,#67513,#67514,#67515,
#67516,#67517,#67518,#67519,#67520,#67521,#67522,#67523,#67524,#67525,#67526,
#67527),.UNSPECIFIED.,.F.,.F.,(4,1,1,1,1,1,1,1,1,1,1,1,1,1,4),(53.4070751110264,
53.4213852651416,53.9190799367764,54.4167746084112,54.914469280046,55.4121639516808,
55.9098586233156,56.4075532949504,56.9052479665852,57.40294263822,57.9006373098548,
58.3983319814896,58.8960266531244,59.3937213247592,59.690260418206),
 .UNSPECIFIED.);
#1528=B_SPLINE_CURVE_WITH_KNOTS('',3,(#67528,#67529,#67530,#67531,#67532,
#67533,#67534,#67535,#67536,#67537,#67538,#67539,#67540,#67541,#67542,#67543,
#67544),.UNSPECIFIED.,.F.,.F.,(4,1,1,1,1,1,1,1,1,1,1,1,1,1,4),(53.4070751110264,
53.5913443733932,54.089039045028,54.5867337166628,55.0844283882976,55.5821230599324,
56.0798177315672,56.577512403202,57.0752070748368,57.5729017464716,58.0705964181064,
58.5682910897412,59.065985761376,59.5636804330108,59.690260418206),
 .UNSPECIFIED.);
#1529=B_SPLINE_CURVE_WITH_KNOTS('',3,(#67549,#67550,#67551,#67552,#67553,
#67554,#67555,#67556,#67557,#67558,#67559,#67560,#67561,#67562,#67563,#67564),
 .UNSPECIFIED.,.F.,.F.,(4,1,1,1,1,1,1,1,1,1,1,1,1,4),(47.1238898038468,
47.449049205524,47.9467438771588,48.4444385487936,48.9421332204284,49.4398278920632,
49.937522563698,50.4352172353328,50.9329119069676,51.4306065786024,51.9283012502372,
52.425995921872,52.9236905935068,53.4070751110264),.UNSPECIFIED.);
#1530=B_SPLINE_CURVE_WITH_KNOTS('',3,(#67565,#67566,#67567,#67568,#67569,
#67570,#67571,#67572,#67573,#67574,#67575,#67576,#67577,#67578,#67579,#67580),
 .UNSPECIFIED.,.F.,.F.,(4,1,1,1,1,1,1,1,1,1,1,1,1,4),(47.1238898038468,
47.6190083137756,48.1167029854104,48.6143976570452,49.11209232868,49.6097870003148,
50.1074816719496,50.6051763435844,51.1028710152192,51.600565686854,52.0982603584888,
52.5959550301236,53.0936497017584,53.4070751110264),.UNSPECIFIED.);
#1531=B_SPLINE_CURVE_WITH_KNOTS('',3,(#67585,#67586,#67587,#67588,#67589,
#67590,#67591,#67592,#67593,#67594,#67595,#67596,#67597,#67598,#67599,#67600,
#67601),.UNSPECIFIED.,.F.,.F.,(4,1,1,1,1,1,1,1,1,1,1,1,1,1,4),(40.8407044966673,
40.9790184742715,41.4767131459063,41.9744078175411,42.472102489176,42.9697971608108,
43.4674918324456,43.9651865040804,44.4628811757152,44.96057584735,45.4582705189848,
45.9559651906196,46.4536598622544,46.9513545338892,47.1238898038468),
 .UNSPECIFIED.);
#1532=B_SPLINE_CURVE_WITH_KNOTS('',3,(#67602,#67603,#67604,#67605,#67606,
#67607,#67608,#67609,#67610,#67611,#67612,#67613,#67614,#67615,#67616,#67617,
#67618),.UNSPECIFIED.,.F.,.F.,(4,1,1,1,1,1,1,1,1,1,1,1,1,1,4),(40.8407044966672,
41.1489775825231,41.6466722541579,42.1443669257927,42.6420615974275,43.1397562690623,
43.6374509406971,44.1351456123319,44.6328402839667,45.1305349556015,45.6282296272363,
46.1259242988711,46.6236189705059,47.1213136421407,47.1238898038468),
 .UNSPECIFIED.);
#1533=B_SPLINE_CURVE_WITH_KNOTS('',3,(#67623,#67624,#67625,#67626,#67627,
#67628,#67629,#67630,#67631,#67632,#67633,#67634,#67635,#67636,#67637,#67638),
 .UNSPECIFIED.,.F.,.F.,(4,1,1,1,1,1,1,1,1,1,1,1,1,4),(34.5575191894877,
35.0066824146539,35.5043770862887,36.0020717579235,36.4997664295583,36.9974611011931,
37.4951557728279,37.9928504444627,38.4905451160975,38.9882397877323,39.4859344593671,
39.9836291310019,40.4813238026367,40.8407044966673),.UNSPECIFIED.);
#1534=B_SPLINE_CURVE_WITH_KNOTS('',3,(#67639,#67640,#67641,#67642,#67643,
#67644,#67645,#67646,#67647,#67648,#67649,#67650,#67651,#67652,#67653,#67654,
#67655),.UNSPECIFIED.,.F.,.F.,(4,1,1,1,1,1,1,1,1,1,1,1,1,1,4),(34.5575191894876,
34.6789468512707,35.1766415229055,35.6743361945403,36.1720308661751,36.6697255378099,
37.1674202094447,37.6651148810795,38.1628095527143,38.6605042243491,39.1581988959839,
39.6558935676187,40.1535882392535,40.6512829108883,40.8407044966672),
 .UNSPECIFIED.);
#1535=B_SPLINE_CURVE_WITH_KNOTS('',3,(#67660,#67661,#67662,#67663,#67664,
#67665,#67666,#67667,#67668,#67669,#67670,#67671,#67672,#67673,#67674,#67675,
#67676),.UNSPECIFIED.,.F.,.F.,(4,1,1,1,1,1,1,1,1,1,1,1,1,1,4),(28.2743338823081,
28.5366516834015,29.0343463550363,29.5320410266711,30.0297356983059,30.5274303699407,
31.0251250415755,31.5228197132103,32.0205143848451,32.5182090564799,33.0159037281147,
33.5135983997495,34.0112930713843,34.5089877430191,34.5575191894877),
 .UNSPECIFIED.);
#1536=B_SPLINE_CURVE_WITH_KNOTS('',3,(#67677,#67678,#67679,#67680,#67681,
#67682,#67683,#67684,#67685,#67686,#67687,#67688,#67689,#67690,#67691,#67692),
 .UNSPECIFIED.,.F.,.F.,(4,1,1,1,1,1,1,1,1,1,1,1,1,4),(28.2743338823081,
28.7066107916531,29.2043054632879,29.7020001349227,30.1996948065575,30.6973894781923,
31.1950841498271,31.6927788214619,32.1904734930967,32.6881681647315,33.1858628363663,
33.6835575080011,34.1812521796359,34.5575191894876),.UNSPECIFIED.);
#1537=B_SPLINE_CURVE_WITH_KNOTS('',3,(#67697,#67698,#67699,#67700,#67701,
#67702,#67703,#67704,#67705,#67706,#67707,#67708,#67709,#67710,#67711,#67712,
#67713),.UNSPECIFIED.,.F.,.F.,(4,1,1,1,1,1,1,1,1,1,1,1,1,1,4),(21.9911485751285,
22.0666209521491,22.5643156237839,23.0620102954187,23.5597049670535,24.0573996386883,
24.5550943103231,25.0527889819579,25.5504836535927,26.0481783252275,26.5458729968623,
27.0435676684971,27.5412623401319,28.0389570117667,28.2743338823081),
 .UNSPECIFIED.);
#1538=B_SPLINE_CURVE_WITH_KNOTS('',3,(#67714,#67715,#67716,#67717,#67718,
#67719,#67720,#67721,#67722,#67723,#67724,#67725,#67726,#67727,#67728,#67729,
#67730),.UNSPECIFIED.,.F.,.F.,(4,1,1,1,1,1,1,1,1,1,1,1,1,1,4),(21.9911485751285,
22.2365800604006,22.7342747320354,23.2319694036702,23.7296640753051,24.2273587469399,
24.7250534185747,25.2227480902095,25.7204427618443,26.2181374334791,26.7158321051139,
27.2135267767487,27.7112214483835,28.2089161200183,28.2743338823081),
 .UNSPECIFIED.);
#1539=B_SPLINE_CURVE_WITH_KNOTS('',3,(#67735,#67736,#67737,#67738,#67739,
#67740,#67741,#67742,#67743,#67744,#67745,#67746,#67747,#67748,#67749,#67750),
 .UNSPECIFIED.,.F.,.F.,(4,1,1,1,1,1,1,1,1,1,1,1,1,4),(15.7079632679489,
16.0942848925314,16.5919795641662,17.089674235801,17.5873689074358,18.0850635790706,
18.5827582507054,19.0804529223402,19.5781475939751,20.0758422656099,20.5735369372447,
21.0712316088795,21.5689262805143,21.9911485751285),.UNSPECIFIED.);
#1540=B_SPLINE_CURVE_WITH_KNOTS('',3,(#67751,#67752,#67753,#67754,#67755,
#67756,#67757,#67758,#67759,#67760,#67761,#67762,#67763,#67764,#67765,#67766,
#67767),.UNSPECIFIED.,.F.,.F.,(4,1,1,1,1,1,1,1,1,1,1,1,1,1,4),(15.7079632679489,
15.7665493291482,16.264244000783,16.7619386724178,17.2596333440526,17.7573280156874,
18.2550226873222,18.752717358957,19.2504120305918,19.7481067022266,20.2458013738614,
20.7434960454962,21.241190717131,21.7388853887658,21.9911485751285),
 .UNSPECIFIED.);
#1541=B_SPLINE_CURVE_WITH_KNOTS('',2,(#67776,#67777,#67778),
 .UNSPECIFIED.,.F.,.F.,(3,3),(0.,1.),.UNSPECIFIED.);
#1542=B_SPLINE_CURVE_WITH_KNOTS('',2,(#67782,#67783,#67784),
 .UNSPECIFIED.,.F.,.F.,(3,3),(0.,1.),.UNSPECIFIED.);
#1543=B_SPLINE_CURVE_WITH_KNOTS('',2,(#67793,#67794,#67795),
 .UNSPECIFIED.,.F.,.F.,(3,3),(0.,1.),.UNSPECIFIED.);
#1544=B_SPLINE_CURVE_WITH_KNOTS('',2,(#67798,#67799,#67800),
 .UNSPECIFIED.,.F.,.F.,(3,3),(0.,1.),.UNSPECIFIED.);
#1545=B_SPLINE_CURVE_WITH_KNOTS('',2,(#67808,#67809,#67810),
 .UNSPECIFIED.,.F.,.F.,(3,3),(0.,1.),.UNSPECIFIED.);
#1546=B_SPLINE_CURVE_WITH_KNOTS('',2,(#67813,#67814,#67815),
 .UNSPECIFIED.,.F.,.F.,(3,3),(0.,1.),.UNSPECIFIED.);
#1547=B_SPLINE_CURVE_WITH_KNOTS('',2,(#67823,#67824,#67825),
 .UNSPECIFIED.,.F.,.F.,(3,3),(0.,1.),.UNSPECIFIED.);
#1548=B_SPLINE_CURVE_WITH_KNOTS('',2,(#67828,#67829,#67830),
 .UNSPECIFIED.,.F.,.F.,(3,3),(0.,1.),.UNSPECIFIED.);
#1549=B_SPLINE_CURVE_WITH_KNOTS('',2,(#67838,#67839,#67840),
 .UNSPECIFIED.,.F.,.F.,(3,3),(0.,1.),.UNSPECIFIED.);
#1550=B_SPLINE_CURVE_WITH_KNOTS('',2,(#67843,#67844,#67845),
 .UNSPECIFIED.,.F.,.F.,(3,3),(0.,1.),.UNSPECIFIED.);
#1551=B_SPLINE_CURVE_WITH_KNOTS('',2,(#67853,#67854,#67855),
 .UNSPECIFIED.,.F.,.F.,(3,3),(0.,1.),.UNSPECIFIED.);
#1552=B_SPLINE_CURVE_WITH_KNOTS('',2,(#67858,#67859,#67860),
 .UNSPECIFIED.,.F.,.F.,(3,3),(0.,1.),.UNSPECIFIED.);
#1553=B_SPLINE_CURVE_WITH_KNOTS('',2,(#67868,#67869,#67870),
 .UNSPECIFIED.,.F.,.F.,(3,3),(0.,1.),.UNSPECIFIED.);
#1554=B_SPLINE_CURVE_WITH_KNOTS('',2,(#67873,#67874,#67875),
 .UNSPECIFIED.,.F.,.F.,(3,3),(0.,1.),.UNSPECIFIED.);
#1555=B_SPLINE_CURVE_WITH_KNOTS('',2,(#67882,#67883,#67884),
 .UNSPECIFIED.,.F.,.F.,(3,3),(0.,1.),.UNSPECIFIED.);
#1556=B_SPLINE_CURVE_WITH_KNOTS('',2,(#67885,#67886,#67887),
 .UNSPECIFIED.,.F.,.F.,(3,3),(0.,1.),.UNSPECIFIED.);
#1557=B_SPLINE_CURVE_WITH_KNOTS('',2,(#67896,#67897,#67898),
 .UNSPECIFIED.,.F.,.F.,(3,3),(0.,1.),.UNSPECIFIED.);
#1558=B_SPLINE_CURVE_WITH_KNOTS('',2,(#67902,#67903,#67904),
 .UNSPECIFIED.,.F.,.F.,(3,3),(0.,1.),.UNSPECIFIED.);
#1559=B_SPLINE_CURVE_WITH_KNOTS('',2,(#67913,#67914,#67915),
 .UNSPECIFIED.,.F.,.F.,(3,3),(0.,1.),.UNSPECIFIED.);
#1560=B_SPLINE_CURVE_WITH_KNOTS('',2,(#67918,#67919,#67920),
 .UNSPECIFIED.,.F.,.F.,(3,3),(0.,1.),.UNSPECIFIED.);
#1561=B_SPLINE_CURVE_WITH_KNOTS('',2,(#67928,#67929,#67930),
 .UNSPECIFIED.,.F.,.F.,(3,3),(0.,1.),.UNSPECIFIED.);
#1562=B_SPLINE_CURVE_WITH_KNOTS('',2,(#67933,#67934,#67935),
 .UNSPECIFIED.,.F.,.F.,(3,3),(0.,1.),.UNSPECIFIED.);
#1563=B_SPLINE_CURVE_WITH_KNOTS('',2,(#67943,#67944,#67945),
 .UNSPECIFIED.,.F.,.F.,(3,3),(0.,1.),.UNSPECIFIED.);
#1564=B_SPLINE_CURVE_WITH_KNOTS('',2,(#67948,#67949,#67950),
 .UNSPECIFIED.,.F.,.F.,(3,3),(0.,1.),.UNSPECIFIED.);
#1565=B_SPLINE_CURVE_WITH_KNOTS('',2,(#67958,#67959,#67960),
 .UNSPECIFIED.,.F.,.F.,(3,3),(0.,1.),.UNSPECIFIED.);
#1566=B_SPLINE_CURVE_WITH_KNOTS('',2,(#67963,#67964,#67965),
 .UNSPECIFIED.,.F.,.F.,(3,3),(0.,1.),.UNSPECIFIED.);
#1567=B_SPLINE_CURVE_WITH_KNOTS('',2,(#67973,#67974,#67975),
 .UNSPECIFIED.,.F.,.F.,(3,3),(0.,1.),.UNSPECIFIED.);
#1568=B_SPLINE_CURVE_WITH_KNOTS('',2,(#67978,#67979,#67980),
 .UNSPECIFIED.,.F.,.F.,(3,3),(0.,1.),.UNSPECIFIED.);
#1569=B_SPLINE_CURVE_WITH_KNOTS('',2,(#67988,#67989,#67990),
 .UNSPECIFIED.,.F.,.F.,(3,3),(0.,1.),.UNSPECIFIED.);
#1570=B_SPLINE_CURVE_WITH_KNOTS('',2,(#67993,#67994,#67995),
 .UNSPECIFIED.,.F.,.F.,(3,3),(0.,1.),.UNSPECIFIED.);
#1571=B_SPLINE_CURVE_WITH_KNOTS('',2,(#68003,#68004,#68005),
 .UNSPECIFIED.,.F.,.F.,(3,3),(0.,1.),.UNSPECIFIED.);
#1572=B_SPLINE_CURVE_WITH_KNOTS('',2,(#68008,#68009,#68010),
 .UNSPECIFIED.,.F.,.F.,(3,3),(0.,1.),.UNSPECIFIED.);
#1573=B_SPLINE_CURVE_WITH_KNOTS('',2,(#68017,#68018,#68019),
 .UNSPECIFIED.,.F.,.F.,(3,3),(0.,1.),.UNSPECIFIED.);
#1574=B_SPLINE_CURVE_WITH_KNOTS('',2,(#68020,#68021,#68022),
 .UNSPECIFIED.,.F.,.F.,(3,3),(0.,1.),.UNSPECIFIED.);
#1575=B_SPLINE_CURVE_WITH_KNOTS('',2,(#68031,#68032,#68033),
 .UNSPECIFIED.,.F.,.F.,(3,3),(0.,1.),.UNSPECIFIED.);
#1576=B_SPLINE_CURVE_WITH_KNOTS('',2,(#68037,#68038,#68039),
 .UNSPECIFIED.,.F.,.F.,(3,3),(0.,1.),.UNSPECIFIED.);
#1577=B_SPLINE_CURVE_WITH_KNOTS('',2,(#68048,#68049,#68050),
 .UNSPECIFIED.,.F.,.F.,(3,3),(0.,1.),.UNSPECIFIED.);
#1578=B_SPLINE_CURVE_WITH_KNOTS('',2,(#68053,#68054,#68055),
 .UNSPECIFIED.,.F.,.F.,(3,3),(0.,1.),.UNSPECIFIED.);
#1579=B_SPLINE_CURVE_WITH_KNOTS('',2,(#68063,#68064,#68065),
 .UNSPECIFIED.,.F.,.F.,(3,3),(0.,1.),.UNSPECIFIED.);
#1580=B_SPLINE_CURVE_WITH_KNOTS('',2,(#68068,#68069,#68070),
 .UNSPECIFIED.,.F.,.F.,(3,3),(0.,1.),.UNSPECIFIED.);
#1581=B_SPLINE_CURVE_WITH_KNOTS('',2,(#68078,#68079,#68080),
 .UNSPECIFIED.,.F.,.F.,(3,3),(0.,1.),.UNSPECIFIED.);
#1582=B_SPLINE_CURVE_WITH_KNOTS('',2,(#68083,#68084,#68085),
 .UNSPECIFIED.,.F.,.F.,(3,3),(0.,1.),.UNSPECIFIED.);
#1583=B_SPLINE_CURVE_WITH_KNOTS('',2,(#68093,#68094,#68095),
 .UNSPECIFIED.,.F.,.F.,(3,3),(0.,1.),.UNSPECIFIED.);
#1584=B_SPLINE_CURVE_WITH_KNOTS('',2,(#68098,#68099,#68100),
 .UNSPECIFIED.,.F.,.F.,(3,3),(0.,1.),.UNSPECIFIED.);
#1585=B_SPLINE_CURVE_WITH_KNOTS('',2,(#68108,#68109,#68110),
 .UNSPECIFIED.,.F.,.F.,(3,3),(0.,1.),.UNSPECIFIED.);
#1586=B_SPLINE_CURVE_WITH_KNOTS('',2,(#68113,#68114,#68115),
 .UNSPECIFIED.,.F.,.F.,(3,3),(0.,1.),.UNSPECIFIED.);
#1587=B_SPLINE_CURVE_WITH_KNOTS('',2,(#68123,#68124,#68125),
 .UNSPECIFIED.,.F.,.F.,(3,3),(0.,1.),.UNSPECIFIED.);
#1588=B_SPLINE_CURVE_WITH_KNOTS('',2,(#68128,#68129,#68130),
 .UNSPECIFIED.,.F.,.F.,(3,3),(0.,1.),.UNSPECIFIED.);
#1589=B_SPLINE_CURVE_WITH_KNOTS('',2,(#68138,#68139,#68140),
 .UNSPECIFIED.,.F.,.F.,(3,3),(0.,1.),.UNSPECIFIED.);
#1590=B_SPLINE_CURVE_WITH_KNOTS('',2,(#68143,#68144,#68145),
 .UNSPECIFIED.,.F.,.F.,(3,3),(0.,1.),.UNSPECIFIED.);
#1591=B_SPLINE_CURVE_WITH_KNOTS('',2,(#68153,#68154,#68155),
 .UNSPECIFIED.,.F.,.F.,(3,3),(0.,1.),.UNSPECIFIED.);
#1592=B_SPLINE_CURVE_WITH_KNOTS('',2,(#68158,#68159,#68160),
 .UNSPECIFIED.,.F.,.F.,(3,3),(0.,1.),.UNSPECIFIED.);
#1593=B_SPLINE_CURVE_WITH_KNOTS('',2,(#68168,#68169,#68170),
 .UNSPECIFIED.,.F.,.F.,(3,3),(0.,1.),.UNSPECIFIED.);
#1594=B_SPLINE_CURVE_WITH_KNOTS('',2,(#68173,#68174,#68175),
 .UNSPECIFIED.,.F.,.F.,(3,3),(0.,1.),.UNSPECIFIED.);
#1595=B_SPLINE_CURVE_WITH_KNOTS('',2,(#68183,#68184,#68185),
 .UNSPECIFIED.,.F.,.F.,(3,3),(0.,1.),.UNSPECIFIED.);
#1596=B_SPLINE_CURVE_WITH_KNOTS('',2,(#68188,#68189,#68190),
 .UNSPECIFIED.,.F.,.F.,(3,3),(0.,1.),.UNSPECIFIED.);
#1597=B_SPLINE_CURVE_WITH_KNOTS('',2,(#68198,#68199,#68200),
 .UNSPECIFIED.,.F.,.F.,(3,3),(0.,1.),.UNSPECIFIED.);
#1598=B_SPLINE_CURVE_WITH_KNOTS('',2,(#68203,#68204,#68205),
 .UNSPECIFIED.,.F.,.F.,(3,3),(0.,1.),.UNSPECIFIED.);
#1599=B_SPLINE_CURVE_WITH_KNOTS('',2,(#68213,#68214,#68215),
 .UNSPECIFIED.,.F.,.F.,(3,3),(0.,1.),.UNSPECIFIED.);
#1600=B_SPLINE_CURVE_WITH_KNOTS('',2,(#68218,#68219,#68220),
 .UNSPECIFIED.,.F.,.F.,(3,3),(0.,1.),.UNSPECIFIED.);
#1601=B_SPLINE_CURVE_WITH_KNOTS('',2,(#68228,#68229,#68230),
 .UNSPECIFIED.,.F.,.F.,(3,3),(0.,1.),.UNSPECIFIED.);
#1602=B_SPLINE_CURVE_WITH_KNOTS('',2,(#68233,#68234,#68235),
 .UNSPECIFIED.,.F.,.F.,(3,3),(0.,1.),.UNSPECIFIED.);
#1603=B_SPLINE_CURVE_WITH_KNOTS('',2,(#68243,#68244,#68245),
 .UNSPECIFIED.,.F.,.F.,(3,3),(0.,1.),.UNSPECIFIED.);
#1604=B_SPLINE_CURVE_WITH_KNOTS('',2,(#68248,#68249,#68250),
 .UNSPECIFIED.,.F.,.F.,(3,3),(0.,1.),.UNSPECIFIED.);
#1605=B_SPLINE_CURVE_WITH_KNOTS('',2,(#68257,#68258,#68259),
 .UNSPECIFIED.,.F.,.F.,(3,3),(0.,1.),.UNSPECIFIED.);
#1606=B_SPLINE_CURVE_WITH_KNOTS('',2,(#68260,#68261,#68262),
 .UNSPECIFIED.,.F.,.F.,(3,3),(0.,1.),.UNSPECIFIED.);
#1607=B_SPLINE_CURVE_WITH_KNOTS('',2,(#68297,#68298,#68299),
 .UNSPECIFIED.,.F.,.F.,(3,3),(0.,1.),.UNSPECIFIED.);
#1608=B_SPLINE_CURVE_WITH_KNOTS('',2,(#68303,#68304,#68305),
 .UNSPECIFIED.,.F.,.F.,(3,3),(0.,1.),.UNSPECIFIED.);
#1609=B_SPLINE_CURVE_WITH_KNOTS('',2,(#68314,#68315,#68316),
 .UNSPECIFIED.,.F.,.F.,(3,3),(0.,1.),.UNSPECIFIED.);
#1610=B_SPLINE_CURVE_WITH_KNOTS('',2,(#68319,#68320,#68321),
 .UNSPECIFIED.,.F.,.F.,(3,3),(0.,1.),.UNSPECIFIED.);
#1611=B_SPLINE_CURVE_WITH_KNOTS('',2,(#68329,#68330,#68331),
 .UNSPECIFIED.,.F.,.F.,(3,3),(0.,1.),.UNSPECIFIED.);
#1612=B_SPLINE_CURVE_WITH_KNOTS('',2,(#68334,#68335,#68336),
 .UNSPECIFIED.,.F.,.F.,(3,3),(0.,1.),.UNSPECIFIED.);
#1613=B_SPLINE_CURVE_WITH_KNOTS('',2,(#68344,#68345,#68346),
 .UNSPECIFIED.,.F.,.F.,(3,3),(0.,1.),.UNSPECIFIED.);
#1614=B_SPLINE_CURVE_WITH_KNOTS('',2,(#68349,#68350,#68351),
 .UNSPECIFIED.,.F.,.F.,(3,3),(0.,1.),.UNSPECIFIED.);
#1615=B_SPLINE_CURVE_WITH_KNOTS('',2,(#68359,#68360,#68361),
 .UNSPECIFIED.,.F.,.F.,(3,3),(0.,1.),.UNSPECIFIED.);
#1616=B_SPLINE_CURVE_WITH_KNOTS('',2,(#68364,#68365,#68366),
 .UNSPECIFIED.,.F.,.F.,(3,3),(0.,1.),.UNSPECIFIED.);
#1617=B_SPLINE_CURVE_WITH_KNOTS('',2,(#68374,#68375,#68376),
 .UNSPECIFIED.,.F.,.F.,(3,3),(0.,1.),.UNSPECIFIED.);
#1618=B_SPLINE_CURVE_WITH_KNOTS('',2,(#68379,#68380,#68381),
 .UNSPECIFIED.,.F.,.F.,(3,3),(0.,1.),.UNSPECIFIED.);
#1619=B_SPLINE_CURVE_WITH_KNOTS('',2,(#68389,#68390,#68391),
 .UNSPECIFIED.,.F.,.F.,(3,3),(0.,1.),.UNSPECIFIED.);
#1620=B_SPLINE_CURVE_WITH_KNOTS('',2,(#68394,#68395,#68396),
 .UNSPECIFIED.,.F.,.F.,(3,3),(0.,1.),.UNSPECIFIED.);
#1621=B_SPLINE_CURVE_WITH_KNOTS('',2,(#68403,#68404,#68405),
 .UNSPECIFIED.,.F.,.F.,(3,3),(0.,1.),.UNSPECIFIED.);
#1622=B_SPLINE_CURVE_WITH_KNOTS('',2,(#68406,#68407,#68408),
 .UNSPECIFIED.,.F.,.F.,(3,3),(0.,1.),.UNSPECIFIED.);
#1623=B_SPLINE_CURVE_WITH_KNOTS('',2,(#68417,#68418,#68419),
 .UNSPECIFIED.,.F.,.F.,(3,3),(0.,1.),.UNSPECIFIED.);
#1624=B_SPLINE_CURVE_WITH_KNOTS('',2,(#68423,#68424,#68425),
 .UNSPECIFIED.,.F.,.F.,(3,3),(0.,1.),.UNSPECIFIED.);
#1625=B_SPLINE_CURVE_WITH_KNOTS('',2,(#68434,#68435,#68436),
 .UNSPECIFIED.,.F.,.F.,(3,3),(0.,1.),.UNSPECIFIED.);
#1626=B_SPLINE_CURVE_WITH_KNOTS('',2,(#68439,#68440,#68441),
 .UNSPECIFIED.,.F.,.F.,(3,3),(0.,1.),.UNSPECIFIED.);
#1627=B_SPLINE_CURVE_WITH_KNOTS('',2,(#68449,#68450,#68451),
 .UNSPECIFIED.,.F.,.F.,(3,3),(0.,1.),.UNSPECIFIED.);
#1628=B_SPLINE_CURVE_WITH_KNOTS('',2,(#68454,#68455,#68456),
 .UNSPECIFIED.,.F.,.F.,(3,3),(0.,1.),.UNSPECIFIED.);
#1629=B_SPLINE_CURVE_WITH_KNOTS('',2,(#68464,#68465,#68466),
 .UNSPECIFIED.,.F.,.F.,(3,3),(0.,1.),.UNSPECIFIED.);
#1630=B_SPLINE_CURVE_WITH_KNOTS('',2,(#68469,#68470,#68471),
 .UNSPECIFIED.,.F.,.F.,(3,3),(0.,1.),.UNSPECIFIED.);
#1631=B_SPLINE_CURVE_WITH_KNOTS('',2,(#68479,#68480,#68481),
 .UNSPECIFIED.,.F.,.F.,(3,3),(0.,1.),.UNSPECIFIED.);
#1632=B_SPLINE_CURVE_WITH_KNOTS('',2,(#68484,#68485,#68486),
 .UNSPECIFIED.,.F.,.F.,(3,3),(0.,1.),.UNSPECIFIED.);
#1633=B_SPLINE_CURVE_WITH_KNOTS('',2,(#68494,#68495,#68496),
 .UNSPECIFIED.,.F.,.F.,(3,3),(0.,1.),.UNSPECIFIED.);
#1634=B_SPLINE_CURVE_WITH_KNOTS('',2,(#68499,#68500,#68501),
 .UNSPECIFIED.,.F.,.F.,(3,3),(0.,1.),.UNSPECIFIED.);
#1635=B_SPLINE_CURVE_WITH_KNOTS('',2,(#68509,#68510,#68511),
 .UNSPECIFIED.,.F.,.F.,(3,3),(0.,1.),.UNSPECIFIED.);
#1636=B_SPLINE_CURVE_WITH_KNOTS('',2,(#68514,#68515,#68516),
 .UNSPECIFIED.,.F.,.F.,(3,3),(0.,1.),.UNSPECIFIED.);
#1637=B_SPLINE_CURVE_WITH_KNOTS('',2,(#68524,#68525,#68526),
 .UNSPECIFIED.,.F.,.F.,(3,3),(0.,1.),.UNSPECIFIED.);
#1638=B_SPLINE_CURVE_WITH_KNOTS('',2,(#68529,#68530,#68531),
 .UNSPECIFIED.,.F.,.F.,(3,3),(0.,1.),.UNSPECIFIED.);
#1639=B_SPLINE_CURVE_WITH_KNOTS('',2,(#68538,#68539,#68540),
 .UNSPECIFIED.,.F.,.F.,(3,3),(0.,1.),.UNSPECIFIED.);
#1640=B_SPLINE_CURVE_WITH_KNOTS('',2,(#68541,#68542,#68543),
 .UNSPECIFIED.,.F.,.F.,(3,3),(0.,1.),.UNSPECIFIED.);
#1641=B_SPLINE_CURVE_WITH_KNOTS('',2,(#68552,#68553,#68554),
 .UNSPECIFIED.,.F.,.F.,(3,3),(0.,1.),.UNSPECIFIED.);
#1642=B_SPLINE_CURVE_WITH_KNOTS('',2,(#68558,#68559,#68560),
 .UNSPECIFIED.,.F.,.F.,(3,3),(0.,1.),.UNSPECIFIED.);
#1643=B_SPLINE_CURVE_WITH_KNOTS('',2,(#68569,#68570,#68571),
 .UNSPECIFIED.,.F.,.F.,(3,3),(0.,1.),.UNSPECIFIED.);
#1644=B_SPLINE_CURVE_WITH_KNOTS('',2,(#68574,#68575,#68576),
 .UNSPECIFIED.,.F.,.F.,(3,3),(0.,1.),.UNSPECIFIED.);
#1645=B_SPLINE_CURVE_WITH_KNOTS('',2,(#68584,#68585,#68586),
 .UNSPECIFIED.,.F.,.F.,(3,3),(0.,1.),.UNSPECIFIED.);
#1646=B_SPLINE_CURVE_WITH_KNOTS('',2,(#68589,#68590,#68591),
 .UNSPECIFIED.,.F.,.F.,(3,3),(0.,1.),.UNSPECIFIED.);
#1647=B_SPLINE_CURVE_WITH_KNOTS('',2,(#68599,#68600,#68601),
 .UNSPECIFIED.,.F.,.F.,(3,3),(0.,1.),.UNSPECIFIED.);
#1648=B_SPLINE_CURVE_WITH_KNOTS('',2,(#68604,#68605,#68606),
 .UNSPECIFIED.,.F.,.F.,(3,3),(0.,1.),.UNSPECIFIED.);
#1649=B_SPLINE_CURVE_WITH_KNOTS('',2,(#68614,#68615,#68616),
 .UNSPECIFIED.,.F.,.F.,(3,3),(0.,1.),.UNSPECIFIED.);
#1650=B_SPLINE_CURVE_WITH_KNOTS('',2,(#68619,#68620,#68621),
 .UNSPECIFIED.,.F.,.F.,(3,3),(0.,1.),.UNSPECIFIED.);
#1651=B_SPLINE_CURVE_WITH_KNOTS('',2,(#68629,#68630,#68631),
 .UNSPECIFIED.,.F.,.F.,(3,3),(0.,1.),.UNSPECIFIED.);
#1652=B_SPLINE_CURVE_WITH_KNOTS('',2,(#68634,#68635,#68636),
 .UNSPECIFIED.,.F.,.F.,(3,3),(0.,1.),.UNSPECIFIED.);
#1653=B_SPLINE_CURVE_WITH_KNOTS('',2,(#68644,#68645,#68646),
 .UNSPECIFIED.,.F.,.F.,(3,3),(0.,1.),.UNSPECIFIED.);
#1654=B_SPLINE_CURVE_WITH_KNOTS('',2,(#68649,#68650,#68651),
 .UNSPECIFIED.,.F.,.F.,(3,3),(0.,1.),.UNSPECIFIED.);
#1655=B_SPLINE_CURVE_WITH_KNOTS('',2,(#68659,#68660,#68661),
 .UNSPECIFIED.,.F.,.F.,(3,3),(0.,1.),.UNSPECIFIED.);
#1656=B_SPLINE_CURVE_WITH_KNOTS('',2,(#68664,#68665,#68666),
 .UNSPECIFIED.,.F.,.F.,(3,3),(0.,1.),.UNSPECIFIED.);
#1657=B_SPLINE_CURVE_WITH_KNOTS('',2,(#68674,#68675,#68676),
 .UNSPECIFIED.,.F.,.F.,(3,3),(0.,1.),.UNSPECIFIED.);
#1658=B_SPLINE_CURVE_WITH_KNOTS('',2,(#68679,#68680,#68681),
 .UNSPECIFIED.,.F.,.F.,(3,3),(0.,1.),.UNSPECIFIED.);
#1659=B_SPLINE_CURVE_WITH_KNOTS('',2,(#68689,#68690,#68691),
 .UNSPECIFIED.,.F.,.F.,(3,3),(0.,1.),.UNSPECIFIED.);
#1660=B_SPLINE_CURVE_WITH_KNOTS('',2,(#68694,#68695,#68696),
 .UNSPECIFIED.,.F.,.F.,(3,3),(0.,1.),.UNSPECIFIED.);
#1661=B_SPLINE_CURVE_WITH_KNOTS('',2,(#68704,#68705,#68706),
 .UNSPECIFIED.,.F.,.F.,(3,3),(0.,1.),.UNSPECIFIED.);
#1662=B_SPLINE_CURVE_WITH_KNOTS('',2,(#68709,#68710,#68711),
 .UNSPECIFIED.,.F.,.F.,(3,3),(0.,1.),.UNSPECIFIED.);
#1663=B_SPLINE_CURVE_WITH_KNOTS('',2,(#68719,#68720,#68721),
 .UNSPECIFIED.,.F.,.F.,(3,3),(0.,1.),.UNSPECIFIED.);
#1664=B_SPLINE_CURVE_WITH_KNOTS('',2,(#68724,#68725,#68726),
 .UNSPECIFIED.,.F.,.F.,(3,3),(0.,1.),.UNSPECIFIED.);
#1665=B_SPLINE_CURVE_WITH_KNOTS('',2,(#68734,#68735,#68736),
 .UNSPECIFIED.,.F.,.F.,(3,3),(0.,1.),.UNSPECIFIED.);
#1666=B_SPLINE_CURVE_WITH_KNOTS('',2,(#68739,#68740,#68741),
 .UNSPECIFIED.,.F.,.F.,(3,3),(0.,1.),.UNSPECIFIED.);
#1667=B_SPLINE_CURVE_WITH_KNOTS('',2,(#68749,#68750,#68751),
 .UNSPECIFIED.,.F.,.F.,(3,3),(0.,1.),.UNSPECIFIED.);
#1668=B_SPLINE_CURVE_WITH_KNOTS('',2,(#68754,#68755,#68756),
 .UNSPECIFIED.,.F.,.F.,(3,3),(0.,1.),.UNSPECIFIED.);
#1669=B_SPLINE_CURVE_WITH_KNOTS('',2,(#68764,#68765,#68766),
 .UNSPECIFIED.,.F.,.F.,(3,3),(0.,1.),.UNSPECIFIED.);
#1670=B_SPLINE_CURVE_WITH_KNOTS('',2,(#68769,#68770,#68771),
 .UNSPECIFIED.,.F.,.F.,(3,3),(0.,1.),.UNSPECIFIED.);
#1671=B_SPLINE_CURVE_WITH_KNOTS('',2,(#68778,#68779,#68780),
 .UNSPECIFIED.,.F.,.F.,(3,3),(0.,1.),.UNSPECIFIED.);
#1672=B_SPLINE_CURVE_WITH_KNOTS('',2,(#68781,#68782,#68783),
 .UNSPECIFIED.,.F.,.F.,(3,3),(0.,1.),.UNSPECIFIED.);
#1673=B_SPLINE_CURVE_WITH_KNOTS('',3,(#68790,#68791,#68792,#68793,#68794,
#68795,#68796,#68797,#68798,#68799,#68800,#68801,#68802,#68803,#68804,#68805,
#68806,#68807,#68808,#68809,#68810,#68811,#68812,#68813,#68814,#68815,#68816,
#68817,#68818,#68819,#68820,#68821,#68822,#68823,#68824,#68825,#68826,#68827,
#68828,#68829,#68830,#68831,#68832,#68833,#68834,#68835,#68836,#68837,#68838,
#68839,#68840,#68841,#68842,#68843,#68844,#68845,#68846,#68847,#68848,#68849,
#68850,#68851,#68852,#68853,#68854,#68855,#68856,#68857,#68858,#68859,#68860,
#68861,#68862),.UNSPECIFIED.,.F.,.F.,(4,3,3,3,3,3,3,3,3,3,3,3,3,3,3,3,3,
3,3,3,3,3,3,3,4),(-1.5337369924875,-1.47614434194274,-1.38903457285003,
-1.35939767545676,-1.33406695848438,-1.23088611202814,-1.19147645830862,
-1.16614958179783,-1.1277052655719,-1.02513486077225,-0.955412872192556,
-0.901872933084063,-0.873045820076336,-0.765171934991001,-0.671173342986202,
-0.616456444662515,-0.58488614612667,-0.476926645981598,-0.389177566971804,
-0.338395442046788,-0.310738024076525,-0.288566068862146,-0.179389393286242,
-0.0693222977829609,0.),.UNSPECIFIED.);
#1674=B_SPLINE_CURVE_WITH_KNOTS('',3,(#68867,#68868,#68869,#68870,#68871,
#68872,#68873,#68874,#68875,#68876,#68877,#68878,#68879,#68880,#68881,#68882,
#68883,#68884,#68885,#68886,#68887,#68888,#68889,#68890,#68891,#68892,#68893,
#68894,#68895,#68896,#68897,#68898,#68899,#68900,#68901,#68902,#68903,#68904,
#68905,#68906,#68907,#68908,#68909,#68910,#68911,#68912,#68913,#68914,#68915,
#68916,#68917,#68918,#68919,#68920,#68921,#68922,#68923,#68924,#68925,#68926,
#68927,#68928,#68929,#68930,#68931,#68932,#68933,#68934,#68935,#68936,#68937,
#68938,#68939,#68940,#68941,#68942,#68943,#68944,#68945),.UNSPECIFIED.,
 .F.,.F.,(4,3,3,3,3,3,3,3,3,3,3,3,3,3,3,3,3,3,3,3,3,3,3,3,3,3,4),(-1.52870610664513,
-1.46224068530639,-1.36596309804718,-1.32440296404387,-1.2951147317008,
-1.18612253398519,-1.14615032738057,-1.1200232336817,-1.0958154346986,-1.07713033626957,
-0.970210386711197,-0.864245604343508,-0.830831276447041,-0.810033160995986,
-0.704712885007061,-0.614931313624051,-0.566215947085015,-0.5441889725864,
-0.52276593090361,-0.420925957142934,-0.345586599475019,-0.297497915232979,
-0.271800404456334,-0.25273374406439,-0.152661671243804,-0.0544537748451435,
0.),.UNSPECIFIED.);
#1675=B_SPLINE_CURVE_WITH_KNOTS('',3,(#69694,#69695,#69696,#69697),
 .UNSPECIFIED.,.F.,.F.,(4,4),(89.0882430066573,89.5008331081196),
 .UNSPECIFIED.);
#1676=B_SPLINE_CURVE_WITH_KNOTS('',3,(#69699,#69700,#69701,#69702,#69703,
#69704,#69705,#69706,#69707,#69708,#69709,#69710,#69711,#69712,#69713,#69714,
#69715,#69716,#69717,#69718,#69719,#69720,#69721,#69722,#69723,#69724,#69725,
#69726,#69727,#69728,#69729,#69730,#69731,#69732,#69733,#69734,#69735,#69736,
#69737,#69738,#69739,#69740,#69741,#69742,#69743,#69744,#69745,#69746,#69747,
#69748,#69749,#69750,#69751,#69752,#69753,#69754,#69755,#69756,#69757,#69758,
#69759,#69760,#69761,#69762,#69763,#69764,#69765,#69766,#69767,#69768,#69769,
#69770,#69771),.UNSPECIFIED.,.F.,.F.,(4,3,3,3,3,3,3,3,3,3,3,3,3,3,3,3,3,
3,3,3,3,3,3,3,4),(-1.53373699248748,-1.47614434194271,-1.38903457285,-1.35939768361858,
-1.33406696685154,-1.23088611621171,-1.19147646127634,-1.16614958291887,
-1.12770526557188,-1.02513485497022,-0.955412885820892,-0.901872950742785,
-0.87304581950843,-0.765171934991016,-0.671173342986216,-0.616456453073865,
-0.584886146683686,-0.476926640886848,-0.389177566971813,-0.338395437911183,
-0.310738015345227,-0.288566061371844,-0.179389433105355,-0.0693223098585095,
0.),.UNSPECIFIED.);
#1677=B_SPLINE_CURVE_WITH_KNOTS('',3,(#69772,#69773,#69774,#69775,#69776,
#69777,#69778,#69779,#69780,#69781,#69782,#69783,#69784,#69785),
 .UNSPECIFIED.,.F.,.F.,(4,1,1,1,1,1,1,1,1,1,1,4),(10.3761157273101,10.7896026128002,
11.287297284435,11.7849919560698,12.2826866277046,12.7803812993394,13.2780759709742,
13.775770642609,14.2734653142438,14.7711599858786,15.2688546575134,15.7079632679489),
 .UNSPECIFIED.);
#1678=B_SPLINE_CURVE_WITH_KNOTS('',3,(#69791,#69792,#69793,#69794,#69795,
#69796,#69797,#69798,#69799,#69800,#69801,#69802,#69803,#69804,#69805,#69806,
#69807,#69808,#69809,#69810,#69811,#69812,#69813,#69814,#69815,#69816,#69817,
#69818,#69819,#69820,#69821,#69822,#69823,#69824,#69825,#69826,#69827,#69828,
#69829,#69830,#69831,#69832,#69833,#69834,#69835,#69836,#69837,#69838,#69839,
#69840,#69841,#69842,#69843,#69844,#69845,#69846,#69847,#69848,#69849,#69850,
#69851,#69852,#69853,#69854,#69855,#69856,#69857,#69858,#69859,#69860,#69861,
#69862,#69863,#69864,#69865,#69866,#69867,#69868,#69869),.UNSPECIFIED.,
 .F.,.F.,(4,3,3,3,3,3,3,3,3,3,3,3,3,3,3,3,3,3,3,3,3,3,3,3,3,3,4),(-1.52870610664512,
-1.46224068530633,-1.36596309804712,-1.32440295915268,-1.29511472974395,
-1.18612253300673,-1.1461503275642,-1.12002323492101,-1.09581543513247,
-1.07713033626952,-0.970210390750287,-0.864245635359953,-0.830831234316541,
-0.810033082630868,-0.70471288500701,-0.614931313624002,-0.566215946319255,
-0.544188965889431,-0.522765927890383,-0.4209259135058,-0.345586599474978,
-0.297497900017229,-0.271800352260087,-0.252733663988387,-0.15266159062613,
-0.0544537709407456,0.),.UNSPECIFIED.);
#1679=B_SPLINE_CURVE_WITH_KNOTS('',3,(#69872,#69873,#69874,#69875,#69876,
#69877,#69878,#69879,#69880,#69881,#69882,#69883),.UNSPECIFIED.,.F.,.F.,
(4,1,1,1,1,1,1,1,1,4),(11.6150328478182,12.112727519453,12.6104221910878,
13.1081168627226,13.6058115343574,14.1035062059922,14.601200877627,15.0988955492618,
15.5965902208966,15.7079632679489),.UNSPECIFIED.);
#1680=PLANE('',#27059);
#1681=PLANE('',#27102);
#1682=PLANE('',#27141);
#1683=PLANE('',#27147);
#1684=PLANE('',#27152);
#1685=PLANE('',#27158);
#1686=PLANE('',#27160);
#1687=PLANE('',#27161);
#1688=PLANE('',#27163);
#1689=PLANE('',#27164);
#1690=PLANE('',#27166);
#1691=PLANE('',#27167);
#1692=PLANE('',#27169);
#1693=PLANE('',#27170);
#1694=PLANE('',#27172);
#1695=PLANE('',#27173);
#1696=PLANE('',#27175);
#1697=PLANE('',#27176);
#1698=PLANE('',#27178);
#1699=PLANE('',#27179);
#1700=PLANE('',#27181);
#1701=PLANE('',#27182);
#1702=PLANE('',#27184);
#1703=PLANE('',#27185);
#1704=PLANE('',#27187);
#1705=PLANE('',#27188);
#1706=PLANE('',#27190);
#1707=PLANE('',#27191);
#1708=PLANE('',#27193);
#1709=PLANE('',#27194);
#1710=PLANE('',#27196);
#1711=PLANE('',#27197);
#1712=PLANE('',#27199);
#1713=PLANE('',#27200);
#1714=PLANE('',#27202);
#1715=PLANE('',#27203);
#1716=PLANE('',#27205);
#1717=PLANE('',#27206);
#1718=PLANE('',#27208);
#1719=PLANE('',#27209);
#1720=PLANE('',#27211);
#1721=PLANE('',#27212);
#1722=PLANE('',#27261);
#1723=PLANE('',#27264);
#1724=PLANE('',#27271);
#1725=PLANE('',#27277);
#1726=PLANE('',#27282);
#1727=PLANE('',#27284);
#1728=PLANE('',#27290);
#1729=PLANE('',#27291);
#1730=PLANE('',#27292);
#1731=PLANE('',#27293);
#1732=PLANE('',#27294);
#1733=PLANE('',#27298);
#1734=PLANE('',#27299);
#1735=PLANE('',#27309);
#1736=PLANE('',#27310);
#1737=PLANE('',#27311);
#1738=PLANE('',#27312);
#1739=PLANE('',#27313);
#1740=PLANE('',#27314);
#1741=PLANE('',#27321);
#1742=PLANE('',#27326);
#1743=PLANE('',#27327);
#1744=PLANE('',#27328);
#1745=PLANE('',#27329);
#1746=PLANE('',#27330);
#1747=PLANE('',#27335);
#1748=PLANE('',#27340);
#1749=PLANE('',#27341);
#1750=PLANE('',#27342);
#1751=PLANE('',#27343);
#1752=PLANE('',#27344);
#1753=PLANE('',#27345);
#1754=PLANE('',#27348);
#1755=PLANE('',#27353);
#1756=PLANE('',#27367);
#1757=PLANE('',#27370);
#1758=PLANE('',#27376);
#1759=PLANE('',#27379);
#1760=PLANE('',#27383);
#1761=PLANE('',#27390);
#1762=PLANE('',#27398);
#1763=PLANE('',#27424);
#1764=PLANE('',#27429);
#1765=PLANE('',#27450);
#1766=PLANE('',#27453);
#1767=PLANE('',#27458);
#1768=PLANE('',#27460);
#1769=PLANE('',#27462);
#1770=PLANE('',#27464);
#1771=PLANE('',#27466);
#1772=PLANE('',#27468);
#1773=PLANE('',#27478);
#1774=PLANE('',#27479);
#1775=PLANE('',#27480);
#1776=PLANE('',#27481);
#1777=PLANE('',#27482);
#1778=PLANE('',#27483);
#1779=PLANE('',#27484);
#1780=PLANE('',#27485);
#1781=PLANE('',#27486);
#1782=PLANE('',#27487);
#1783=PLANE('',#27488);
#1784=PLANE('',#27489);
#1785=PLANE('',#27490);
#1786=PLANE('',#27491);
#1787=PLANE('',#27492);
#1788=PLANE('',#27493);
#1789=PLANE('',#27494);
#1790=PLANE('',#27495);
#1791=PLANE('',#27496);
#1792=PLANE('',#27497);
#1793=PLANE('',#27498);
#1794=PLANE('',#27499);
#1795=PLANE('',#27500);
#1796=PLANE('',#27501);
#1797=PLANE('',#27502);
#1798=PLANE('',#27509);
#1799=PLANE('',#27511);
#1800=PLANE('',#27512);
#1801=PLANE('',#27513);
#1802=PLANE('',#27514);
#1803=PLANE('',#27515);
#1804=PLANE('',#27516);
#1805=PLANE('',#27517);
#1806=PLANE('',#27518);
#1807=PLANE('',#27519);
#1808=PLANE('',#27520);
#1809=PLANE('',#27521);
#1810=PLANE('',#27522);
#1811=PLANE('',#27523);
#1812=PLANE('',#27524);
#1813=PLANE('',#27525);
#1814=PLANE('',#27526);
#1815=PLANE('',#27527);
#1816=PLANE('',#27528);
#1817=PLANE('',#27529);
#1818=PLANE('',#27530);
#1819=PLANE('',#27531);
#1820=PLANE('',#27532);
#1821=PLANE('',#27533);
#1822=PLANE('',#27534);
#1823=PLANE('',#27535);
#1824=PLANE('',#27536);
#1825=PLANE('',#27537);
#1826=PLANE('',#27538);
#1827=PLANE('',#27539);
#1828=PLANE('',#27540);
#1829=PLANE('',#27541);
#1830=PLANE('',#27542);
#1831=PLANE('',#27543);
#1832=PLANE('',#27544);
#1833=PLANE('',#27545);
#1834=PLANE('',#27546);
#1835=PLANE('',#27609);
#1836=PLANE('',#27612);
#1837=PLANE('',#27617);
#1838=PLANE('',#27619);
#1839=PLANE('',#27621);
#1840=PLANE('',#27623);
#1841=PLANE('',#27625);
#1842=PLANE('',#27627);
#1843=PLANE('',#27637);
#1844=PLANE('',#27638);
#1845=PLANE('',#27639);
#1846=PLANE('',#27640);
#1847=PLANE('',#27641);
#1848=PLANE('',#27642);
#1849=PLANE('',#27643);
#1850=PLANE('',#27644);
#1851=PLANE('',#27645);
#1852=PLANE('',#27646);
#1853=PLANE('',#27647);
#1854=PLANE('',#27648);
#1855=PLANE('',#27649);
#1856=PLANE('',#27650);
#1857=PLANE('',#27651);
#1858=PLANE('',#27652);
#1859=PLANE('',#27653);
#1860=PLANE('',#27654);
#1861=PLANE('',#27655);
#1862=PLANE('',#27656);
#1863=PLANE('',#27657);
#1864=PLANE('',#27658);
#1865=PLANE('',#27659);
#1866=PLANE('',#27660);
#1867=PLANE('',#27661);
#1868=PLANE('',#27668);
#1869=PLANE('',#27675);
#1870=PLANE('',#27679);
#1871=PLANE('',#27682);
#1872=PLANE('',#27683);
#1873=PLANE('',#27684);
#1874=PLANE('',#27686);
#1875=PLANE('',#27687);
#1876=PLANE('',#27688);
#1877=PLANE('',#27731);
#1878=PLANE('',#27734);
#1879=PLANE('',#27739);
#1880=PLANE('',#27741);
#1881=PLANE('',#27743);
#1882=PLANE('',#27745);
#1883=PLANE('',#27747);
#1884=PLANE('',#27749);
#1885=PLANE('',#27759);
#1886=PLANE('',#27760);
#1887=PLANE('',#27761);
#1888=PLANE('',#27762);
#1889=PLANE('',#27763);
#1890=PLANE('',#27764);
#1891=PLANE('',#27765);
#1892=PLANE('',#27766);
#1893=PLANE('',#27767);
#1894=PLANE('',#27768);
#1895=PLANE('',#27769);
#1896=PLANE('',#27770);
#1897=PLANE('',#27771);
#1898=PLANE('',#27772);
#1899=PLANE('',#27773);
#1900=PLANE('',#27774);
#1901=PLANE('',#27775);
#1902=PLANE('',#27776);
#1903=PLANE('',#27777);
#1904=PLANE('',#27778);
#1905=PLANE('',#27779);
#1906=PLANE('',#27780);
#1907=PLANE('',#27781);
#1908=PLANE('',#27782);
#1909=PLANE('',#27783);
#1910=PLANE('',#27790);
#1911=PLANE('',#27803);
#1912=PLANE('',#27809);
#1913=PLANE('',#27810);
#1914=PLANE('',#27811);
#1915=PLANE('',#27814);
#1916=PLANE('',#27819);
#1917=PLANE('',#27820);
#1918=PLANE('',#27821);
#1919=PLANE('',#27822);
#1920=PLANE('',#27823);
#1921=PLANE('',#27824);
#1922=PLANE('',#27825);
#1923=PLANE('',#27826);
#1924=PLANE('',#27827);
#1925=PLANE('',#27828);
#1926=PLANE('',#27829);
#1927=PLANE('',#27830);
#1928=PLANE('',#27831);
#1929=PLANE('',#27832);
#1930=PLANE('',#27833);
#1931=PLANE('',#27834);
#1932=PLANE('',#27835);
#1933=PLANE('',#27836);
#1934=PLANE('',#27837);
#1935=PLANE('',#27838);
#1936=PLANE('',#27839);
#1937=PLANE('',#27840);
#1938=PLANE('',#27841);
#1939=PLANE('',#27842);
#1940=PLANE('',#27843);
#1941=PLANE('',#27844);
#1942=PLANE('',#27845);
#1943=PLANE('',#27846);
#1944=PLANE('',#27847);
#1945=PLANE('',#27848);
#1946=PLANE('',#27849);
#1947=PLANE('',#27850);
#1948=PLANE('',#27851);
#1949=PLANE('',#27852);
#1950=PLANE('',#27853);
#1951=PLANE('',#27854);
#1952=PLANE('',#27855);
#1953=PLANE('',#27856);
#1954=PLANE('',#27857);
#1955=PLANE('',#27858);
#1956=PLANE('',#27859);
#1957=PLANE('',#27860);
#1958=PLANE('',#27861);
#1959=PLANE('',#27862);
#1960=PLANE('',#27863);
#1961=PLANE('',#27864);
#1962=PLANE('',#27865);
#1963=PLANE('',#27866);
#1964=PLANE('',#27867);
#1965=PLANE('',#27868);
#1966=PLANE('',#27869);
#1967=PLANE('',#27870);
#1968=PLANE('',#27871);
#1969=PLANE('',#27872);
#1970=PLANE('',#27873);
#1971=PLANE('',#27874);
#1972=PLANE('',#27875);
#1973=PLANE('',#27876);
#1974=PLANE('',#27877);
#1975=PLANE('',#27878);
#1976=PLANE('',#27879);
#1977=PLANE('',#27880);
#1978=PLANE('',#27881);
#1979=PLANE('',#27882);
#1980=PLANE('',#27883);
#1981=PLANE('',#27884);
#1982=PLANE('',#27885);
#1983=PLANE('',#27886);
#1984=PLANE('',#27887);
#1985=PLANE('',#27888);
#1986=PLANE('',#27889);
#1987=PLANE('',#27890);
#1988=PLANE('',#27891);
#1989=PLANE('',#27892);
#1990=PLANE('',#27893);
#1991=PLANE('',#27894);
#1992=PLANE('',#27895);
#1993=PLANE('',#27896);
#1994=PLANE('',#27897);
#1995=PLANE('',#27898);
#1996=PLANE('',#27899);
#1997=PLANE('',#27900);
#1998=PLANE('',#27901);
#1999=PLANE('',#27902);
#2000=PLANE('',#27903);
#2001=PLANE('',#27904);
#2002=PLANE('',#27905);
#2003=PLANE('',#27906);
#2004=PLANE('',#27907);
#2005=PLANE('',#27908);
#2006=PLANE('',#27909);
#2007=PLANE('',#27910);
#2008=PLANE('',#27912);
#2009=PLANE('',#27913);
#2010=PLANE('',#27914);
#2011=PLANE('',#27915);
#2012=PLANE('',#27916);
#2013=PLANE('',#27917);
#2014=PLANE('',#27918);
#2015=PLANE('',#27919);
#2016=PLANE('',#27920);
#2017=PLANE('',#27921);
#2018=PLANE('',#27922);
#2019=PLANE('',#27923);
#2020=PLANE('',#27924);
#2021=PLANE('',#27925);
#2022=PLANE('',#27926);
#2023=PLANE('',#27927);
#2024=PLANE('',#27928);
#2025=PLANE('',#27929);
#2026=PLANE('',#27930);
#2027=PLANE('',#27931);
#2028=PLANE('',#27932);
#2029=PLANE('',#27933);
#2030=PLANE('',#27934);
#2031=PLANE('',#27935);
#2032=PLANE('',#27936);
#2033=PLANE('',#27937);
#2034=PLANE('',#27938);
#2035=PLANE('',#27939);
#2036=PLANE('',#27940);
#2037=PLANE('',#27941);
#2038=PLANE('',#27942);
#2039=PLANE('',#27943);
#2040=PLANE('',#27944);
#2041=PLANE('',#27945);
#2042=PLANE('',#27946);
#2043=PLANE('',#27947);
#2044=PLANE('',#27948);
#2045=PLANE('',#27949);
#2046=PLANE('',#27950);
#2047=PLANE('',#27951);
#2048=PLANE('',#27952);
#2049=PLANE('',#27953);
#2050=PLANE('',#27954);
#2051=PLANE('',#27955);
#2052=PLANE('',#27956);
#2053=PLANE('',#27957);
#2054=PLANE('',#27958);
#2055=PLANE('',#27959);
#2056=PLANE('',#27960);
#2057=PLANE('',#27961);
#2058=PLANE('',#27962);
#2059=PLANE('',#27963);
#2060=PLANE('',#27964);
#2061=PLANE('',#27965);
#2062=PLANE('',#27966);
#2063=PLANE('',#27967);
#2064=PLANE('',#27968);
#2065=PLANE('',#27969);
#2066=PLANE('',#27970);
#2067=PLANE('',#27971);
#2068=PLANE('',#27972);
#2069=PLANE('',#27973);
#2070=PLANE('',#27974);
#2071=PLANE('',#27975);
#2072=PLANE('',#27976);
#2073=PLANE('',#27977);
#2074=PLANE('',#27978);
#2075=PLANE('',#27979);
#2076=PLANE('',#27980);
#2077=PLANE('',#27981);
#2078=PLANE('',#27982);
#2079=PLANE('',#27983);
#2080=PLANE('',#27984);
#2081=PLANE('',#27985);
#2082=PLANE('',#27986);
#2083=PLANE('',#27987);
#2084=PLANE('',#27988);
#2085=PLANE('',#27989);
#2086=PLANE('',#27990);
#2087=PLANE('',#27991);
#2088=PLANE('',#27992);
#2089=PLANE('',#27993);
#2090=PLANE('',#27994);
#2091=PLANE('',#27995);
#2092=PLANE('',#27996);
#2093=PLANE('',#27997);
#2094=PLANE('',#27998);
#2095=PLANE('',#27999);
#2096=PLANE('',#28000);
#2097=PLANE('',#28001);
#2098=PLANE('',#28002);
#2099=PLANE('',#28003);
#2100=PLANE('',#28004);
#2101=PLANE('',#28005);
#2102=PLANE('',#28006);
#2103=PLANE('',#28007);
#2104=PLANE('',#28008);
#2105=PLANE('',#28009);
#2106=PLANE('',#28010);
#2107=PLANE('',#28011);
#2108=PLANE('',#28012);
#2109=PLANE('',#28013);
#2110=PLANE('',#28014);
#2111=PLANE('',#28015);
#2112=PLANE('',#28016);
#2113=PLANE('',#28017);
#2114=PLANE('',#28018);
#2115=PLANE('',#28019);
#2116=PLANE('',#28020);
#2117=PLANE('',#28021);
#2118=PLANE('',#28022);
#2119=PLANE('',#28023);
#2120=PLANE('',#28024);
#2121=PLANE('',#28025);
#2122=PLANE('',#28026);
#2123=PLANE('',#28027);
#2124=PLANE('',#28028);
#2125=PLANE('',#28029);
#2126=PLANE('',#28030);
#2127=PLANE('',#28031);
#2128=PLANE('',#28032);
#2129=PLANE('',#28033);
#2130=PLANE('',#28034);
#2131=PLANE('',#28035);
#2132=PLANE('',#28036);
#2133=PLANE('',#28037);
#2134=PLANE('',#28038);
#2135=PLANE('',#28039);
#2136=PLANE('',#28040);
#2137=PLANE('',#28041);
#2138=PLANE('',#28042);
#2139=PLANE('',#28043);
#2140=PLANE('',#28044);
#2141=PLANE('',#28045);
#2142=PLANE('',#28046);
#2143=PLANE('',#28047);
#2144=PLANE('',#28048);
#2145=PLANE('',#28049);
#2146=PLANE('',#28050);
#2147=PLANE('',#28051);
#2148=PLANE('',#28052);
#2149=PLANE('',#28053);
#2150=PLANE('',#28054);
#2151=PLANE('',#28055);
#2152=PLANE('',#28056);
#2153=PLANE('',#28057);
#2154=PLANE('',#28058);
#2155=PLANE('',#28059);
#2156=PLANE('',#28060);
#2157=PLANE('',#28061);
#2158=PLANE('',#28062);
#2159=PLANE('',#28063);
#2160=PLANE('',#28064);
#2161=PLANE('',#28065);
#2162=PLANE('',#28066);
#2163=PLANE('',#28067);
#2164=PLANE('',#28068);
#2165=PLANE('',#28069);
#2166=PLANE('',#28070);
#2167=PLANE('',#28071);
#2168=PLANE('',#28072);
#2169=PLANE('',#28073);
#2170=PLANE('',#28074);
#2171=PLANE('',#28075);
#2172=PLANE('',#28076);
#2173=PLANE('',#28077);
#2174=PLANE('',#28078);
#2175=PLANE('',#28079);
#2176=PLANE('',#28080);
#2177=PLANE('',#28081);
#2178=PLANE('',#28082);
#2179=PLANE('',#28083);
#2180=PLANE('',#28084);
#2181=PLANE('',#28085);
#2182=PLANE('',#28086);
#2183=PLANE('',#28087);
#2184=PLANE('',#28088);
#2185=PLANE('',#28089);
#2186=PLANE('',#28090);
#2187=PLANE('',#28091);
#2188=PLANE('',#28092);
#2189=PLANE('',#28093);
#2190=PLANE('',#28094);
#2191=PLANE('',#28095);
#2192=PLANE('',#28096);
#2193=PLANE('',#28097);
#2194=PLANE('',#28098);
#2195=PLANE('',#28099);
#2196=PLANE('',#28100);
#2197=PLANE('',#28101);
#2198=PLANE('',#28102);
#2199=PLANE('',#28103);
#2200=PLANE('',#28104);
#2201=PLANE('',#28105);
#2202=PLANE('',#28106);
#2203=PLANE('',#28107);
#2204=PLANE('',#28108);
#2205=PLANE('',#28109);
#2206=PLANE('',#28110);
#2207=PLANE('',#28111);
#2208=PLANE('',#28112);
#2209=PLANE('',#28113);
#2210=PLANE('',#28114);
#2211=PLANE('',#28115);
#2212=PLANE('',#28116);
#2213=PLANE('',#28117);
#2214=PLANE('',#28118);
#2215=PLANE('',#28119);
#2216=PLANE('',#28120);
#2217=PLANE('',#28121);
#2218=PLANE('',#28122);
#2219=PLANE('',#28123);
#2220=PLANE('',#28124);
#2221=PLANE('',#28125);
#2222=PLANE('',#28126);
#2223=PLANE('',#28127);
#2224=PLANE('',#28128);
#2225=PLANE('',#28129);
#2226=PLANE('',#28130);
#2227=PLANE('',#28131);
#2228=PLANE('',#28132);
#2229=PLANE('',#28133);
#2230=PLANE('',#28134);
#2231=PLANE('',#28135);
#2232=PLANE('',#28136);
#2233=PLANE('',#28137);
#2234=PLANE('',#28138);
#2235=PLANE('',#28139);
#2236=PLANE('',#28140);
#2237=PLANE('',#28141);
#2238=PLANE('',#28142);
#2239=PLANE('',#28143);
#2240=PLANE('',#28144);
#2241=PLANE('',#28145);
#2242=PLANE('',#28146);
#2243=PLANE('',#28147);
#2244=PLANE('',#28148);
#2245=PLANE('',#28149);
#2246=PLANE('',#28150);
#2247=PLANE('',#28151);
#2248=PLANE('',#28152);
#2249=PLANE('',#28153);
#2250=PLANE('',#28154);
#2251=PLANE('',#28155);
#2252=PLANE('',#28156);
#2253=PLANE('',#28157);
#2254=PLANE('',#28158);
#2255=PLANE('',#28159);
#2256=PLANE('',#28160);
#2257=PLANE('',#28161);
#2258=PLANE('',#28162);
#2259=PLANE('',#28163);
#2260=PLANE('',#28164);
#2261=PLANE('',#28165);
#2262=PLANE('',#28166);
#2263=PLANE('',#28168);
#2264=PLANE('',#28169);
#2265=PLANE('',#28170);
#2266=PLANE('',#28171);
#2267=PLANE('',#28172);
#2268=PLANE('',#28173);
#2269=PLANE('',#28174);
#2270=PLANE('',#28175);
#2271=PLANE('',#28176);
#2272=PLANE('',#28177);
#2273=PLANE('',#28178);
#2274=PLANE('',#28179);
#2275=PLANE('',#28180);
#2276=PLANE('',#28181);
#2277=PLANE('',#28182);
#2278=PLANE('',#28183);
#2279=PLANE('',#28184);
#2280=PLANE('',#28185);
#2281=PLANE('',#28186);
#2282=PLANE('',#28187);
#2283=PLANE('',#28188);
#2284=PLANE('',#28189);
#2285=PLANE('',#28190);
#2286=PLANE('',#28191);
#2287=PLANE('',#28192);
#2288=PLANE('',#28193);
#2289=PLANE('',#28194);
#2290=PLANE('',#28195);
#2291=PLANE('',#28196);
#2292=PLANE('',#28197);
#2293=PLANE('',#28198);
#2294=PLANE('',#28199);
#2295=PLANE('',#28200);
#2296=PLANE('',#28201);
#2297=PLANE('',#28202);
#2298=PLANE('',#28203);
#2299=PLANE('',#28204);
#2300=PLANE('',#28205);
#2301=PLANE('',#28206);
#2302=PLANE('',#28207);
#2303=PLANE('',#28208);
#2304=PLANE('',#28209);
#2305=PLANE('',#28210);
#2306=PLANE('',#28211);
#2307=PLANE('',#28212);
#2308=PLANE('',#28213);
#2309=PLANE('',#28214);
#2310=PLANE('',#28215);
#2311=PLANE('',#28216);
#2312=PLANE('',#28217);
#2313=PLANE('',#28218);
#2314=PLANE('',#28219);
#2315=PLANE('',#28220);
#2316=PLANE('',#28221);
#2317=PLANE('',#28222);
#2318=PLANE('',#28223);
#2319=PLANE('',#28224);
#2320=PLANE('',#28225);
#2321=PLANE('',#28226);
#2322=PLANE('',#28227);
#2323=PLANE('',#28228);
#2324=PLANE('',#28229);
#2325=PLANE('',#28230);
#2326=PLANE('',#28231);
#2327=PLANE('',#28232);
#2328=PLANE('',#28233);
#2329=PLANE('',#28234);
#2330=PLANE('',#28235);
#2331=PLANE('',#28236);
#2332=PLANE('',#28237);
#2333=PLANE('',#28238);
#2334=PLANE('',#28239);
#2335=PLANE('',#28240);
#2336=PLANE('',#28241);
#2337=PLANE('',#28242);
#2338=PLANE('',#28243);
#2339=PLANE('',#28244);
#2340=PLANE('',#28245);
#2341=PLANE('',#28246);
#2342=PLANE('',#28247);
#2343=PLANE('',#28248);
#2344=PLANE('',#28249);
#2345=PLANE('',#28250);
#2346=PLANE('',#28251);
#2347=PLANE('',#28252);
#2348=PLANE('',#28253);
#2349=PLANE('',#28254);
#2350=PLANE('',#28255);
#2351=PLANE('',#28256);
#2352=PLANE('',#28257);
#2353=PLANE('',#28258);
#2354=PLANE('',#28259);
#2355=PLANE('',#28260);
#2356=PLANE('',#28261);
#2357=PLANE('',#28262);
#2358=PLANE('',#28263);
#2359=PLANE('',#28264);
#2360=PLANE('',#28265);
#2361=PLANE('',#28266);
#2362=PLANE('',#28267);
#2363=PLANE('',#28268);
#2364=PLANE('',#28269);
#2365=PLANE('',#28270);
#2366=PLANE('',#28271);
#2367=PLANE('',#28272);
#2368=PLANE('',#28273);
#2369=PLANE('',#28274);
#2370=PLANE('',#28275);
#2371=PLANE('',#28276);
#2372=PLANE('',#28277);
#2373=PLANE('',#28286);
#2374=PLANE('',#28287);
#2375=PLANE('',#28288);
#2376=PLANE('',#28289);
#2377=PLANE('',#28290);
#2378=PLANE('',#28291);
#2379=PLANE('',#28292);
#2380=PLANE('',#28293);
#2381=PLANE('',#28294);
#2382=PLANE('',#28295);
#2383=PLANE('',#28296);
#2384=PLANE('',#28297);
#2385=PLANE('',#28298);
#2386=PLANE('',#28299);
#2387=PLANE('',#28300);
#2388=PLANE('',#28301);
#2389=PLANE('',#28302);
#2390=PLANE('',#28303);
#2391=PLANE('',#28304);
#2392=PLANE('',#28306);
#2393=PLANE('',#28310);
#2394=PLANE('',#28311);
#2395=PLANE('',#28315);
#2396=PLANE('',#28316);
#2397=PLANE('',#28320);
#2398=PLANE('',#28321);
#2399=PLANE('',#28325);
#2400=PLANE('',#28326);
#2401=PLANE('',#28330);
#2402=PLANE('',#28331);
#2403=PLANE('',#28335);
#2404=PLANE('',#28336);
#2405=PLANE('',#28340);
#2406=PLANE('',#28341);
#2407=PLANE('',#28345);
#2408=PLANE('',#28346);
#2409=PLANE('',#28348);
#2410=PLANE('',#28350);
#2411=PLANE('',#28353);
#2412=PLANE('',#28356);
#2413=PLANE('',#28358);
#2414=PLANE('',#28360);
#2415=PLANE('',#28362);
#2416=PLANE('',#28364);
#2417=PLANE('',#28366);
#2418=PLANE('',#28368);
#2419=PLANE('',#28370);
#2420=PLANE('',#28372);
#2421=PLANE('',#28374);
#2422=PLANE('',#28376);
#2423=PLANE('',#28378);
#2424=PLANE('',#28383);
#2425=PLANE('',#28388);
#2426=PLANE('',#28411);
#2427=PLANE('',#28412);
#2428=PLANE('',#28421);
#2429=PLANE('',#28422);
#2430=PLANE('',#28423);
#2431=PLANE('',#28428);
#2432=PLANE('',#28429);
#2433=PLANE('',#28462);
#2434=PLANE('',#28463);
#2435=PLANE('',#28472);
#2436=PLANE('',#28474);
#2437=PLANE('',#28475);
#2438=PLANE('',#28482);
#2439=PLANE('',#28492);
#2440=PLANE('',#28523);
#2441=PLANE('',#28526);
#2442=PLANE('',#28539);
#2443=PLANE('',#28560);
#2444=PLANE('',#28567);
#2445=PLANE('',#28573);
#2446=PLANE('',#28604);
#2447=PLANE('',#28620);
#2448=PLANE('',#28623);
#2449=PLANE('',#28625);
#2450=PLANE('',#28629);
#2451=PLANE('',#28656);
#2452=PLANE('',#28659);
#2453=PLANE('',#28660);
#2454=PLANE('',#28663);
#2455=PLANE('',#28667);
#2456=PLANE('',#28671);
#2457=PLANE('',#28672);
#2458=PLANE('',#28673);
#2459=PLANE('',#28678);
#2460=PLANE('',#28688);
#2461=PLANE('',#28689);
#2462=PLANE('',#28690);
#2463=PLANE('',#28696);
#2464=PLANE('',#28707);
#2465=PLANE('',#28712);
#2466=PLANE('',#28715);
#2467=PLANE('',#28718);
#2468=PLANE('',#28720);
#2469=PLANE('',#28727);
#2470=PLANE('',#28732);
#2471=PLANE('',#28738);
#2472=PLANE('',#28739);
#2473=PLANE('',#28743);
#2474=PLANE('',#28744);
#2475=PLANE('',#28749);
#2476=PLANE('',#28750);
#2477=PLANE('',#28751);
#2478=PLANE('',#28752);
#2479=PLANE('',#28753);
#2480=PLANE('',#28756);
#2481=PLANE('',#28762);
#2482=PLANE('',#28764);
#2483=PLANE('',#28765);
#2484=PLANE('',#28766);
#2485=PLANE('',#28773);
#2486=PLANE('',#28774);
#2487=PLANE('',#28776);
#2488=PLANE('',#28777);
#2489=PLANE('',#28778);
#2490=PLANE('',#28779);
#2491=PLANE('',#28780);
#2492=PLANE('',#28781);
#2493=PLANE('',#28782);
#2494=PLANE('',#28783);
#2495=PLANE('',#28784);
#2496=PLANE('',#28785);
#2497=PLANE('',#28786);
#2498=PLANE('',#28787);
#2499=PLANE('',#28788);
#2500=PLANE('',#28789);
#2501=PLANE('',#28790);
#2502=PLANE('',#28791);
#2503=PLANE('',#28792);
#2504=PLANE('',#28793);
#2505=PLANE('',#28794);
#2506=PLANE('',#28795);
#2507=PLANE('',#28796);
#2508=PLANE('',#28797);
#2509=PLANE('',#28798);
#2510=PLANE('',#28799);
#2511=PLANE('',#28800);
#2512=PLANE('',#28803);
#2513=PLANE('',#28808);
#2514=PLANE('',#28809);
#2515=PLANE('',#28810);
#2516=PLANE('',#28812);
#2517=PLANE('',#28813);
#2518=PLANE('',#28814);
#2519=PLANE('',#28815);
#2520=PLANE('',#28816);
#2521=PLANE('',#28817);
#2522=PLANE('',#28818);
#2523=PLANE('',#28819);
#2524=PLANE('',#28822);
#2525=PLANE('',#28826);
#2526=PLANE('',#28832);
#2527=PLANE('',#28839);
#2528=PLANE('',#28842);
#2529=PLANE('',#28845);
#2530=PLANE('',#28846);
#2531=PLANE('',#28848);
#2532=PLANE('',#28849);
#2533=PLANE('',#28855);
#2534=PLANE('',#28857);
#2535=PLANE('',#28858);
#2536=PLANE('',#28859);
#2537=PLANE('',#28861);
#2538=PLANE('',#28862);
#2539=PLANE('',#28865);
#2540=PLANE('',#28870);
#2541=PLANE('',#28875);
#2542=PLANE('',#28878);
#2543=PLANE('',#28879);
#2544=PLANE('',#28883);
#2545=PLANE('',#28886);
#2546=PLANE('',#28888);
#2547=PLANE('',#28891);
#2548=PLANE('',#28925);
#2549=PLANE('',#28926);
#2550=PLANE('',#28927);
#2551=PLANE('',#28928);
#2552=PLANE('',#28929);
#2553=PLANE('',#28930);
#2554=PLANE('',#28931);
#2555=PLANE('',#28932);
#2556=PLANE('',#28933);
#2557=PLANE('',#28934);
#2558=PLANE('',#28935);
#2559=PLANE('',#28936);
#2560=PLANE('',#28939);
#2561=PLANE('',#28948);
#2562=PLANE('',#28952);
#2563=PLANE('',#28953);
#2564=PLANE('',#28954);
#2565=PLANE('',#28955);
#2566=PLANE('',#28956);
#2567=PLANE('',#28957);
#2568=PLANE('',#28958);
#2569=PLANE('',#28959);
#2570=FACE_OUTER_BOUND('',#4059,.T.);
#2571=FACE_OUTER_BOUND('',#4060,.T.);
#2572=FACE_OUTER_BOUND('',#4062,.T.);
#2573=FACE_OUTER_BOUND('',#4063,.T.);
#2574=FACE_OUTER_BOUND('',#4064,.T.);
#2575=FACE_OUTER_BOUND('',#4066,.T.);
#2576=FACE_OUTER_BOUND('',#4067,.T.);
#2577=FACE_OUTER_BOUND('',#4068,.T.);
#2578=FACE_OUTER_BOUND('',#4069,.T.);
#2579=FACE_OUTER_BOUND('',#4070,.T.);
#2580=FACE_OUTER_BOUND('',#4072,.T.);
#2581=FACE_OUTER_BOUND('',#4073,.T.);
#2582=FACE_OUTER_BOUND('',#4074,.T.);
#2583=FACE_OUTER_BOUND('',#4076,.T.);
#2584=FACE_OUTER_BOUND('',#4077,.T.);
#2585=FACE_OUTER_BOUND('',#4078,.T.);
#2586=FACE_OUTER_BOUND('',#4079,.T.);
#2587=FACE_OUTER_BOUND('',#4080,.T.);
#2588=FACE_OUTER_BOUND('',#4081,.T.);
#2589=FACE_OUTER_BOUND('',#4082,.T.);
#2590=FACE_OUTER_BOUND('',#4083,.T.);
#2591=FACE_OUTER_BOUND('',#4084,.T.);
#2592=FACE_OUTER_BOUND('',#4085,.T.);
#2593=FACE_OUTER_BOUND('',#4086,.T.);
#2594=FACE_OUTER_BOUND('',#4087,.T.);
#2595=FACE_OUTER_BOUND('',#4088,.T.);
#2596=FACE_OUTER_BOUND('',#4089,.T.);
#2597=FACE_OUTER_BOUND('',#4090,.T.);
#2598=FACE_OUTER_BOUND('',#4091,.T.);
#2599=FACE_OUTER_BOUND('',#4092,.T.);
#2600=FACE_OUTER_BOUND('',#4093,.T.);
#2601=FACE_OUTER_BOUND('',#4094,.T.);
#2602=FACE_OUTER_BOUND('',#4095,.T.);
#2603=FACE_OUTER_BOUND('',#4096,.T.);
#2604=FACE_OUTER_BOUND('',#4097,.T.);
#2605=FACE_OUTER_BOUND('',#4098,.T.);
#2606=FACE_OUTER_BOUND('',#4099,.T.);
#2607=FACE_OUTER_BOUND('',#4100,.T.);
#2608=FACE_OUTER_BOUND('',#4101,.T.);
#2609=FACE_OUTER_BOUND('',#4102,.T.);
#2610=FACE_OUTER_BOUND('',#4103,.T.);
#2611=FACE_OUTER_BOUND('',#4104,.T.);
#2612=FACE_OUTER_BOUND('',#4105,.T.);
#2613=FACE_OUTER_BOUND('',#4106,.T.);
#2614=FACE_OUTER_BOUND('',#4107,.T.);
#2615=FACE_OUTER_BOUND('',#4108,.T.);
#2616=FACE_OUTER_BOUND('',#4109,.T.);
#2617=FACE_OUTER_BOUND('',#4110,.T.);
#2618=FACE_OUTER_BOUND('',#4111,.T.);
#2619=FACE_OUTER_BOUND('',#4112,.T.);
#2620=FACE_OUTER_BOUND('',#4113,.T.);
#2621=FACE_OUTER_BOUND('',#4114,.T.);
#2622=FACE_OUTER_BOUND('',#4115,.T.);
#2623=FACE_OUTER_BOUND('',#4116,.T.);
#2624=FACE_OUTER_BOUND('',#4117,.T.);
#2625=FACE_OUTER_BOUND('',#4118,.T.);
#2626=FACE_OUTER_BOUND('',#4119,.T.);
#2627=FACE_OUTER_BOUND('',#4120,.T.);
#2628=FACE_OUTER_BOUND('',#4121,.T.);
#2629=FACE_OUTER_BOUND('',#4122,.T.);
#2630=FACE_OUTER_BOUND('',#4123,.T.);
#2631=FACE_OUTER_BOUND('',#4124,.T.);
#2632=FACE_OUTER_BOUND('',#4125,.T.);
#2633=FACE_OUTER_BOUND('',#4126,.T.);
#2634=FACE_OUTER_BOUND('',#4127,.T.);
#2635=FACE_OUTER_BOUND('',#4128,.T.);
#2636=FACE_OUTER_BOUND('',#4129,.T.);
#2637=FACE_OUTER_BOUND('',#4130,.T.);
#2638=FACE_OUTER_BOUND('',#4131,.T.);
#2639=FACE_OUTER_BOUND('',#4132,.T.);
#2640=FACE_OUTER_BOUND('',#4133,.T.);
#2641=FACE_OUTER_BOUND('',#4134,.T.);
#2642=FACE_OUTER_BOUND('',#4135,.T.);
#2643=FACE_OUTER_BOUND('',#4136,.T.);
#2644=FACE_OUTER_BOUND('',#4137,.T.);
#2645=FACE_OUTER_BOUND('',#4138,.T.);
#2646=FACE_OUTER_BOUND('',#4139,.T.);
#2647=FACE_OUTER_BOUND('',#4140,.T.);
#2648=FACE_OUTER_BOUND('',#4141,.T.);
#2649=FACE_OUTER_BOUND('',#4142,.T.);
#2650=FACE_OUTER_BOUND('',#4143,.T.);
#2651=FACE_OUTER_BOUND('',#4144,.T.);
#2652=FACE_OUTER_BOUND('',#4145,.T.);
#2653=FACE_OUTER_BOUND('',#4146,.T.);
#2654=FACE_OUTER_BOUND('',#4147,.T.);
#2655=FACE_OUTER_BOUND('',#4148,.T.);
#2656=FACE_OUTER_BOUND('',#4149,.T.);
#2657=FACE_OUTER_BOUND('',#4150,.T.);
#2658=FACE_OUTER_BOUND('',#4151,.T.);
#2659=FACE_OUTER_BOUND('',#4152,.T.);
#2660=FACE_OUTER_BOUND('',#4153,.T.);
#2661=FACE_OUTER_BOUND('',#4154,.T.);
#2662=FACE_OUTER_BOUND('',#4155,.T.);
#2663=FACE_OUTER_BOUND('',#4156,.T.);
#2664=FACE_OUTER_BOUND('',#4157,.T.);
#2665=FACE_OUTER_BOUND('',#4158,.T.);
#2666=FACE_OUTER_BOUND('',#4159,.T.);
#2667=FACE_OUTER_BOUND('',#4160,.T.);
#2668=FACE_OUTER_BOUND('',#4161,.T.);
#2669=FACE_OUTER_BOUND('',#4162,.T.);
#2670=FACE_OUTER_BOUND('',#4163,.T.);
#2671=FACE_OUTER_BOUND('',#4164,.T.);
#2672=FACE_OUTER_BOUND('',#4165,.T.);
#2673=FACE_OUTER_BOUND('',#4166,.T.);
#2674=FACE_OUTER_BOUND('',#4167,.T.);
#2675=FACE_OUTER_BOUND('',#4168,.T.);
#2676=FACE_OUTER_BOUND('',#4169,.T.);
#2677=FACE_OUTER_BOUND('',#4170,.T.);
#2678=FACE_OUTER_BOUND('',#4171,.T.);
#2679=FACE_OUTER_BOUND('',#4172,.T.);
#2680=FACE_OUTER_BOUND('',#4173,.T.);
#2681=FACE_OUTER_BOUND('',#4174,.T.);
#2682=FACE_OUTER_BOUND('',#4175,.T.);
#2683=FACE_OUTER_BOUND('',#4176,.T.);
#2684=FACE_OUTER_BOUND('',#4177,.T.);
#2685=FACE_OUTER_BOUND('',#4178,.T.);
#2686=FACE_OUTER_BOUND('',#4179,.T.);
#2687=FACE_OUTER_BOUND('',#4180,.T.);
#2688=FACE_OUTER_BOUND('',#4181,.T.);
#2689=FACE_OUTER_BOUND('',#4182,.T.);
#2690=FACE_OUTER_BOUND('',#4183,.T.);
#2691=FACE_OUTER_BOUND('',#4184,.T.);
#2692=FACE_OUTER_BOUND('',#4185,.T.);
#2693=FACE_OUTER_BOUND('',#4186,.T.);
#2694=FACE_OUTER_BOUND('',#4187,.T.);
#2695=FACE_OUTER_BOUND('',#4188,.T.);
#2696=FACE_OUTER_BOUND('',#4189,.T.);
#2697=FACE_OUTER_BOUND('',#4190,.T.);
#2698=FACE_OUTER_BOUND('',#4191,.T.);
#2699=FACE_OUTER_BOUND('',#4192,.T.);
#2700=FACE_OUTER_BOUND('',#4193,.T.);
#2701=FACE_OUTER_BOUND('',#4194,.T.);
#2702=FACE_OUTER_BOUND('',#4195,.T.);
#2703=FACE_OUTER_BOUND('',#4196,.T.);
#2704=FACE_OUTER_BOUND('',#4197,.T.);
#2705=FACE_OUTER_BOUND('',#4198,.T.);
#2706=FACE_OUTER_BOUND('',#4199,.T.);
#2707=FACE_OUTER_BOUND('',#4200,.T.);
#2708=FACE_OUTER_BOUND('',#4201,.T.);
#2709=FACE_OUTER_BOUND('',#4202,.T.);
#2710=FACE_OUTER_BOUND('',#4203,.T.);
#2711=FACE_OUTER_BOUND('',#4204,.T.);
#2712=FACE_OUTER_BOUND('',#4205,.T.);
#2713=FACE_OUTER_BOUND('',#4206,.T.);
#2714=FACE_OUTER_BOUND('',#4207,.T.);
#2715=FACE_OUTER_BOUND('',#4208,.T.);
#2716=FACE_OUTER_BOUND('',#4209,.T.);
#2717=FACE_OUTER_BOUND('',#4210,.T.);
#2718=FACE_OUTER_BOUND('',#4211,.T.);
#2719=FACE_OUTER_BOUND('',#4212,.T.);
#2720=FACE_OUTER_BOUND('',#4213,.T.);
#2721=FACE_OUTER_BOUND('',#4214,.T.);
#2722=FACE_OUTER_BOUND('',#4215,.T.);
#2723=FACE_OUTER_BOUND('',#4216,.T.);
#2724=FACE_OUTER_BOUND('',#4217,.T.);
#2725=FACE_OUTER_BOUND('',#4218,.T.);
#2726=FACE_OUTER_BOUND('',#4219,.T.);
#2727=FACE_OUTER_BOUND('',#4220,.T.);
#2728=FACE_OUTER_BOUND('',#4221,.T.);
#2729=FACE_OUTER_BOUND('',#4222,.T.);
#2730=FACE_OUTER_BOUND('',#4224,.T.);
#2731=FACE_OUTER_BOUND('',#4225,.T.);
#2732=FACE_OUTER_BOUND('',#4226,.T.);
#2733=FACE_OUTER_BOUND('',#4227,.T.);
#2734=FACE_OUTER_BOUND('',#4228,.T.);
#2735=FACE_OUTER_BOUND('',#4229,.T.);
#2736=FACE_OUTER_BOUND('',#4230,.T.);
#2737=FACE_OUTER_BOUND('',#4231,.T.);
#2738=FACE_OUTER_BOUND('',#4232,.T.);
#2739=FACE_OUTER_BOUND('',#4233,.T.);
#2740=FACE_OUTER_BOUND('',#4234,.T.);
#2741=FACE_OUTER_BOUND('',#4235,.T.);
#2742=FACE_OUTER_BOUND('',#4236,.T.);
#2743=FACE_OUTER_BOUND('',#4237,.T.);
#2744=FACE_OUTER_BOUND('',#4239,.T.);
#2745=FACE_OUTER_BOUND('',#4240,.T.);
#2746=FACE_OUTER_BOUND('',#4241,.T.);
#2747=FACE_OUTER_BOUND('',#4242,.T.);
#2748=FACE_OUTER_BOUND('',#4243,.T.);
#2749=FACE_OUTER_BOUND('',#4244,.T.);
#2750=FACE_OUTER_BOUND('',#4245,.T.);
#2751=FACE_OUTER_BOUND('',#4246,.T.);
#2752=FACE_OUTER_BOUND('',#4247,.T.);
#2753=FACE_OUTER_BOUND('',#4248,.T.);
#2754=FACE_OUTER_BOUND('',#4249,.T.);
#2755=FACE_OUTER_BOUND('',#4250,.T.);
#2756=FACE_OUTER_BOUND('',#4251,.T.);
#2757=FACE_OUTER_BOUND('',#4252,.T.);
#2758=FACE_OUTER_BOUND('',#4253,.T.);
#2759=FACE_OUTER_BOUND('',#4254,.T.);
#2760=FACE_OUTER_BOUND('',#4255,.T.);
#2761=FACE_OUTER_BOUND('',#4256,.T.);
#2762=FACE_OUTER_BOUND('',#4257,.T.);
#2763=FACE_OUTER_BOUND('',#4258,.T.);
#2764=FACE_OUTER_BOUND('',#4259,.T.);
#2765=FACE_OUTER_BOUND('',#4260,.T.);
#2766=FACE_OUTER_BOUND('',#4261,.T.);
#2767=FACE_OUTER_BOUND('',#4262,.T.);
#2768=FACE_OUTER_BOUND('',#4263,.T.);
#2769=FACE_OUTER_BOUND('',#4264,.T.);
#2770=FACE_OUTER_BOUND('',#4265,.T.);
#2771=FACE_OUTER_BOUND('',#4266,.T.);
#2772=FACE_OUTER_BOUND('',#4267,.T.);
#2773=FACE_OUTER_BOUND('',#4268,.T.);
#2774=FACE_OUTER_BOUND('',#4269,.T.);
#2775=FACE_OUTER_BOUND('',#4270,.T.);
#2776=FACE_OUTER_BOUND('',#4271,.T.);
#2777=FACE_OUTER_BOUND('',#4272,.T.);
#2778=FACE_OUTER_BOUND('',#4273,.T.);
#2779=FACE_OUTER_BOUND('',#4274,.T.);
#2780=FACE_OUTER_BOUND('',#4275,.T.);
#2781=FACE_OUTER_BOUND('',#4276,.T.);
#2782=FACE_OUTER_BOUND('',#4277,.T.);
#2783=FACE_OUTER_BOUND('',#4278,.T.);
#2784=FACE_OUTER_BOUND('',#4279,.T.);
#2785=FACE_OUTER_BOUND('',#4280,.T.);
#2786=FACE_OUTER_BOUND('',#4281,.T.);
#2787=FACE_OUTER_BOUND('',#4282,.T.);
#2788=FACE_OUTER_BOUND('',#4283,.T.);
#2789=FACE_OUTER_BOUND('',#4284,.T.);
#2790=FACE_OUTER_BOUND('',#4285,.T.);
#2791=FACE_OUTER_BOUND('',#4286,.T.);
#2792=FACE_OUTER_BOUND('',#4288,.T.);
#2793=FACE_OUTER_BOUND('',#4289,.T.);
#2794=FACE_OUTER_BOUND('',#4290,.T.);
#2795=FACE_OUTER_BOUND('',#4291,.T.);
#2796=FACE_OUTER_BOUND('',#4292,.T.);
#2797=FACE_OUTER_BOUND('',#4293,.T.);
#2798=FACE_OUTER_BOUND('',#4294,.T.);
#2799=FACE_OUTER_BOUND('',#4295,.T.);
#2800=FACE_OUTER_BOUND('',#4296,.T.);
#2801=FACE_OUTER_BOUND('',#4297,.T.);
#2802=FACE_OUTER_BOUND('',#4298,.T.);
#2803=FACE_OUTER_BOUND('',#4299,.T.);
#2804=FACE_OUTER_BOUND('',#4300,.T.);
#2805=FACE_OUTER_BOUND('',#4301,.T.);
#2806=FACE_OUTER_BOUND('',#4308,.T.);
#2807=FACE_OUTER_BOUND('',#4309,.T.);
#2808=FACE_OUTER_BOUND('',#4311,.T.);
#2809=FACE_OUTER_BOUND('',#4312,.T.);
#2810=FACE_OUTER_BOUND('',#4313,.T.);
#2811=FACE_OUTER_BOUND('',#4314,.T.);
#2812=FACE_OUTER_BOUND('',#4315,.T.);
#2813=FACE_OUTER_BOUND('',#4316,.T.);
#2814=FACE_OUTER_BOUND('',#4317,.T.);
#2815=FACE_OUTER_BOUND('',#4318,.T.);
#2816=FACE_OUTER_BOUND('',#4319,.T.);
#2817=FACE_OUTER_BOUND('',#4321,.T.);
#2818=FACE_OUTER_BOUND('',#4322,.T.);
#2819=FACE_OUTER_BOUND('',#4323,.T.);
#2820=FACE_OUTER_BOUND('',#4325,.T.);
#2821=FACE_OUTER_BOUND('',#4326,.T.);
#2822=FACE_OUTER_BOUND('',#4327,.T.);
#2823=FACE_OUTER_BOUND('',#4328,.T.);
#2824=FACE_OUTER_BOUND('',#4329,.T.);
#2825=FACE_OUTER_BOUND('',#4330,.T.);
#2826=FACE_OUTER_BOUND('',#4331,.T.);
#2827=FACE_OUTER_BOUND('',#4332,.T.);
#2828=FACE_OUTER_BOUND('',#4333,.T.);
#2829=FACE_OUTER_BOUND('',#4334,.T.);
#2830=FACE_OUTER_BOUND('',#4335,.T.);
#2831=FACE_OUTER_BOUND('',#4336,.T.);
#2832=FACE_OUTER_BOUND('',#4337,.T.);
#2833=FACE_OUTER_BOUND('',#4338,.T.);
#2834=FACE_OUTER_BOUND('',#4339,.T.);
#2835=FACE_OUTER_BOUND('',#4340,.T.);
#2836=FACE_OUTER_BOUND('',#4341,.T.);
#2837=FACE_OUTER_BOUND('',#4342,.T.);
#2838=FACE_OUTER_BOUND('',#4343,.T.);
#2839=FACE_OUTER_BOUND('',#4344,.T.);
#2840=FACE_OUTER_BOUND('',#4345,.T.);
#2841=FACE_OUTER_BOUND('',#4346,.T.);
#2842=FACE_OUTER_BOUND('',#4347,.T.);
#2843=FACE_OUTER_BOUND('',#4348,.T.);
#2844=FACE_OUTER_BOUND('',#4349,.T.);
#2845=FACE_OUTER_BOUND('',#4350,.T.);
#2846=FACE_OUTER_BOUND('',#4351,.T.);
#2847=FACE_OUTER_BOUND('',#4352,.T.);
#2848=FACE_OUTER_BOUND('',#4353,.T.);
#2849=FACE_OUTER_BOUND('',#4354,.T.);
#2850=FACE_OUTER_BOUND('',#4355,.T.);
#2851=FACE_OUTER_BOUND('',#4356,.T.);
#2852=FACE_OUTER_BOUND('',#4357,.T.);
#2853=FACE_OUTER_BOUND('',#4358,.T.);
#2854=FACE_OUTER_BOUND('',#4359,.T.);
#2855=FACE_OUTER_BOUND('',#4360,.T.);
#2856=FACE_OUTER_BOUND('',#4361,.T.);
#2857=FACE_OUTER_BOUND('',#4362,.T.);
#2858=FACE_OUTER_BOUND('',#4363,.T.);
#2859=FACE_OUTER_BOUND('',#4364,.T.);
#2860=FACE_OUTER_BOUND('',#4365,.T.);
#2861=FACE_OUTER_BOUND('',#4366,.T.);
#2862=FACE_OUTER_BOUND('',#4367,.T.);
#2863=FACE_OUTER_BOUND('',#4368,.T.);
#2864=FACE_OUTER_BOUND('',#4369,.T.);
#2865=FACE_OUTER_BOUND('',#4370,.T.);
#2866=FACE_OUTER_BOUND('',#4371,.T.);
#2867=FACE_OUTER_BOUND('',#4372,.T.);
#2868=FACE_OUTER_BOUND('',#4373,.T.);
#2869=FACE_OUTER_BOUND('',#4374,.T.);
#2870=FACE_OUTER_BOUND('',#4375,.T.);
#2871=FACE_OUTER_BOUND('',#4376,.T.);
#2872=FACE_OUTER_BOUND('',#4377,.T.);
#2873=FACE_OUTER_BOUND('',#4378,.T.);
#2874=FACE_OUTER_BOUND('',#4379,.T.);
#2875=FACE_OUTER_BOUND('',#4380,.T.);
#2876=FACE_OUTER_BOUND('',#4382,.T.);
#2877=FACE_OUTER_BOUND('',#4383,.T.);
#2878=FACE_OUTER_BOUND('',#4384,.T.);
#2879=FACE_OUTER_BOUND('',#4385,.T.);
#2880=FACE_OUTER_BOUND('',#4386,.T.);
#2881=FACE_OUTER_BOUND('',#4387,.T.);
#2882=FACE_OUTER_BOUND('',#4388,.T.);
#2883=FACE_OUTER_BOUND('',#4389,.T.);
#2884=FACE_OUTER_BOUND('',#4390,.T.);
#2885=FACE_OUTER_BOUND('',#4391,.T.);
#2886=FACE_OUTER_BOUND('',#4392,.T.);
#2887=FACE_OUTER_BOUND('',#4393,.T.);
#2888=FACE_OUTER_BOUND('',#4394,.T.);
#2889=FACE_OUTER_BOUND('',#4395,.T.);
#2890=FACE_OUTER_BOUND('',#4396,.T.);
#2891=FACE_OUTER_BOUND('',#4397,.T.);
#2892=FACE_OUTER_BOUND('',#4398,.T.);
#2893=FACE_OUTER_BOUND('',#4399,.T.);
#2894=FACE_OUTER_BOUND('',#4400,.T.);
#2895=FACE_OUTER_BOUND('',#4401,.T.);
#2896=FACE_OUTER_BOUND('',#4402,.T.);
#2897=FACE_OUTER_BOUND('',#4403,.T.);
#2898=FACE_OUTER_BOUND('',#4404,.T.);
#2899=FACE_OUTER_BOUND('',#4405,.T.);
#2900=FACE_OUTER_BOUND('',#4406,.T.);
#2901=FACE_OUTER_BOUND('',#4407,.T.);
#2902=FACE_OUTER_BOUND('',#4408,.T.);
#2903=FACE_OUTER_BOUND('',#4409,.T.);
#2904=FACE_OUTER_BOUND('',#4410,.T.);
#2905=FACE_OUTER_BOUND('',#4411,.T.);
#2906=FACE_OUTER_BOUND('',#4412,.T.);
#2907=FACE_OUTER_BOUND('',#4413,.T.);
#2908=FACE_OUTER_BOUND('',#4414,.T.);
#2909=FACE_OUTER_BOUND('',#4415,.T.);
#2910=FACE_OUTER_BOUND('',#4416,.T.);
#2911=FACE_OUTER_BOUND('',#4419,.T.);
#2912=FACE_OUTER_BOUND('',#4420,.T.);
#2913=FACE_OUTER_BOUND('',#4421,.T.);
#2914=FACE_OUTER_BOUND('',#4422,.T.);
#2915=FACE_OUTER_BOUND('',#4423,.T.);
#2916=FACE_OUTER_BOUND('',#4424,.T.);
#2917=FACE_OUTER_BOUND('',#4425,.T.);
#2918=FACE_OUTER_BOUND('',#4426,.T.);
#2919=FACE_OUTER_BOUND('',#4427,.T.);
#2920=FACE_OUTER_BOUND('',#4428,.T.);
#2921=FACE_OUTER_BOUND('',#4429,.T.);
#2922=FACE_OUTER_BOUND('',#4430,.T.);
#2923=FACE_OUTER_BOUND('',#4431,.T.);
#2924=FACE_OUTER_BOUND('',#4432,.T.);
#2925=FACE_OUTER_BOUND('',#4433,.T.);
#2926=FACE_OUTER_BOUND('',#4434,.T.);
#2927=FACE_OUTER_BOUND('',#4435,.T.);
#2928=FACE_OUTER_BOUND('',#4436,.T.);
#2929=FACE_OUTER_BOUND('',#4437,.T.);
#2930=FACE_OUTER_BOUND('',#4438,.T.);
#2931=FACE_OUTER_BOUND('',#4439,.T.);
#2932=FACE_OUTER_BOUND('',#4440,.T.);
#2933=FACE_OUTER_BOUND('',#4441,.T.);
#2934=FACE_OUTER_BOUND('',#4442,.T.);
#2935=FACE_OUTER_BOUND('',#4443,.T.);
#2936=FACE_OUTER_BOUND('',#4444,.T.);
#2937=FACE_OUTER_BOUND('',#4445,.T.);
#2938=FACE_OUTER_BOUND('',#4446,.T.);
#2939=FACE_OUTER_BOUND('',#4447,.T.);
#2940=FACE_OUTER_BOUND('',#4448,.T.);
#2941=FACE_OUTER_BOUND('',#4449,.T.);
#2942=FACE_OUTER_BOUND('',#4450,.T.);
#2943=FACE_OUTER_BOUND('',#4451,.T.);
#2944=FACE_OUTER_BOUND('',#4452,.T.);
#2945=FACE_OUTER_BOUND('',#4453,.T.);
#2946=FACE_OUTER_BOUND('',#4454,.T.);
#2947=FACE_OUTER_BOUND('',#4455,.T.);
#2948=FACE_OUTER_BOUND('',#4456,.T.);
#2949=FACE_OUTER_BOUND('',#4457,.T.);
#2950=FACE_OUTER_BOUND('',#4458,.T.);
#2951=FACE_OUTER_BOUND('',#4459,.T.);
#2952=FACE_OUTER_BOUND('',#4460,.T.);
#2953=FACE_OUTER_BOUND('',#4461,.T.);
#2954=FACE_OUTER_BOUND('',#4462,.T.);
#2955=FACE_OUTER_BOUND('',#4463,.T.);
#2956=FACE_OUTER_BOUND('',#4464,.T.);
#2957=FACE_OUTER_BOUND('',#4465,.T.);
#2958=FACE_OUTER_BOUND('',#4466,.T.);
#2959=FACE_OUTER_BOUND('',#4467,.T.);
#2960=FACE_OUTER_BOUND('',#4468,.T.);
#2961=FACE_OUTER_BOUND('',#4469,.T.);
#2962=FACE_OUTER_BOUND('',#4470,.T.);
#2963=FACE_OUTER_BOUND('',#4471,.T.);
#2964=FACE_OUTER_BOUND('',#4472,.T.);
#2965=FACE_OUTER_BOUND('',#4473,.T.);
#2966=FACE_OUTER_BOUND('',#4474,.T.);
#2967=FACE_OUTER_BOUND('',#4475,.T.);
#2968=FACE_OUTER_BOUND('',#4476,.T.);
#2969=FACE_OUTER_BOUND('',#4477,.T.);
#2970=FACE_OUTER_BOUND('',#4478,.T.);
#2971=FACE_OUTER_BOUND('',#4479,.T.);
#2972=FACE_OUTER_BOUND('',#4480,.T.);
#2973=FACE_OUTER_BOUND('',#4481,.T.);
#2974=FACE_OUTER_BOUND('',#4482,.T.);
#2975=FACE_OUTER_BOUND('',#4483,.T.);
#2976=FACE_OUTER_BOUND('',#4484,.T.);
#2977=FACE_OUTER_BOUND('',#4485,.T.);
#2978=FACE_OUTER_BOUND('',#4486,.T.);
#2979=FACE_OUTER_BOUND('',#4487,.T.);
#2980=FACE_OUTER_BOUND('',#4488,.T.);
#2981=FACE_OUTER_BOUND('',#4489,.T.);
#2982=FACE_OUTER_BOUND('',#4490,.T.);
#2983=FACE_OUTER_BOUND('',#4491,.T.);
#2984=FACE_OUTER_BOUND('',#4492,.T.);
#2985=FACE_OUTER_BOUND('',#4493,.T.);
#2986=FACE_OUTER_BOUND('',#4494,.T.);
#2987=FACE_OUTER_BOUND('',#4495,.T.);
#2988=FACE_OUTER_BOUND('',#4496,.T.);
#2989=FACE_OUTER_BOUND('',#4497,.T.);
#2990=FACE_OUTER_BOUND('',#4498,.T.);
#2991=FACE_OUTER_BOUND('',#4499,.T.);
#2992=FACE_OUTER_BOUND('',#4500,.T.);
#2993=FACE_OUTER_BOUND('',#4501,.T.);
#2994=FACE_OUTER_BOUND('',#4502,.T.);
#2995=FACE_OUTER_BOUND('',#4503,.T.);
#2996=FACE_OUTER_BOUND('',#4504,.T.);
#2997=FACE_OUTER_BOUND('',#4505,.T.);
#2998=FACE_OUTER_BOUND('',#4506,.T.);
#2999=FACE_OUTER_BOUND('',#4507,.T.);
#3000=FACE_OUTER_BOUND('',#4508,.T.);
#3001=FACE_OUTER_BOUND('',#4509,.T.);
#3002=FACE_OUTER_BOUND('',#4510,.T.);
#3003=FACE_OUTER_BOUND('',#4511,.T.);
#3004=FACE_OUTER_BOUND('',#4512,.T.);
#3005=FACE_OUTER_BOUND('',#4513,.T.);
#3006=FACE_OUTER_BOUND('',#4514,.T.);
#3007=FACE_OUTER_BOUND('',#4515,.T.);
#3008=FACE_OUTER_BOUND('',#4516,.T.);
#3009=FACE_OUTER_BOUND('',#4517,.T.);
#3010=FACE_OUTER_BOUND('',#4518,.T.);
#3011=FACE_OUTER_BOUND('',#4520,.T.);
#3012=FACE_OUTER_BOUND('',#4521,.T.);
#3013=FACE_OUTER_BOUND('',#4522,.T.);
#3014=FACE_OUTER_BOUND('',#4524,.T.);
#3015=FACE_OUTER_BOUND('',#4525,.T.);
#3016=FACE_OUTER_BOUND('',#4527,.T.);
#3017=FACE_OUTER_BOUND('',#4528,.T.);
#3018=FACE_OUTER_BOUND('',#4529,.T.);
#3019=FACE_OUTER_BOUND('',#4530,.T.);
#3020=FACE_OUTER_BOUND('',#4531,.T.);
#3021=FACE_OUTER_BOUND('',#4532,.T.);
#3022=FACE_OUTER_BOUND('',#4533,.T.);
#3023=FACE_OUTER_BOUND('',#4534,.T.);
#3024=FACE_OUTER_BOUND('',#4535,.T.);
#3025=FACE_OUTER_BOUND('',#4536,.T.);
#3026=FACE_OUTER_BOUND('',#4537,.T.);
#3027=FACE_OUTER_BOUND('',#4538,.T.);
#3028=FACE_OUTER_BOUND('',#4539,.T.);
#3029=FACE_OUTER_BOUND('',#4540,.T.);
#3030=FACE_OUTER_BOUND('',#4541,.T.);
#3031=FACE_OUTER_BOUND('',#4542,.T.);
#3032=FACE_OUTER_BOUND('',#4543,.T.);
#3033=FACE_OUTER_BOUND('',#4544,.T.);
#3034=FACE_OUTER_BOUND('',#4545,.T.);
#3035=FACE_OUTER_BOUND('',#4546,.T.);
#3036=FACE_OUTER_BOUND('',#4547,.T.);
#3037=FACE_OUTER_BOUND('',#4548,.T.);
#3038=FACE_OUTER_BOUND('',#4549,.T.);
#3039=FACE_OUTER_BOUND('',#4550,.T.);
#3040=FACE_OUTER_BOUND('',#4551,.T.);
#3041=FACE_OUTER_BOUND('',#4552,.T.);
#3042=FACE_OUTER_BOUND('',#4553,.T.);
#3043=FACE_OUTER_BOUND('',#4554,.T.);
#3044=FACE_OUTER_BOUND('',#4555,.T.);
#3045=FACE_OUTER_BOUND('',#4556,.T.);
#3046=FACE_OUTER_BOUND('',#4557,.T.);
#3047=FACE_OUTER_BOUND('',#4558,.T.);
#3048=FACE_OUTER_BOUND('',#4559,.T.);
#3049=FACE_OUTER_BOUND('',#4560,.T.);
#3050=FACE_OUTER_BOUND('',#4561,.T.);
#3051=FACE_OUTER_BOUND('',#4562,.T.);
#3052=FACE_OUTER_BOUND('',#4563,.T.);
#3053=FACE_OUTER_BOUND('',#4564,.T.);
#3054=FACE_OUTER_BOUND('',#4565,.T.);
#3055=FACE_OUTER_BOUND('',#4566,.T.);
#3056=FACE_OUTER_BOUND('',#4567,.T.);
#3057=FACE_OUTER_BOUND('',#4568,.T.);
#3058=FACE_OUTER_BOUND('',#4569,.T.);
#3059=FACE_OUTER_BOUND('',#4570,.T.);
#3060=FACE_OUTER_BOUND('',#4571,.T.);
#3061=FACE_OUTER_BOUND('',#4572,.T.);
#3062=FACE_OUTER_BOUND('',#4573,.T.);
#3063=FACE_OUTER_BOUND('',#4574,.T.);
#3064=FACE_OUTER_BOUND('',#4575,.T.);
#3065=FACE_OUTER_BOUND('',#4576,.T.);
#3066=FACE_OUTER_BOUND('',#4577,.T.);
#3067=FACE_OUTER_BOUND('',#4578,.T.);
#3068=FACE_OUTER_BOUND('',#4579,.T.);
#3069=FACE_OUTER_BOUND('',#4580,.T.);
#3070=FACE_OUTER_BOUND('',#4581,.T.);
#3071=FACE_OUTER_BOUND('',#4582,.T.);
#3072=FACE_OUTER_BOUND('',#4583,.T.);
#3073=FACE_OUTER_BOUND('',#4584,.T.);
#3074=FACE_OUTER_BOUND('',#4585,.T.);
#3075=FACE_OUTER_BOUND('',#4586,.T.);
#3076=FACE_OUTER_BOUND('',#4587,.T.);
#3077=FACE_OUTER_BOUND('',#4588,.T.);
#3078=FACE_OUTER_BOUND('',#4589,.T.);
#3079=FACE_OUTER_BOUND('',#4590,.T.);
#3080=FACE_OUTER_BOUND('',#4591,.T.);
#3081=FACE_OUTER_BOUND('',#4592,.T.);
#3082=FACE_OUTER_BOUND('',#4593,.T.);
#3083=FACE_OUTER_BOUND('',#4594,.T.);
#3084=FACE_OUTER_BOUND('',#4595,.T.);
#3085=FACE_OUTER_BOUND('',#4596,.T.);
#3086=FACE_OUTER_BOUND('',#4597,.T.);
#3087=FACE_OUTER_BOUND('',#4598,.T.);
#3088=FACE_OUTER_BOUND('',#4599,.T.);
#3089=FACE_OUTER_BOUND('',#4600,.T.);
#3090=FACE_OUTER_BOUND('',#4601,.T.);
#3091=FACE_OUTER_BOUND('',#4602,.T.);
#3092=FACE_OUTER_BOUND('',#4603,.T.);
#3093=FACE_OUTER_BOUND('',#4604,.T.);
#3094=FACE_OUTER_BOUND('',#4605,.T.);
#3095=FACE_OUTER_BOUND('',#4606,.T.);
#3096=FACE_OUTER_BOUND('',#4607,.T.);
#3097=FACE_OUTER_BOUND('',#4608,.T.);
#3098=FACE_OUTER_BOUND('',#4609,.T.);
#3099=FACE_OUTER_BOUND('',#4610,.T.);
#3100=FACE_OUTER_BOUND('',#4611,.T.);
#3101=FACE_OUTER_BOUND('',#4612,.T.);
#3102=FACE_OUTER_BOUND('',#4613,.T.);
#3103=FACE_OUTER_BOUND('',#4615,.T.);
#3104=FACE_OUTER_BOUND('',#4616,.T.);
#3105=FACE_OUTER_BOUND('',#4620,.T.);
#3106=FACE_OUTER_BOUND('',#4622,.T.);
#3107=FACE_OUTER_BOUND('',#4623,.T.);
#3108=FACE_OUTER_BOUND('',#4624,.T.);
#3109=FACE_OUTER_BOUND('',#4625,.T.);
#3110=FACE_OUTER_BOUND('',#4627,.T.);
#3111=FACE_OUTER_BOUND('',#4628,.T.);
#3112=FACE_OUTER_BOUND('',#4629,.T.);
#3113=FACE_OUTER_BOUND('',#4630,.T.);
#3114=FACE_OUTER_BOUND('',#4631,.T.);
#3115=FACE_OUTER_BOUND('',#4633,.T.);
#3116=FACE_OUTER_BOUND('',#4634,.T.);
#3117=FACE_OUTER_BOUND('',#4635,.T.);
#3118=FACE_OUTER_BOUND('',#4636,.T.);
#3119=FACE_OUTER_BOUND('',#4637,.T.);
#3120=FACE_OUTER_BOUND('',#4638,.T.);
#3121=FACE_OUTER_BOUND('',#4640,.T.);
#3122=FACE_OUTER_BOUND('',#4641,.T.);
#3123=FACE_OUTER_BOUND('',#4642,.T.);
#3124=FACE_OUTER_BOUND('',#4643,.T.);
#3125=FACE_OUTER_BOUND('',#4644,.T.);
#3126=FACE_OUTER_BOUND('',#4645,.T.);
#3127=FACE_OUTER_BOUND('',#4646,.T.);
#3128=FACE_OUTER_BOUND('',#4647,.T.);
#3129=FACE_OUTER_BOUND('',#4648,.T.);
#3130=FACE_OUTER_BOUND('',#4649,.T.);
#3131=FACE_OUTER_BOUND('',#4650,.T.);
#3132=FACE_OUTER_BOUND('',#4651,.T.);
#3133=FACE_OUTER_BOUND('',#4652,.T.);
#3134=FACE_OUTER_BOUND('',#4653,.T.);
#3135=FACE_OUTER_BOUND('',#4654,.T.);
#3136=FACE_OUTER_BOUND('',#4655,.T.);
#3137=FACE_OUTER_BOUND('',#4656,.T.);
#3138=FACE_OUTER_BOUND('',#4657,.T.);
#3139=FACE_OUTER_BOUND('',#4658,.T.);
#3140=FACE_OUTER_BOUND('',#4659,.T.);
#3141=FACE_OUTER_BOUND('',#4660,.T.);
#3142=FACE_OUTER_BOUND('',#4661,.T.);
#3143=FACE_OUTER_BOUND('',#4662,.T.);
#3144=FACE_OUTER_BOUND('',#4663,.T.);
#3145=FACE_OUTER_BOUND('',#4664,.T.);
#3146=FACE_OUTER_BOUND('',#4665,.T.);
#3147=FACE_OUTER_BOUND('',#4666,.T.);
#3148=FACE_OUTER_BOUND('',#4667,.T.);
#3149=FACE_OUTER_BOUND('',#4668,.T.);
#3150=FACE_OUTER_BOUND('',#4669,.T.);
#3151=FACE_OUTER_BOUND('',#4670,.T.);
#3152=FACE_OUTER_BOUND('',#4671,.T.);
#3153=FACE_OUTER_BOUND('',#4672,.T.);
#3154=FACE_OUTER_BOUND('',#4673,.T.);
#3155=FACE_OUTER_BOUND('',#4674,.T.);
#3156=FACE_OUTER_BOUND('',#4675,.T.);
#3157=FACE_OUTER_BOUND('',#4676,.T.);
#3158=FACE_OUTER_BOUND('',#4677,.T.);
#3159=FACE_OUTER_BOUND('',#4678,.T.);
#3160=FACE_OUTER_BOUND('',#4679,.T.);
#3161=FACE_OUTER_BOUND('',#4680,.T.);
#3162=FACE_OUTER_BOUND('',#4681,.T.);
#3163=FACE_OUTER_BOUND('',#4682,.T.);
#3164=FACE_OUTER_BOUND('',#4683,.T.);
#3165=FACE_OUTER_BOUND('',#4684,.T.);
#3166=FACE_OUTER_BOUND('',#4685,.T.);
#3167=FACE_OUTER_BOUND('',#4686,.T.);
#3168=FACE_OUTER_BOUND('',#4687,.T.);
#3169=FACE_OUTER_BOUND('',#4688,.T.);
#3170=FACE_OUTER_BOUND('',#4689,.T.);
#3171=FACE_OUTER_BOUND('',#4690,.T.);
#3172=FACE_OUTER_BOUND('',#4691,.T.);
#3173=FACE_OUTER_BOUND('',#4692,.T.);
#3174=FACE_OUTER_BOUND('',#4693,.T.);
#3175=FACE_OUTER_BOUND('',#4694,.T.);
#3176=FACE_OUTER_BOUND('',#4695,.T.);
#3177=FACE_OUTER_BOUND('',#4696,.T.);
#3178=FACE_OUTER_BOUND('',#4697,.T.);
#3179=FACE_OUTER_BOUND('',#4698,.T.);
#3180=FACE_OUTER_BOUND('',#4699,.T.);
#3181=FACE_OUTER_BOUND('',#4700,.T.);
#3182=FACE_OUTER_BOUND('',#4701,.T.);
#3183=FACE_OUTER_BOUND('',#4702,.T.);
#3184=FACE_OUTER_BOUND('',#4703,.T.);
#3185=FACE_OUTER_BOUND('',#4704,.T.);
#3186=FACE_OUTER_BOUND('',#4705,.T.);
#3187=FACE_OUTER_BOUND('',#4706,.T.);
#3188=FACE_OUTER_BOUND('',#4707,.T.);
#3189=FACE_OUTER_BOUND('',#4708,.T.);
#3190=FACE_OUTER_BOUND('',#4709,.T.);
#3191=FACE_OUTER_BOUND('',#4710,.T.);
#3192=FACE_OUTER_BOUND('',#4711,.T.);
#3193=FACE_OUTER_BOUND('',#4712,.T.);
#3194=FACE_OUTER_BOUND('',#4713,.T.);
#3195=FACE_OUTER_BOUND('',#4714,.T.);
#3196=FACE_OUTER_BOUND('',#4715,.T.);
#3197=FACE_OUTER_BOUND('',#4716,.T.);
#3198=FACE_OUTER_BOUND('',#4717,.T.);
#3199=FACE_OUTER_BOUND('',#4718,.T.);
#3200=FACE_OUTER_BOUND('',#4719,.T.);
#3201=FACE_OUTER_BOUND('',#4720,.T.);
#3202=FACE_OUTER_BOUND('',#4721,.T.);
#3203=FACE_OUTER_BOUND('',#4722,.T.);
#3204=FACE_OUTER_BOUND('',#4723,.T.);
#3205=FACE_OUTER_BOUND('',#4724,.T.);
#3206=FACE_OUTER_BOUND('',#4725,.T.);
#3207=FACE_OUTER_BOUND('',#4726,.T.);
#3208=FACE_OUTER_BOUND('',#4727,.T.);
#3209=FACE_OUTER_BOUND('',#4728,.T.);
#3210=FACE_OUTER_BOUND('',#4729,.T.);
#3211=FACE_OUTER_BOUND('',#4730,.T.);
#3212=FACE_OUTER_BOUND('',#4731,.T.);
#3213=FACE_OUTER_BOUND('',#4732,.T.);
#3214=FACE_OUTER_BOUND('',#4733,.T.);
#3215=FACE_OUTER_BOUND('',#4735,.T.);
#3216=FACE_OUTER_BOUND('',#4736,.T.);
#3217=FACE_OUTER_BOUND('',#4737,.T.);
#3218=FACE_OUTER_BOUND('',#4738,.T.);
#3219=FACE_OUTER_BOUND('',#4739,.T.);
#3220=FACE_OUTER_BOUND('',#4740,.T.);
#3221=FACE_OUTER_BOUND('',#4741,.T.);
#3222=FACE_OUTER_BOUND('',#4742,.T.);
#3223=FACE_OUTER_BOUND('',#4743,.T.);
#3224=FACE_OUTER_BOUND('',#4744,.T.);
#3225=FACE_OUTER_BOUND('',#4745,.T.);
#3226=FACE_OUTER_BOUND('',#4746,.T.);
#3227=FACE_OUTER_BOUND('',#4747,.T.);
#3228=FACE_OUTER_BOUND('',#4748,.T.);
#3229=FACE_OUTER_BOUND('',#4749,.T.);
#3230=FACE_OUTER_BOUND('',#4750,.T.);
#3231=FACE_OUTER_BOUND('',#4751,.T.);
#3232=FACE_OUTER_BOUND('',#4752,.T.);
#3233=FACE_OUTER_BOUND('',#4753,.T.);
#3234=FACE_OUTER_BOUND('',#4754,.T.);
#3235=FACE_OUTER_BOUND('',#4755,.T.);
#3236=FACE_OUTER_BOUND('',#4756,.T.);
#3237=FACE_OUTER_BOUND('',#4757,.T.);
#3238=FACE_OUTER_BOUND('',#4758,.T.);
#3239=FACE_OUTER_BOUND('',#4759,.T.);
#3240=FACE_OUTER_BOUND('',#4760,.T.);
#3241=FACE_OUTER_BOUND('',#4761,.T.);
#3242=FACE_OUTER_BOUND('',#4762,.T.);
#3243=FACE_OUTER_BOUND('',#4763,.T.);
#3244=FACE_OUTER_BOUND('',#4764,.T.);
#3245=FACE_OUTER_BOUND('',#4765,.T.);
#3246=FACE_OUTER_BOUND('',#4766,.T.);
#3247=FACE_OUTER_BOUND('',#4767,.T.);
#3248=FACE_OUTER_BOUND('',#4768,.T.);
#3249=FACE_OUTER_BOUND('',#4769,.T.);
#3250=FACE_OUTER_BOUND('',#4770,.T.);
#3251=FACE_OUTER_BOUND('',#4771,.T.);
#3252=FACE_OUTER_BOUND('',#4772,.T.);
#3253=FACE_OUTER_BOUND('',#4773,.T.);
#3254=FACE_OUTER_BOUND('',#4774,.T.);
#3255=FACE_OUTER_BOUND('',#4775,.T.);
#3256=FACE_OUTER_BOUND('',#4776,.T.);
#3257=FACE_OUTER_BOUND('',#4777,.T.);
#3258=FACE_OUTER_BOUND('',#4778,.T.);
#3259=FACE_OUTER_BOUND('',#4779,.T.);
#3260=FACE_OUTER_BOUND('',#4780,.T.);
#3261=FACE_OUTER_BOUND('',#4781,.T.);
#3262=FACE_OUTER_BOUND('',#4782,.T.);
#3263=FACE_OUTER_BOUND('',#4783,.T.);
#3264=FACE_OUTER_BOUND('',#4784,.T.);
#3265=FACE_OUTER_BOUND('',#4785,.T.);
#3266=FACE_OUTER_BOUND('',#4786,.T.);
#3267=FACE_OUTER_BOUND('',#4787,.T.);
#3268=FACE_OUTER_BOUND('',#4788,.T.);
#3269=FACE_OUTER_BOUND('',#4789,.T.);
#3270=FACE_OUTER_BOUND('',#4790,.T.);
#3271=FACE_OUTER_BOUND('',#4791,.T.);
#3272=FACE_OUTER_BOUND('',#4792,.T.);
#3273=FACE_OUTER_BOUND('',#4793,.T.);
#3274=FACE_OUTER_BOUND('',#4794,.T.);
#3275=FACE_OUTER_BOUND('',#4795,.T.);
#3276=FACE_OUTER_BOUND('',#4796,.T.);
#3277=FACE_OUTER_BOUND('',#4797,.T.);
#3278=FACE_OUTER_BOUND('',#4798,.T.);
#3279=FACE_OUTER_BOUND('',#4799,.T.);
#3280=FACE_OUTER_BOUND('',#4800,.T.);
#3281=FACE_OUTER_BOUND('',#4801,.T.);
#3282=FACE_OUTER_BOUND('',#4802,.T.);
#3283=FACE_OUTER_BOUND('',#4803,.T.);
#3284=FACE_OUTER_BOUND('',#4804,.T.);
#3285=FACE_OUTER_BOUND('',#4805,.T.);
#3286=FACE_OUTER_BOUND('',#4806,.T.);
#3287=FACE_OUTER_BOUND('',#4807,.T.);
#3288=FACE_OUTER_BOUND('',#4808,.T.);
#3289=FACE_OUTER_BOUND('',#4809,.T.);
#3290=FACE_OUTER_BOUND('',#4810,.T.);
#3291=FACE_OUTER_BOUND('',#4811,.T.);
#3292=FACE_OUTER_BOUND('',#4812,.T.);
#3293=FACE_OUTER_BOUND('',#4813,.T.);
#3294=FACE_OUTER_BOUND('',#4814,.T.);
#3295=FACE_OUTER_BOUND('',#4815,.T.);
#3296=FACE_OUTER_BOUND('',#4816,.T.);
#3297=FACE_OUTER_BOUND('',#4817,.T.);
#3298=FACE_OUTER_BOUND('',#4818,.T.);
#3299=FACE_OUTER_BOUND('',#4819,.T.);
#3300=FACE_OUTER_BOUND('',#4820,.T.);
#3301=FACE_OUTER_BOUND('',#4821,.T.);
#3302=FACE_OUTER_BOUND('',#4822,.T.);
#3303=FACE_OUTER_BOUND('',#4823,.T.);
#3304=FACE_OUTER_BOUND('',#4824,.T.);
#3305=FACE_OUTER_BOUND('',#4825,.T.);
#3306=FACE_OUTER_BOUND('',#4826,.T.);
#3307=FACE_OUTER_BOUND('',#4827,.T.);
#3308=FACE_OUTER_BOUND('',#4828,.T.);
#3309=FACE_OUTER_BOUND('',#4829,.T.);
#3310=FACE_OUTER_BOUND('',#4830,.T.);
#3311=FACE_OUTER_BOUND('',#4831,.T.);
#3312=FACE_OUTER_BOUND('',#4832,.T.);
#3313=FACE_OUTER_BOUND('',#4833,.T.);
#3314=FACE_OUTER_BOUND('',#4834,.T.);
#3315=FACE_OUTER_BOUND('',#4835,.T.);
#3316=FACE_OUTER_BOUND('',#4836,.T.);
#3317=FACE_OUTER_BOUND('',#4837,.T.);
#3318=FACE_OUTER_BOUND('',#4838,.T.);
#3319=FACE_OUTER_BOUND('',#4839,.T.);
#3320=FACE_OUTER_BOUND('',#4840,.T.);
#3321=FACE_OUTER_BOUND('',#4841,.T.);
#3322=FACE_OUTER_BOUND('',#4842,.T.);
#3323=FACE_OUTER_BOUND('',#4843,.T.);
#3324=FACE_OUTER_BOUND('',#4844,.T.);
#3325=FACE_OUTER_BOUND('',#4845,.T.);
#3326=FACE_OUTER_BOUND('',#4846,.T.);
#3327=FACE_OUTER_BOUND('',#4847,.T.);
#3328=FACE_OUTER_BOUND('',#4848,.T.);
#3329=FACE_OUTER_BOUND('',#4849,.T.);
#3330=FACE_OUTER_BOUND('',#4850,.T.);
#3331=FACE_OUTER_BOUND('',#4851,.T.);
#3332=FACE_OUTER_BOUND('',#4852,.T.);
#3333=FACE_OUTER_BOUND('',#4853,.T.);
#3334=FACE_OUTER_BOUND('',#4854,.T.);
#3335=FACE_OUTER_BOUND('',#4855,.T.);
#3336=FACE_OUTER_BOUND('',#4856,.T.);
#3337=FACE_OUTER_BOUND('',#4857,.T.);
#3338=FACE_OUTER_BOUND('',#4858,.T.);
#3339=FACE_OUTER_BOUND('',#4859,.T.);
#3340=FACE_OUTER_BOUND('',#4860,.T.);
#3341=FACE_OUTER_BOUND('',#4861,.T.);
#3342=FACE_OUTER_BOUND('',#4862,.T.);
#3343=FACE_OUTER_BOUND('',#4863,.T.);
#3344=FACE_OUTER_BOUND('',#4864,.T.);
#3345=FACE_OUTER_BOUND('',#4865,.T.);
#3346=FACE_OUTER_BOUND('',#4866,.T.);
#3347=FACE_OUTER_BOUND('',#4867,.T.);
#3348=FACE_OUTER_BOUND('',#4868,.T.);
#3349=FACE_OUTER_BOUND('',#4869,.T.);
#3350=FACE_OUTER_BOUND('',#4870,.T.);
#3351=FACE_OUTER_BOUND('',#4871,.T.);
#3352=FACE_OUTER_BOUND('',#4872,.T.);
#3353=FACE_OUTER_BOUND('',#4873,.T.);
#3354=FACE_OUTER_BOUND('',#4874,.T.);
#3355=FACE_OUTER_BOUND('',#4875,.T.);
#3356=FACE_OUTER_BOUND('',#4876,.T.);
#3357=FACE_OUTER_BOUND('',#4877,.T.);
#3358=FACE_OUTER_BOUND('',#4878,.T.);
#3359=FACE_OUTER_BOUND('',#4879,.T.);
#3360=FACE_OUTER_BOUND('',#4880,.T.);
#3361=FACE_OUTER_BOUND('',#4881,.T.);
#3362=FACE_OUTER_BOUND('',#4882,.T.);
#3363=FACE_OUTER_BOUND('',#4883,.T.);
#3364=FACE_OUTER_BOUND('',#4884,.T.);
#3365=FACE_OUTER_BOUND('',#4885,.T.);
#3366=FACE_OUTER_BOUND('',#4886,.T.);
#3367=FACE_OUTER_BOUND('',#4887,.T.);
#3368=FACE_OUTER_BOUND('',#4888,.T.);
#3369=FACE_OUTER_BOUND('',#4889,.T.);
#3370=FACE_OUTER_BOUND('',#4890,.T.);
#3371=FACE_OUTER_BOUND('',#4891,.T.);
#3372=FACE_OUTER_BOUND('',#4892,.T.);
#3373=FACE_OUTER_BOUND('',#4893,.T.);
#3374=FACE_OUTER_BOUND('',#4894,.T.);
#3375=FACE_OUTER_BOUND('',#4895,.T.);
#3376=FACE_OUTER_BOUND('',#4896,.T.);
#3377=FACE_OUTER_BOUND('',#4897,.T.);
#3378=FACE_OUTER_BOUND('',#4898,.T.);
#3379=FACE_OUTER_BOUND('',#4899,.T.);
#3380=FACE_OUTER_BOUND('',#4900,.T.);
#3381=FACE_OUTER_BOUND('',#4901,.T.);
#3382=FACE_OUTER_BOUND('',#4902,.T.);
#3383=FACE_OUTER_BOUND('',#4903,.T.);
#3384=FACE_OUTER_BOUND('',#4904,.T.);
#3385=FACE_OUTER_BOUND('',#4905,.T.);
#3386=FACE_OUTER_BOUND('',#4906,.T.);
#3387=FACE_OUTER_BOUND('',#4907,.T.);
#3388=FACE_OUTER_BOUND('',#4908,.T.);
#3389=FACE_OUTER_BOUND('',#4909,.T.);
#3390=FACE_OUTER_BOUND('',#4910,.T.);
#3391=FACE_OUTER_BOUND('',#4911,.T.);
#3392=FACE_OUTER_BOUND('',#4912,.T.);
#3393=FACE_OUTER_BOUND('',#4913,.T.);
#3394=FACE_OUTER_BOUND('',#4914,.T.);
#3395=FACE_OUTER_BOUND('',#4915,.T.);
#3396=FACE_OUTER_BOUND('',#4916,.T.);
#3397=FACE_OUTER_BOUND('',#4917,.T.);
#3398=FACE_OUTER_BOUND('',#4918,.T.);
#3399=FACE_OUTER_BOUND('',#4919,.T.);
#3400=FACE_OUTER_BOUND('',#4920,.T.);
#3401=FACE_OUTER_BOUND('',#4921,.T.);
#3402=FACE_OUTER_BOUND('',#4922,.T.);
#3403=FACE_OUTER_BOUND('',#4923,.T.);
#3404=FACE_OUTER_BOUND('',#4924,.T.);
#3405=FACE_OUTER_BOUND('',#4925,.T.);
#3406=FACE_OUTER_BOUND('',#4926,.T.);
#3407=FACE_OUTER_BOUND('',#4927,.T.);
#3408=FACE_OUTER_BOUND('',#4928,.T.);
#3409=FACE_OUTER_BOUND('',#4929,.T.);
#3410=FACE_OUTER_BOUND('',#4930,.T.);
#3411=FACE_OUTER_BOUND('',#4931,.T.);
#3412=FACE_OUTER_BOUND('',#4932,.T.);
#3413=FACE_OUTER_BOUND('',#4933,.T.);
#3414=FACE_OUTER_BOUND('',#4934,.T.);
#3415=FACE_OUTER_BOUND('',#4935,.T.);
#3416=FACE_OUTER_BOUND('',#4936,.T.);
#3417=FACE_OUTER_BOUND('',#4937,.T.);
#3418=FACE_OUTER_BOUND('',#4938,.T.);
#3419=FACE_OUTER_BOUND('',#4939,.T.);
#3420=FACE_OUTER_BOUND('',#4940,.T.);
#3421=FACE_OUTER_BOUND('',#4941,.T.);
#3422=FACE_OUTER_BOUND('',#4942,.T.);
#3423=FACE_OUTER_BOUND('',#4943,.T.);
#3424=FACE_OUTER_BOUND('',#4944,.T.);
#3425=FACE_OUTER_BOUND('',#4945,.T.);
#3426=FACE_OUTER_BOUND('',#4946,.T.);
#3427=FACE_OUTER_BOUND('',#4947,.T.);
#3428=FACE_OUTER_BOUND('',#4948,.T.);
#3429=FACE_OUTER_BOUND('',#4949,.T.);
#3430=FACE_OUTER_BOUND('',#4950,.T.);
#3431=FACE_OUTER_BOUND('',#4951,.T.);
#3432=FACE_OUTER_BOUND('',#4952,.T.);
#3433=FACE_OUTER_BOUND('',#4953,.T.);
#3434=FACE_OUTER_BOUND('',#4954,.T.);
#3435=FACE_OUTER_BOUND('',#4955,.T.);
#3436=FACE_OUTER_BOUND('',#4956,.T.);
#3437=FACE_OUTER_BOUND('',#4957,.T.);
#3438=FACE_OUTER_BOUND('',#4958,.T.);
#3439=FACE_OUTER_BOUND('',#4959,.T.);
#3440=FACE_OUTER_BOUND('',#4960,.T.);
#3441=FACE_OUTER_BOUND('',#4961,.T.);
#3442=FACE_OUTER_BOUND('',#4962,.T.);
#3443=FACE_OUTER_BOUND('',#4963,.T.);
#3444=FACE_OUTER_BOUND('',#4964,.T.);
#3445=FACE_OUTER_BOUND('',#4965,.T.);
#3446=FACE_OUTER_BOUND('',#4966,.T.);
#3447=FACE_OUTER_BOUND('',#4967,.T.);
#3448=FACE_OUTER_BOUND('',#4968,.T.);
#3449=FACE_OUTER_BOUND('',#4969,.T.);
#3450=FACE_OUTER_BOUND('',#4970,.T.);
#3451=FACE_OUTER_BOUND('',#4971,.T.);
#3452=FACE_OUTER_BOUND('',#4972,.T.);
#3453=FACE_OUTER_BOUND('',#4973,.T.);
#3454=FACE_OUTER_BOUND('',#4974,.T.);
#3455=FACE_OUTER_BOUND('',#4975,.T.);
#3456=FACE_OUTER_BOUND('',#4976,.T.);
#3457=FACE_OUTER_BOUND('',#4977,.T.);
#3458=FACE_OUTER_BOUND('',#4978,.T.);
#3459=FACE_OUTER_BOUND('',#4979,.T.);
#3460=FACE_OUTER_BOUND('',#4980,.T.);
#3461=FACE_OUTER_BOUND('',#4981,.T.);
#3462=FACE_OUTER_BOUND('',#4982,.T.);
#3463=FACE_OUTER_BOUND('',#4983,.T.);
#3464=FACE_OUTER_BOUND('',#4984,.T.);
#3465=FACE_OUTER_BOUND('',#4985,.T.);
#3466=FACE_OUTER_BOUND('',#4986,.T.);
#3467=FACE_OUTER_BOUND('',#4987,.T.);
#3468=FACE_OUTER_BOUND('',#4988,.T.);
#3469=FACE_OUTER_BOUND('',#4989,.T.);
#3470=FACE_OUTER_BOUND('',#4991,.T.);
#3471=FACE_OUTER_BOUND('',#4992,.T.);
#3472=FACE_OUTER_BOUND('',#4993,.T.);
#3473=FACE_OUTER_BOUND('',#4994,.T.);
#3474=FACE_OUTER_BOUND('',#4995,.T.);
#3475=FACE_OUTER_BOUND('',#4996,.T.);
#3476=FACE_OUTER_BOUND('',#4997,.T.);
#3477=FACE_OUTER_BOUND('',#4998,.T.);
#3478=FACE_OUTER_BOUND('',#4999,.T.);
#3479=FACE_OUTER_BOUND('',#5000,.T.);
#3480=FACE_OUTER_BOUND('',#5001,.T.);
#3481=FACE_OUTER_BOUND('',#5002,.T.);
#3482=FACE_OUTER_BOUND('',#5003,.T.);
#3483=FACE_OUTER_BOUND('',#5004,.T.);
#3484=FACE_OUTER_BOUND('',#5005,.T.);
#3485=FACE_OUTER_BOUND('',#5006,.T.);
#3486=FACE_OUTER_BOUND('',#5007,.T.);
#3487=FACE_OUTER_BOUND('',#5008,.T.);
#3488=FACE_OUTER_BOUND('',#5009,.T.);
#3489=FACE_OUTER_BOUND('',#5010,.T.);
#3490=FACE_OUTER_BOUND('',#5011,.T.);
#3491=FACE_OUTER_BOUND('',#5012,.T.);
#3492=FACE_OUTER_BOUND('',#5013,.T.);
#3493=FACE_OUTER_BOUND('',#5014,.T.);
#3494=FACE_OUTER_BOUND('',#5015,.T.);
#3495=FACE_OUTER_BOUND('',#5016,.T.);
#3496=FACE_OUTER_BOUND('',#5017,.T.);
#3497=FACE_OUTER_BOUND('',#5018,.T.);
#3498=FACE_OUTER_BOUND('',#5019,.T.);
#3499=FACE_OUTER_BOUND('',#5020,.T.);
#3500=FACE_OUTER_BOUND('',#5021,.T.);
#3501=FACE_OUTER_BOUND('',#5022,.T.);
#3502=FACE_OUTER_BOUND('',#5023,.T.);
#3503=FACE_OUTER_BOUND('',#5024,.T.);
#3504=FACE_OUTER_BOUND('',#5025,.T.);
#3505=FACE_OUTER_BOUND('',#5026,.T.);
#3506=FACE_OUTER_BOUND('',#5027,.T.);
#3507=FACE_OUTER_BOUND('',#5028,.T.);
#3508=FACE_OUTER_BOUND('',#5029,.T.);
#3509=FACE_OUTER_BOUND('',#5030,.T.);
#3510=FACE_OUTER_BOUND('',#5031,.T.);
#3511=FACE_OUTER_BOUND('',#5032,.T.);
#3512=FACE_OUTER_BOUND('',#5033,.T.);
#3513=FACE_OUTER_BOUND('',#5034,.T.);
#3514=FACE_OUTER_BOUND('',#5035,.T.);
#3515=FACE_OUTER_BOUND('',#5036,.T.);
#3516=FACE_OUTER_BOUND('',#5037,.T.);
#3517=FACE_OUTER_BOUND('',#5038,.T.);
#3518=FACE_OUTER_BOUND('',#5039,.T.);
#3519=FACE_OUTER_BOUND('',#5040,.T.);
#3520=FACE_OUTER_BOUND('',#5041,.T.);
#3521=FACE_OUTER_BOUND('',#5042,.T.);
#3522=FACE_OUTER_BOUND('',#5043,.T.);
#3523=FACE_OUTER_BOUND('',#5044,.T.);
#3524=FACE_OUTER_BOUND('',#5045,.T.);
#3525=FACE_OUTER_BOUND('',#5046,.T.);
#3526=FACE_OUTER_BOUND('',#5047,.T.);
#3527=FACE_OUTER_BOUND('',#5048,.T.);
#3528=FACE_OUTER_BOUND('',#5049,.T.);
#3529=FACE_OUTER_BOUND('',#5050,.T.);
#3530=FACE_OUTER_BOUND('',#5051,.T.);
#3531=FACE_OUTER_BOUND('',#5052,.T.);
#3532=FACE_OUTER_BOUND('',#5053,.T.);
#3533=FACE_OUTER_BOUND('',#5054,.T.);
#3534=FACE_OUTER_BOUND('',#5055,.T.);
#3535=FACE_OUTER_BOUND('',#5056,.T.);
#3536=FACE_OUTER_BOUND('',#5057,.T.);
#3537=FACE_OUTER_BOUND('',#5058,.T.);
#3538=FACE_OUTER_BOUND('',#5059,.T.);
#3539=FACE_OUTER_BOUND('',#5060,.T.);
#3540=FACE_OUTER_BOUND('',#5061,.T.);
#3541=FACE_OUTER_BOUND('',#5062,.T.);
#3542=FACE_OUTER_BOUND('',#5063,.T.);
#3543=FACE_OUTER_BOUND('',#5064,.T.);
#3544=FACE_OUTER_BOUND('',#5065,.T.);
#3545=FACE_OUTER_BOUND('',#5066,.T.);
#3546=FACE_OUTER_BOUND('',#5067,.T.);
#3547=FACE_OUTER_BOUND('',#5068,.T.);
#3548=FACE_OUTER_BOUND('',#5069,.T.);
#3549=FACE_OUTER_BOUND('',#5070,.T.);
#3550=FACE_OUTER_BOUND('',#5071,.T.);
#3551=FACE_OUTER_BOUND('',#5072,.T.);
#3552=FACE_OUTER_BOUND('',#5073,.T.);
#3553=FACE_OUTER_BOUND('',#5074,.T.);
#3554=FACE_OUTER_BOUND('',#5075,.T.);
#3555=FACE_OUTER_BOUND('',#5076,.T.);
#3556=FACE_OUTER_BOUND('',#5077,.T.);
#3557=FACE_OUTER_BOUND('',#5078,.T.);
#3558=FACE_OUTER_BOUND('',#5079,.T.);
#3559=FACE_OUTER_BOUND('',#5080,.T.);
#3560=FACE_OUTER_BOUND('',#5081,.T.);
#3561=FACE_OUTER_BOUND('',#5082,.T.);
#3562=FACE_OUTER_BOUND('',#5083,.T.);
#3563=FACE_OUTER_BOUND('',#5084,.T.);
#3564=FACE_OUTER_BOUND('',#5085,.T.);
#3565=FACE_OUTER_BOUND('',#5086,.T.);
#3566=FACE_OUTER_BOUND('',#5087,.T.);
#3567=FACE_OUTER_BOUND('',#5088,.T.);
#3568=FACE_OUTER_BOUND('',#5089,.T.);
#3569=FACE_OUTER_BOUND('',#5090,.T.);
#3570=FACE_OUTER_BOUND('',#5091,.T.);
#3571=FACE_OUTER_BOUND('',#5092,.T.);
#3572=FACE_OUTER_BOUND('',#5093,.T.);
#3573=FACE_OUTER_BOUND('',#5094,.T.);
#3574=FACE_OUTER_BOUND('',#5095,.T.);
#3575=FACE_OUTER_BOUND('',#5096,.T.);
#3576=FACE_OUTER_BOUND('',#5097,.T.);
#3577=FACE_OUTER_BOUND('',#5098,.T.);
#3578=FACE_OUTER_BOUND('',#5099,.T.);
#3579=FACE_OUTER_BOUND('',#5100,.T.);
#3580=FACE_OUTER_BOUND('',#5101,.T.);
#3581=FACE_OUTER_BOUND('',#5102,.T.);
#3582=FACE_OUTER_BOUND('',#5103,.T.);
#3583=FACE_OUTER_BOUND('',#5105,.T.);
#3584=FACE_OUTER_BOUND('',#5106,.T.);
#3585=FACE_OUTER_BOUND('',#5107,.T.);
#3586=FACE_OUTER_BOUND('',#5108,.T.);
#3587=FACE_OUTER_BOUND('',#5109,.T.);
#3588=FACE_OUTER_BOUND('',#5110,.T.);
#3589=FACE_OUTER_BOUND('',#5111,.T.);
#3590=FACE_OUTER_BOUND('',#5112,.T.);
#3591=FACE_OUTER_BOUND('',#5113,.T.);
#3592=FACE_OUTER_BOUND('',#5114,.T.);
#3593=FACE_OUTER_BOUND('',#5115,.T.);
#3594=FACE_OUTER_BOUND('',#5116,.T.);
#3595=FACE_OUTER_BOUND('',#5117,.T.);
#3596=FACE_OUTER_BOUND('',#5118,.T.);
#3597=FACE_OUTER_BOUND('',#5119,.T.);
#3598=FACE_OUTER_BOUND('',#5120,.T.);
#3599=FACE_OUTER_BOUND('',#5121,.T.);
#3600=FACE_OUTER_BOUND('',#5122,.T.);
#3601=FACE_OUTER_BOUND('',#5123,.T.);
#3602=FACE_OUTER_BOUND('',#5124,.T.);
#3603=FACE_OUTER_BOUND('',#5125,.T.);
#3604=FACE_OUTER_BOUND('',#5126,.T.);
#3605=FACE_OUTER_BOUND('',#5127,.T.);
#3606=FACE_OUTER_BOUND('',#5128,.T.);
#3607=FACE_OUTER_BOUND('',#5129,.T.);
#3608=FACE_OUTER_BOUND('',#5130,.T.);
#3609=FACE_OUTER_BOUND('',#5131,.T.);
#3610=FACE_OUTER_BOUND('',#5132,.T.);
#3611=FACE_OUTER_BOUND('',#5133,.T.);
#3612=FACE_OUTER_BOUND('',#5134,.T.);
#3613=FACE_OUTER_BOUND('',#5135,.T.);
#3614=FACE_OUTER_BOUND('',#5136,.T.);
#3615=FACE_OUTER_BOUND('',#5137,.T.);
#3616=FACE_OUTER_BOUND('',#5138,.T.);
#3617=FACE_OUTER_BOUND('',#5139,.T.);
#3618=FACE_OUTER_BOUND('',#5140,.T.);
#3619=FACE_OUTER_BOUND('',#5141,.T.);
#3620=FACE_OUTER_BOUND('',#5142,.T.);
#3621=FACE_OUTER_BOUND('',#5143,.T.);
#3622=FACE_OUTER_BOUND('',#5144,.T.);
#3623=FACE_OUTER_BOUND('',#5145,.T.);
#3624=FACE_OUTER_BOUND('',#5146,.T.);
#3625=FACE_OUTER_BOUND('',#5147,.T.);
#3626=FACE_OUTER_BOUND('',#5148,.T.);
#3627=FACE_OUTER_BOUND('',#5149,.T.);
#3628=FACE_OUTER_BOUND('',#5150,.T.);
#3629=FACE_OUTER_BOUND('',#5151,.T.);
#3630=FACE_OUTER_BOUND('',#5152,.T.);
#3631=FACE_OUTER_BOUND('',#5153,.T.);
#3632=FACE_OUTER_BOUND('',#5154,.T.);
#3633=FACE_OUTER_BOUND('',#5155,.T.);
#3634=FACE_OUTER_BOUND('',#5156,.T.);
#3635=FACE_OUTER_BOUND('',#5157,.T.);
#3636=FACE_OUTER_BOUND('',#5158,.T.);
#3637=FACE_OUTER_BOUND('',#5159,.T.);
#3638=FACE_OUTER_BOUND('',#5160,.T.);
#3639=FACE_OUTER_BOUND('',#5161,.T.);
#3640=FACE_OUTER_BOUND('',#5162,.T.);
#3641=FACE_OUTER_BOUND('',#5163,.T.);
#3642=FACE_OUTER_BOUND('',#5164,.T.);
#3643=FACE_OUTER_BOUND('',#5165,.T.);
#3644=FACE_OUTER_BOUND('',#5166,.T.);
#3645=FACE_OUTER_BOUND('',#5167,.T.);
#3646=FACE_OUTER_BOUND('',#5168,.T.);
#3647=FACE_OUTER_BOUND('',#5170,.T.);
#3648=FACE_OUTER_BOUND('',#5171,.T.);
#3649=FACE_OUTER_BOUND('',#5172,.T.);
#3650=FACE_OUTER_BOUND('',#5174,.T.);
#3651=FACE_OUTER_BOUND('',#5175,.T.);
#3652=FACE_OUTER_BOUND('',#5183,.T.);
#3653=FACE_OUTER_BOUND('',#5184,.T.);
#3654=FACE_OUTER_BOUND('',#5185,.T.);
#3655=FACE_OUTER_BOUND('',#5186,.T.);
#3656=FACE_OUTER_BOUND('',#5187,.T.);
#3657=FACE_OUTER_BOUND('',#5188,.T.);
#3658=FACE_OUTER_BOUND('',#5189,.T.);
#3659=FACE_OUTER_BOUND('',#5190,.T.);
#3660=FACE_OUTER_BOUND('',#5191,.T.);
#3661=FACE_OUTER_BOUND('',#5192,.T.);
#3662=FACE_OUTER_BOUND('',#5193,.T.);
#3663=FACE_OUTER_BOUND('',#5194,.T.);
#3664=FACE_OUTER_BOUND('',#5195,.T.);
#3665=FACE_OUTER_BOUND('',#5196,.T.);
#3666=FACE_OUTER_BOUND('',#5197,.T.);
#3667=FACE_OUTER_BOUND('',#5198,.T.);
#3668=FACE_OUTER_BOUND('',#5199,.T.);
#3669=FACE_OUTER_BOUND('',#5200,.T.);
#3670=FACE_OUTER_BOUND('',#5201,.T.);
#3671=FACE_OUTER_BOUND('',#5202,.T.);
#3672=FACE_OUTER_BOUND('',#5203,.T.);
#3673=FACE_OUTER_BOUND('',#5204,.T.);
#3674=FACE_OUTER_BOUND('',#5205,.T.);
#3675=FACE_OUTER_BOUND('',#5206,.T.);
#3676=FACE_OUTER_BOUND('',#5207,.T.);
#3677=FACE_OUTER_BOUND('',#5208,.T.);
#3678=FACE_OUTER_BOUND('',#5209,.T.);
#3679=FACE_OUTER_BOUND('',#5210,.T.);
#3680=FACE_OUTER_BOUND('',#5211,.T.);
#3681=FACE_OUTER_BOUND('',#5212,.T.);
#3682=FACE_OUTER_BOUND('',#5213,.T.);
#3683=FACE_OUTER_BOUND('',#5218,.T.);
#3684=FACE_OUTER_BOUND('',#5220,.T.);
#3685=FACE_OUTER_BOUND('',#5221,.T.);
#3686=FACE_OUTER_BOUND('',#5222,.T.);
#3687=FACE_OUTER_BOUND('',#5223,.T.);
#3688=FACE_OUTER_BOUND('',#5224,.T.);
#3689=FACE_OUTER_BOUND('',#5226,.T.);
#3690=FACE_OUTER_BOUND('',#5227,.T.);
#3691=FACE_OUTER_BOUND('',#5228,.T.);
#3692=FACE_OUTER_BOUND('',#5229,.T.);
#3693=FACE_OUTER_BOUND('',#5231,.T.);
#3694=FACE_OUTER_BOUND('',#5232,.T.);
#3695=FACE_OUTER_BOUND('',#5233,.T.);
#3696=FACE_OUTER_BOUND('',#5234,.T.);
#3697=FACE_OUTER_BOUND('',#5235,.T.);
#3698=FACE_OUTER_BOUND('',#5236,.T.);
#3699=FACE_OUTER_BOUND('',#5237,.T.);
#3700=FACE_OUTER_BOUND('',#5238,.T.);
#3701=FACE_OUTER_BOUND('',#5239,.T.);
#3702=FACE_OUTER_BOUND('',#5240,.T.);
#3703=FACE_OUTER_BOUND('',#5241,.T.);
#3704=FACE_OUTER_BOUND('',#5242,.T.);
#3705=FACE_OUTER_BOUND('',#5243,.T.);
#3706=FACE_OUTER_BOUND('',#5244,.T.);
#3707=FACE_OUTER_BOUND('',#5245,.T.);
#3708=FACE_OUTER_BOUND('',#5246,.T.);
#3709=FACE_OUTER_BOUND('',#5247,.T.);
#3710=FACE_OUTER_BOUND('',#5248,.T.);
#3711=FACE_OUTER_BOUND('',#5249,.T.);
#3712=FACE_OUTER_BOUND('',#5250,.T.);
#3713=FACE_OUTER_BOUND('',#5251,.T.);
#3714=FACE_OUTER_BOUND('',#5253,.T.);
#3715=FACE_OUTER_BOUND('',#5254,.T.);
#3716=FACE_OUTER_BOUND('',#5255,.T.);
#3717=FACE_OUTER_BOUND('',#5256,.T.);
#3718=FACE_OUTER_BOUND('',#5257,.T.);
#3719=FACE_OUTER_BOUND('',#5258,.T.);
#3720=FACE_OUTER_BOUND('',#5259,.T.);
#3721=FACE_OUTER_BOUND('',#5260,.T.);
#3722=FACE_OUTER_BOUND('',#5261,.T.);
#3723=FACE_OUTER_BOUND('',#5262,.T.);
#3724=FACE_OUTER_BOUND('',#5266,.T.);
#3725=FACE_OUTER_BOUND('',#5267,.T.);
#3726=FACE_OUTER_BOUND('',#5268,.T.);
#3727=FACE_OUTER_BOUND('',#5269,.T.);
#3728=FACE_OUTER_BOUND('',#5270,.T.);
#3729=FACE_OUTER_BOUND('',#5271,.T.);
#3730=FACE_OUTER_BOUND('',#5272,.T.);
#3731=FACE_OUTER_BOUND('',#5273,.T.);
#3732=FACE_OUTER_BOUND('',#5274,.T.);
#3733=FACE_OUTER_BOUND('',#5275,.T.);
#3734=FACE_OUTER_BOUND('',#5280,.T.);
#3735=FACE_OUTER_BOUND('',#5281,.T.);
#3736=FACE_OUTER_BOUND('',#5282,.T.);
#3737=FACE_OUTER_BOUND('',#5283,.T.);
#3738=FACE_OUTER_BOUND('',#5284,.T.);
#3739=FACE_OUTER_BOUND('',#5285,.T.);
#3740=FACE_OUTER_BOUND('',#5286,.T.);
#3741=FACE_OUTER_BOUND('',#5287,.T.);
#3742=FACE_OUTER_BOUND('',#5288,.T.);
#3743=FACE_OUTER_BOUND('',#5289,.T.);
#3744=FACE_OUTER_BOUND('',#5296,.T.);
#3745=FACE_OUTER_BOUND('',#5297,.T.);
#3746=FACE_OUTER_BOUND('',#5298,.T.);
#3747=FACE_OUTER_BOUND('',#5299,.T.);
#3748=FACE_OUTER_BOUND('',#5300,.T.);
#3749=FACE_OUTER_BOUND('',#5301,.T.);
#3750=FACE_OUTER_BOUND('',#5302,.T.);
#3751=FACE_OUTER_BOUND('',#5303,.T.);
#3752=FACE_OUTER_BOUND('',#5304,.T.);
#3753=FACE_OUTER_BOUND('',#5305,.T.);
#3754=FACE_OUTER_BOUND('',#5306,.T.);
#3755=FACE_OUTER_BOUND('',#5307,.T.);
#3756=FACE_OUTER_BOUND('',#5308,.T.);
#3757=FACE_OUTER_BOUND('',#5309,.T.);
#3758=FACE_OUTER_BOUND('',#5310,.T.);
#3759=FACE_OUTER_BOUND('',#5311,.T.);
#3760=FACE_OUTER_BOUND('',#5312,.T.);
#3761=FACE_OUTER_BOUND('',#5313,.T.);
#3762=FACE_OUTER_BOUND('',#5314,.T.);
#3763=FACE_OUTER_BOUND('',#5315,.T.);
#3764=FACE_OUTER_BOUND('',#5316,.T.);
#3765=FACE_OUTER_BOUND('',#5317,.T.);
#3766=FACE_OUTER_BOUND('',#5323,.T.);
#3767=FACE_OUTER_BOUND('',#5324,.T.);
#3768=FACE_OUTER_BOUND('',#5325,.T.);
#3769=FACE_OUTER_BOUND('',#5326,.T.);
#3770=FACE_OUTER_BOUND('',#5327,.T.);
#3771=FACE_OUTER_BOUND('',#5328,.T.);
#3772=FACE_OUTER_BOUND('',#5329,.T.);
#3773=FACE_OUTER_BOUND('',#5331,.T.);
#3774=FACE_OUTER_BOUND('',#5332,.T.);
#3775=FACE_OUTER_BOUND('',#5333,.T.);
#3776=FACE_OUTER_BOUND('',#5334,.T.);
#3777=FACE_OUTER_BOUND('',#5335,.T.);
#3778=FACE_OUTER_BOUND('',#5336,.T.);
#3779=FACE_OUTER_BOUND('',#5337,.T.);
#3780=FACE_OUTER_BOUND('',#5338,.T.);
#3781=FACE_OUTER_BOUND('',#5339,.T.);
#3782=FACE_OUTER_BOUND('',#5340,.T.);
#3783=FACE_OUTER_BOUND('',#5341,.T.);
#3784=FACE_OUTER_BOUND('',#5342,.T.);
#3785=FACE_OUTER_BOUND('',#5343,.T.);
#3786=FACE_OUTER_BOUND('',#5344,.T.);
#3787=FACE_OUTER_BOUND('',#5345,.T.);
#3788=FACE_OUTER_BOUND('',#5346,.T.);
#3789=FACE_OUTER_BOUND('',#5347,.T.);
#3790=FACE_OUTER_BOUND('',#5348,.T.);
#3791=FACE_OUTER_BOUND('',#5349,.T.);
#3792=FACE_OUTER_BOUND('',#5350,.T.);
#3793=FACE_OUTER_BOUND('',#5351,.T.);
#3794=FACE_OUTER_BOUND('',#5352,.T.);
#3795=FACE_OUTER_BOUND('',#5353,.T.);
#3796=FACE_OUTER_BOUND('',#5354,.T.);
#3797=FACE_OUTER_BOUND('',#5355,.T.);
#3798=FACE_OUTER_BOUND('',#5356,.T.);
#3799=FACE_OUTER_BOUND('',#5357,.T.);
#3800=FACE_OUTER_BOUND('',#5358,.T.);
#3801=FACE_OUTER_BOUND('',#5359,.T.);
#3802=FACE_OUTER_BOUND('',#5360,.T.);
#3803=FACE_OUTER_BOUND('',#5361,.T.);
#3804=FACE_OUTER_BOUND('',#5362,.T.);
#3805=FACE_OUTER_BOUND('',#5363,.T.);
#3806=FACE_OUTER_BOUND('',#5364,.T.);
#3807=FACE_OUTER_BOUND('',#5365,.T.);
#3808=FACE_OUTER_BOUND('',#5366,.T.);
#3809=FACE_OUTER_BOUND('',#5367,.T.);
#3810=FACE_OUTER_BOUND('',#5368,.T.);
#3811=FACE_OUTER_BOUND('',#5369,.T.);
#3812=FACE_OUTER_BOUND('',#5370,.T.);
#3813=FACE_OUTER_BOUND('',#5371,.T.);
#3814=FACE_OUTER_BOUND('',#5372,.T.);
#3815=FACE_OUTER_BOUND('',#5373,.T.);
#3816=FACE_OUTER_BOUND('',#5374,.T.);
#3817=FACE_OUTER_BOUND('',#5375,.T.);
#3818=FACE_OUTER_BOUND('',#5376,.T.);
#3819=FACE_OUTER_BOUND('',#5377,.T.);
#3820=FACE_OUTER_BOUND('',#5378,.T.);
#3821=FACE_OUTER_BOUND('',#5379,.T.);
#3822=FACE_OUTER_BOUND('',#5380,.T.);
#3823=FACE_OUTER_BOUND('',#5381,.T.);
#3824=FACE_OUTER_BOUND('',#5382,.T.);
#3825=FACE_OUTER_BOUND('',#5383,.T.);
#3826=FACE_OUTER_BOUND('',#5384,.T.);
#3827=FACE_OUTER_BOUND('',#5385,.T.);
#3828=FACE_OUTER_BOUND('',#5386,.T.);
#3829=FACE_OUTER_BOUND('',#5387,.T.);
#3830=FACE_OUTER_BOUND('',#5388,.T.);
#3831=FACE_OUTER_BOUND('',#5389,.T.);
#3832=FACE_OUTER_BOUND('',#5390,.T.);
#3833=FACE_OUTER_BOUND('',#5391,.T.);
#3834=FACE_OUTER_BOUND('',#5392,.T.);
#3835=FACE_OUTER_BOUND('',#5393,.T.);
#3836=FACE_OUTER_BOUND('',#5394,.T.);
#3837=FACE_OUTER_BOUND('',#5395,.T.);
#3838=FACE_OUTER_BOUND('',#5396,.T.);
#3839=FACE_OUTER_BOUND('',#5397,.T.);
#3840=FACE_OUTER_BOUND('',#5398,.T.);
#3841=FACE_OUTER_BOUND('',#5399,.T.);
#3842=FACE_OUTER_BOUND('',#5400,.T.);
#3843=FACE_OUTER_BOUND('',#5401,.T.);
#3844=FACE_OUTER_BOUND('',#5402,.T.);
#3845=FACE_OUTER_BOUND('',#5403,.T.);
#3846=FACE_OUTER_BOUND('',#5404,.T.);
#3847=FACE_OUTER_BOUND('',#5405,.T.);
#3848=FACE_OUTER_BOUND('',#5406,.T.);
#3849=FACE_OUTER_BOUND('',#5407,.T.);
#3850=FACE_OUTER_BOUND('',#5408,.T.);
#3851=FACE_OUTER_BOUND('',#5409,.T.);
#3852=FACE_OUTER_BOUND('',#5410,.T.);
#3853=FACE_OUTER_BOUND('',#5411,.T.);
#3854=FACE_OUTER_BOUND('',#5412,.T.);
#3855=FACE_OUTER_BOUND('',#5413,.T.);
#3856=FACE_OUTER_BOUND('',#5414,.T.);
#3857=FACE_OUTER_BOUND('',#5415,.T.);
#3858=FACE_OUTER_BOUND('',#5416,.T.);
#3859=FACE_OUTER_BOUND('',#5417,.T.);
#3860=FACE_OUTER_BOUND('',#5419,.T.);
#3861=FACE_OUTER_BOUND('',#5420,.T.);
#3862=FACE_OUTER_BOUND('',#5421,.T.);
#3863=FACE_OUTER_BOUND('',#5422,.T.);
#3864=FACE_OUTER_BOUND('',#5423,.T.);
#3865=FACE_OUTER_BOUND('',#5424,.T.);
#3866=FACE_OUTER_BOUND('',#5426,.T.);
#3867=FACE_OUTER_BOUND('',#5427,.T.);
#3868=FACE_OUTER_BOUND('',#5429,.T.);
#3869=FACE_OUTER_BOUND('',#5430,.T.);
#3870=FACE_OUTER_BOUND('',#5431,.T.);
#3871=FACE_OUTER_BOUND('',#5432,.T.);
#3872=FACE_OUTER_BOUND('',#5433,.T.);
#3873=FACE_OUTER_BOUND('',#5434,.T.);
#3874=FACE_OUTER_BOUND('',#5435,.T.);
#3875=FACE_OUTER_BOUND('',#5436,.T.);
#3876=FACE_OUTER_BOUND('',#5437,.T.);
#3877=FACE_OUTER_BOUND('',#5438,.T.);
#3878=FACE_OUTER_BOUND('',#5439,.T.);
#3879=FACE_OUTER_BOUND('',#5440,.T.);
#3880=FACE_OUTER_BOUND('',#5441,.T.);
#3881=FACE_OUTER_BOUND('',#5442,.T.);
#3882=FACE_OUTER_BOUND('',#5443,.T.);
#3883=FACE_OUTER_BOUND('',#5444,.T.);
#3884=FACE_OUTER_BOUND('',#5445,.T.);
#3885=FACE_OUTER_BOUND('',#5447,.T.);
#3886=FACE_OUTER_BOUND('',#5448,.T.);
#3887=FACE_OUTER_BOUND('',#5450,.T.);
#3888=FACE_OUTER_BOUND('',#5451,.T.);
#3889=FACE_OUTER_BOUND('',#5452,.T.);
#3890=FACE_OUTER_BOUND('',#5453,.T.);
#3891=FACE_OUTER_BOUND('',#5454,.T.);
#3892=FACE_OUTER_BOUND('',#5455,.T.);
#3893=FACE_OUTER_BOUND('',#5456,.T.);
#3894=FACE_OUTER_BOUND('',#5457,.T.);
#3895=FACE_OUTER_BOUND('',#5458,.T.);
#3896=FACE_OUTER_BOUND('',#5459,.T.);
#3897=FACE_OUTER_BOUND('',#5460,.T.);
#3898=FACE_OUTER_BOUND('',#5461,.T.);
#3899=FACE_OUTER_BOUND('',#5462,.T.);
#3900=FACE_OUTER_BOUND('',#5463,.T.);
#3901=FACE_OUTER_BOUND('',#5464,.T.);
#3902=FACE_OUTER_BOUND('',#5465,.T.);
#3903=FACE_OUTER_BOUND('',#5466,.T.);
#3904=FACE_OUTER_BOUND('',#5467,.T.);
#3905=FACE_OUTER_BOUND('',#5468,.T.);
#3906=FACE_OUTER_BOUND('',#5469,.T.);
#3907=FACE_OUTER_BOUND('',#5470,.T.);
#3908=FACE_OUTER_BOUND('',#5471,.T.);
#3909=FACE_OUTER_BOUND('',#5472,.T.);
#3910=FACE_OUTER_BOUND('',#5473,.T.);
#3911=FACE_OUTER_BOUND('',#5474,.T.);
#3912=FACE_OUTER_BOUND('',#5475,.T.);
#3913=FACE_OUTER_BOUND('',#5476,.T.);
#3914=FACE_OUTER_BOUND('',#5477,.T.);
#3915=FACE_OUTER_BOUND('',#5478,.T.);
#3916=FACE_OUTER_BOUND('',#5479,.T.);
#3917=FACE_OUTER_BOUND('',#5480,.T.);
#3918=FACE_OUTER_BOUND('',#5481,.T.);
#3919=FACE_OUTER_BOUND('',#5482,.T.);
#3920=FACE_OUTER_BOUND('',#5483,.T.);
#3921=FACE_OUTER_BOUND('',#5484,.T.);
#3922=FACE_OUTER_BOUND('',#5485,.T.);
#3923=FACE_OUTER_BOUND('',#5486,.T.);
#3924=FACE_OUTER_BOUND('',#5487,.T.);
#3925=FACE_OUTER_BOUND('',#5488,.T.);
#3926=FACE_OUTER_BOUND('',#5489,.T.);
#3927=FACE_OUTER_BOUND('',#5490,.T.);
#3928=FACE_OUTER_BOUND('',#5491,.T.);
#3929=FACE_OUTER_BOUND('',#5492,.T.);
#3930=FACE_OUTER_BOUND('',#5493,.T.);
#3931=FACE_OUTER_BOUND('',#5494,.T.);
#3932=FACE_OUTER_BOUND('',#5495,.T.);
#3933=FACE_OUTER_BOUND('',#5496,.T.);
#3934=FACE_OUTER_BOUND('',#5497,.T.);
#3935=FACE_OUTER_BOUND('',#5498,.T.);
#3936=FACE_OUTER_BOUND('',#5499,.T.);
#3937=FACE_OUTER_BOUND('',#5500,.T.);
#3938=FACE_OUTER_BOUND('',#5501,.T.);
#3939=FACE_OUTER_BOUND('',#5502,.T.);
#3940=FACE_OUTER_BOUND('',#5503,.T.);
#3941=FACE_OUTER_BOUND('',#5504,.T.);
#3942=FACE_OUTER_BOUND('',#5505,.T.);
#3943=FACE_OUTER_BOUND('',#5506,.T.);
#3944=FACE_OUTER_BOUND('',#5507,.T.);
#3945=FACE_OUTER_BOUND('',#5508,.T.);
#3946=FACE_OUTER_BOUND('',#5509,.T.);
#3947=FACE_OUTER_BOUND('',#5510,.T.);
#3948=FACE_OUTER_BOUND('',#5511,.T.);
#3949=FACE_OUTER_BOUND('',#5512,.T.);
#3950=FACE_OUTER_BOUND('',#5513,.T.);
#3951=FACE_OUTER_BOUND('',#5514,.T.);
#3952=FACE_OUTER_BOUND('',#5515,.T.);
#3953=FACE_OUTER_BOUND('',#5516,.T.);
#3954=FACE_OUTER_BOUND('',#5517,.T.);
#3955=FACE_OUTER_BOUND('',#5518,.T.);
#3956=FACE_OUTER_BOUND('',#5519,.T.);
#3957=FACE_OUTER_BOUND('',#5520,.T.);
#3958=FACE_OUTER_BOUND('',#5521,.T.);
#3959=FACE_OUTER_BOUND('',#5522,.T.);
#3960=FACE_OUTER_BOUND('',#5523,.T.);
#3961=FACE_OUTER_BOUND('',#5524,.T.);
#3962=FACE_OUTER_BOUND('',#5525,.T.);
#3963=FACE_OUTER_BOUND('',#5526,.T.);
#3964=FACE_OUTER_BOUND('',#5527,.T.);
#3965=FACE_OUTER_BOUND('',#5528,.T.);
#3966=FACE_OUTER_BOUND('',#5529,.T.);
#3967=FACE_OUTER_BOUND('',#5530,.T.);
#3968=FACE_OUTER_BOUND('',#5531,.T.);
#3969=FACE_OUTER_BOUND('',#5532,.T.);
#3970=FACE_OUTER_BOUND('',#5533,.T.);
#3971=FACE_OUTER_BOUND('',#5534,.T.);
#3972=FACE_OUTER_BOUND('',#5535,.T.);
#3973=FACE_OUTER_BOUND('',#5536,.T.);
#3974=FACE_OUTER_BOUND('',#5537,.T.);
#3975=FACE_OUTER_BOUND('',#5538,.T.);
#3976=FACE_OUTER_BOUND('',#5539,.T.);
#3977=FACE_OUTER_BOUND('',#5540,.T.);
#3978=FACE_OUTER_BOUND('',#5541,.T.);
#3979=FACE_OUTER_BOUND('',#5542,.T.);
#3980=FACE_OUTER_BOUND('',#5543,.T.);
#3981=FACE_OUTER_BOUND('',#5544,.T.);
#3982=FACE_OUTER_BOUND('',#5545,.T.);
#3983=FACE_OUTER_BOUND('',#5546,.T.);
#3984=FACE_OUTER_BOUND('',#5547,.T.);
#3985=FACE_OUTER_BOUND('',#5548,.T.);
#3986=FACE_OUTER_BOUND('',#5549,.T.);
#3987=FACE_OUTER_BOUND('',#5550,.T.);
#3988=FACE_OUTER_BOUND('',#5551,.T.);
#3989=FACE_OUTER_BOUND('',#5552,.T.);
#3990=FACE_OUTER_BOUND('',#5553,.T.);
#3991=FACE_OUTER_BOUND('',#5554,.T.);
#3992=FACE_OUTER_BOUND('',#5555,.T.);
#3993=FACE_OUTER_BOUND('',#5556,.T.);
#3994=FACE_OUTER_BOUND('',#5557,.T.);
#3995=FACE_OUTER_BOUND('',#5558,.T.);
#3996=FACE_OUTER_BOUND('',#5559,.T.);
#3997=FACE_OUTER_BOUND('',#5560,.T.);
#3998=FACE_OUTER_BOUND('',#5563,.T.);
#3999=FACE_OUTER_BOUND('',#5564,.T.);
#4000=FACE_OUTER_BOUND('',#5565,.T.);
#4001=FACE_OUTER_BOUND('',#5566,.T.);
#4002=FACE_OUTER_BOUND('',#5567,.T.);
#4003=FACE_OUTER_BOUND('',#5568,.T.);
#4004=FACE_OUTER_BOUND('',#5569,.T.);
#4005=FACE_OUTER_BOUND('',#5570,.T.);
#4006=FACE_OUTER_BOUND('',#5571,.T.);
#4007=FACE_OUTER_BOUND('',#5572,.T.);
#4008=FACE_OUTER_BOUND('',#5573,.T.);
#4009=FACE_OUTER_BOUND('',#5574,.T.);
#4010=FACE_OUTER_BOUND('',#5575,.T.);
#4011=FACE_OUTER_BOUND('',#5576,.T.);
#4012=FACE_OUTER_BOUND('',#5577,.T.);
#4013=FACE_OUTER_BOUND('',#5578,.T.);
#4014=FACE_OUTER_BOUND('',#5579,.T.);
#4015=FACE_OUTER_BOUND('',#5580,.T.);
#4016=FACE_OUTER_BOUND('',#5581,.T.);
#4017=FACE_OUTER_BOUND('',#5582,.T.);
#4018=FACE_OUTER_BOUND('',#5583,.T.);
#4019=FACE_OUTER_BOUND('',#5584,.T.);
#4020=FACE_OUTER_BOUND('',#5585,.T.);
#4021=FACE_OUTER_BOUND('',#5586,.T.);
#4022=FACE_OUTER_BOUND('',#5587,.T.);
#4023=FACE_OUTER_BOUND('',#5588,.T.);
#4024=FACE_OUTER_BOUND('',#5589,.T.);
#4025=FACE_OUTER_BOUND('',#5590,.T.);
#4026=FACE_OUTER_BOUND('',#5591,.T.);
#4027=FACE_OUTER_BOUND('',#5592,.T.);
#4028=FACE_OUTER_BOUND('',#5593,.T.);
#4029=FACE_OUTER_BOUND('',#5594,.T.);
#4030=FACE_OUTER_BOUND('',#5595,.T.);
#4031=FACE_OUTER_BOUND('',#5596,.T.);
#4032=FACE_OUTER_BOUND('',#5597,.T.);
#4033=FACE_OUTER_BOUND('',#5598,.T.);
#4034=FACE_OUTER_BOUND('',#5599,.T.);
#4035=FACE_OUTER_BOUND('',#5600,.T.);
#4036=FACE_OUTER_BOUND('',#5601,.T.);
#4037=FACE_OUTER_BOUND('',#5604,.T.);
#4038=FACE_OUTER_BOUND('',#5605,.T.);
#4039=FACE_OUTER_BOUND('',#5606,.T.);
#4040=FACE_OUTER_BOUND('',#5607,.T.);
#4041=FACE_OUTER_BOUND('',#5608,.T.);
#4042=FACE_OUTER_BOUND('',#5609,.T.);
#4043=FACE_OUTER_BOUND('',#5610,.T.);
#4044=FACE_OUTER_BOUND('',#5611,.T.);
#4045=FACE_OUTER_BOUND('',#5612,.T.);
#4046=FACE_OUTER_BOUND('',#5613,.T.);
#4047=FACE_OUTER_BOUND('',#5614,.T.);
#4048=FACE_OUTER_BOUND('',#5616,.T.);
#4049=FACE_OUTER_BOUND('',#5617,.T.);
#4050=FACE_OUTER_BOUND('',#5618,.T.);
#4051=FACE_OUTER_BOUND('',#5619,.T.);
#4052=FACE_OUTER_BOUND('',#5620,.T.);
#4053=FACE_OUTER_BOUND('',#5621,.T.);
#4054=FACE_OUTER_BOUND('',#5622,.T.);
#4055=FACE_OUTER_BOUND('',#5623,.T.);
#4056=FACE_OUTER_BOUND('',#5624,.T.);
#4057=FACE_OUTER_BOUND('',#5628,.T.);
#4058=FACE_OUTER_BOUND('',#5629,.T.);
#4059=EDGE_LOOP('',(#17498,#17499,#17500,#17501,#17502));
#4060=EDGE_LOOP('',(#17503));
#4061=EDGE_LOOP('',(#17504,#17505,#17506,#17507,#17508,#17509,#17510,#17511,
#17512,#17513,#17514,#17515,#17516,#17517,#17518,#17519,#17520,#17521,#17522,
#17523,#17524,#17525,#17526,#17527,#17528,#17529,#17530,#17531,#17532,#17533,
#17534,#17535,#17536,#17537,#17538,#17539,#17540,#17541,#17542,#17543,#17544,
#17545,#17546,#17547,#17548,#17549,#17550,#17551,#17552,#17553,#17554,#17555,
#17556,#17557,#17558,#17559,#17560,#17561,#17562,#17563,#17564,#17565,#17566,
#17567,#17568,#17569,#17570,#17571,#17572,#17573,#17574,#17575,#17576,#17577,
#17578,#17579,#17580,#17581,#17582,#17583,#17584,#17585,#17586,#17587,#17588,
#17589,#17590,#17591,#17592,#17593,#17594,#17595,#17596,#17597,#17598,#17599,
#17600,#17601,#17602,#17603,#17604,#17605,#17606,#17607,#17608,#17609,#17610,
#17611));
#4062=EDGE_LOOP('',(#17612,#17613,#17614,#17615,#17616));
#4063=EDGE_LOOP('',(#17617,#17618,#17619,#17620,#17621));
#4064=EDGE_LOOP('',(#17622));
#4065=EDGE_LOOP('',(#17623,#17624,#17625,#17626,#17627,#17628,#17629,#17630,
#17631,#17632,#17633,#17634,#17635,#17636,#17637,#17638,#17639,#17640,#17641,
#17642,#17643,#17644,#17645,#17646,#17647,#17648,#17649,#17650,#17651,#17652,
#17653,#17654,#17655,#17656,#17657,#17658,#17659,#17660,#17661,#17662,#17663,
#17664,#17665,#17666,#17667,#17668,#17669,#17670,#17671,#17672,#17673,#17674,
#17675,#17676,#17677,#17678,#17679,#17680,#17681,#17682,#17683,#17684,#17685,
#17686,#17687,#17688,#17689,#17690,#17691,#17692,#17693,#17694,#17695,#17696,
#17697,#17698,#17699,#17700,#17701,#17702,#17703,#17704,#17705,#17706,#17707,
#17708,#17709,#17710,#17711,#17712,#17713,#17714,#17715,#17716,#17717,#17718,
#17719,#17720,#17721,#17722,#17723,#17724,#17725,#17726,#17727,#17728,#17729,
#17730));
#4066=EDGE_LOOP('',(#17731,#17732,#17733,#17734,#17735));
#4067=EDGE_LOOP('',(#17736));
#4068=EDGE_LOOP('',(#17737,#17738,#17739,#17740));
#4069=EDGE_LOOP('',(#17741,#17742,#17743,#17744));
#4070=EDGE_LOOP('',(#17745));
#4071=EDGE_LOOP('',(#17746));
#4072=EDGE_LOOP('',(#17747,#17748,#17749,#17750));
#4073=EDGE_LOOP('',(#17751,#17752,#17753,#17754));
#4074=EDGE_LOOP('',(#17755));
#4075=EDGE_LOOP('',(#17756));
#4076=EDGE_LOOP('',(#17757,#17758,#17759,#17760));
#4077=EDGE_LOOP('',(#17761,#17762,#17763,#17764));
#4078=EDGE_LOOP('',(#17765));
#4079=EDGE_LOOP('',(#17766,#17767,#17768,#17769));
#4080=EDGE_LOOP('',(#17770,#17771,#17772,#17773));
#4081=EDGE_LOOP('',(#17774,#17775,#17776,#17777));
#4082=EDGE_LOOP('',(#17778,#17779,#17780,#17781));
#4083=EDGE_LOOP('',(#17782,#17783,#17784,#17785));
#4084=EDGE_LOOP('',(#17786,#17787,#17788,#17789));
#4085=EDGE_LOOP('',(#17790,#17791,#17792,#17793));
#4086=EDGE_LOOP('',(#17794,#17795,#17796,#17797));
#4087=EDGE_LOOP('',(#17798,#17799,#17800,#17801));
#4088=EDGE_LOOP('',(#17802,#17803,#17804,#17805));
#4089=EDGE_LOOP('',(#17806,#17807,#17808,#17809));
#4090=EDGE_LOOP('',(#17810,#17811,#17812,#17813));
#4091=EDGE_LOOP('',(#17814,#17815,#17816,#17817));
#4092=EDGE_LOOP('',(#17818,#17819,#17820,#17821));
#4093=EDGE_LOOP('',(#17822,#17823,#17824,#17825));
#4094=EDGE_LOOP('',(#17826,#17827,#17828,#17829));
#4095=EDGE_LOOP('',(#17830,#17831,#17832,#17833));
#4096=EDGE_LOOP('',(#17834,#17835,#17836,#17837));
#4097=EDGE_LOOP('',(#17838,#17839,#17840,#17841));
#4098=EDGE_LOOP('',(#17842,#17843,#17844,#17845));
#4099=EDGE_LOOP('',(#17846,#17847,#17848,#17849));
#4100=EDGE_LOOP('',(#17850,#17851,#17852,#17853));
#4101=EDGE_LOOP('',(#17854,#17855,#17856,#17857));
#4102=EDGE_LOOP('',(#17858,#17859,#17860,#17861));
#4103=EDGE_LOOP('',(#17862,#17863,#17864,#17865));
#4104=EDGE_LOOP('',(#17866,#17867,#17868,#17869));
#4105=EDGE_LOOP('',(#17870,#17871,#17872,#17873));
#4106=EDGE_LOOP('',(#17874,#17875,#17876,#17877));
#4107=EDGE_LOOP('',(#17878,#17879,#17880,#17881));
#4108=EDGE_LOOP('',(#17882,#17883,#17884,#17885));
#4109=EDGE_LOOP('',(#17886,#17887,#17888,#17889));
#4110=EDGE_LOOP('',(#17890,#17891,#17892,#17893));
#4111=EDGE_LOOP('',(#17894,#17895,#17896,#17897));
#4112=EDGE_LOOP('',(#17898,#17899,#17900,#17901));
#4113=EDGE_LOOP('',(#17902,#17903,#17904,#17905));
#4114=EDGE_LOOP('',(#17906,#17907,#17908,#17909));
#4115=EDGE_LOOP('',(#17910,#17911,#17912,#17913));
#4116=EDGE_LOOP('',(#17914,#17915,#17916,#17917));
#4117=EDGE_LOOP('',(#17918,#17919,#17920,#17921));
#4118=EDGE_LOOP('',(#17922,#17923,#17924,#17925));
#4119=EDGE_LOOP('',(#17926,#17927,#17928,#17929));
#4120=EDGE_LOOP('',(#17930,#17931,#17932,#17933));
#4121=EDGE_LOOP('',(#17934,#17935,#17936,#17937));
#4122=EDGE_LOOP('',(#17938,#17939,#17940,#17941));
#4123=EDGE_LOOP('',(#17942,#17943,#17944,#17945));
#4124=EDGE_LOOP('',(#17946,#17947,#17948,#17949));
#4125=EDGE_LOOP('',(#17950,#17951,#17952,#17953));
#4126=EDGE_LOOP('',(#17954,#17955,#17956,#17957));
#4127=EDGE_LOOP('',(#17958,#17959,#17960,#17961));
#4128=EDGE_LOOP('',(#17962,#17963,#17964,#17965));
#4129=EDGE_LOOP('',(#17966,#17967,#17968,#17969));
#4130=EDGE_LOOP('',(#17970,#17971,#17972,#17973));
#4131=EDGE_LOOP('',(#17974,#17975,#17976,#17977));
#4132=EDGE_LOOP('',(#17978,#17979,#17980,#17981));
#4133=EDGE_LOOP('',(#17982,#17983,#17984,#17985));
#4134=EDGE_LOOP('',(#17986,#17987,#17988,#17989));
#4135=EDGE_LOOP('',(#17990,#17991,#17992,#17993));
#4136=EDGE_LOOP('',(#17994,#17995,#17996,#17997));
#4137=EDGE_LOOP('',(#17998,#17999,#18000,#18001));
#4138=EDGE_LOOP('',(#18002,#18003,#18004,#18005));
#4139=EDGE_LOOP('',(#18006,#18007,#18008,#18009));
#4140=EDGE_LOOP('',(#18010,#18011,#18012,#18013));
#4141=EDGE_LOOP('',(#18014,#18015,#18016,#18017));
#4142=EDGE_LOOP('',(#18018,#18019,#18020,#18021));
#4143=EDGE_LOOP('',(#18022,#18023,#18024,#18025));
#4144=EDGE_LOOP('',(#18026,#18027,#18028,#18029));
#4145=EDGE_LOOP('',(#18030,#18031,#18032,#18033));
#4146=EDGE_LOOP('',(#18034,#18035,#18036,#18037));
#4147=EDGE_LOOP('',(#18038,#18039,#18040,#18041));
#4148=EDGE_LOOP('',(#18042,#18043,#18044,#18045));
#4149=EDGE_LOOP('',(#18046,#18047,#18048,#18049));
#4150=EDGE_LOOP('',(#18050,#18051,#18052,#18053));
#4151=EDGE_LOOP('',(#18054,#18055,#18056,#18057));
#4152=EDGE_LOOP('',(#18058,#18059,#18060,#18061));
#4153=EDGE_LOOP('',(#18062,#18063,#18064,#18065));
#4154=EDGE_LOOP('',(#18066,#18067,#18068,#18069));
#4155=EDGE_LOOP('',(#18070,#18071,#18072,#18073));
#4156=EDGE_LOOP('',(#18074,#18075,#18076,#18077));
#4157=EDGE_LOOP('',(#18078,#18079,#18080,#18081));
#4158=EDGE_LOOP('',(#18082,#18083,#18084,#18085));
#4159=EDGE_LOOP('',(#18086,#18087,#18088,#18089));
#4160=EDGE_LOOP('',(#18090,#18091,#18092,#18093));
#4161=EDGE_LOOP('',(#18094,#18095,#18096,#18097));
#4162=EDGE_LOOP('',(#18098,#18099,#18100,#18101));
#4163=EDGE_LOOP('',(#18102,#18103,#18104,#18105));
#4164=EDGE_LOOP('',(#18106,#18107,#18108,#18109));
#4165=EDGE_LOOP('',(#18110,#18111,#18112,#18113));
#4166=EDGE_LOOP('',(#18114,#18115,#18116,#18117));
#4167=EDGE_LOOP('',(#18118,#18119,#18120,#18121));
#4168=EDGE_LOOP('',(#18122,#18123,#18124,#18125));
#4169=EDGE_LOOP('',(#18126,#18127,#18128,#18129));
#4170=EDGE_LOOP('',(#18130,#18131,#18132,#18133));
#4171=EDGE_LOOP('',(#18134,#18135,#18136,#18137));
#4172=EDGE_LOOP('',(#18138,#18139,#18140,#18141));
#4173=EDGE_LOOP('',(#18142,#18143,#18144,#18145));
#4174=EDGE_LOOP('',(#18146,#18147,#18148,#18149));
#4175=EDGE_LOOP('',(#18150,#18151,#18152,#18153));
#4176=EDGE_LOOP('',(#18154,#18155,#18156,#18157));
#4177=EDGE_LOOP('',(#18158,#18159,#18160,#18161));
#4178=EDGE_LOOP('',(#18162,#18163,#18164,#18165));
#4179=EDGE_LOOP('',(#18166,#18167,#18168,#18169));
#4180=EDGE_LOOP('',(#18170,#18171,#18172,#18173));
#4181=EDGE_LOOP('',(#18174,#18175,#18176,#18177));
#4182=EDGE_LOOP('',(#18178,#18179,#18180,#18181));
#4183=EDGE_LOOP('',(#18182,#18183,#18184,#18185));
#4184=EDGE_LOOP('',(#18186,#18187,#18188,#18189));
#4185=EDGE_LOOP('',(#18190,#18191,#18192,#18193));
#4186=EDGE_LOOP('',(#18194,#18195,#18196,#18197));
#4187=EDGE_LOOP('',(#18198,#18199,#18200,#18201));
#4188=EDGE_LOOP('',(#18202,#18203,#18204,#18205));
#4189=EDGE_LOOP('',(#18206,#18207,#18208,#18209));
#4190=EDGE_LOOP('',(#18210,#18211,#18212,#18213));
#4191=EDGE_LOOP('',(#18214,#18215,#18216,#18217));
#4192=EDGE_LOOP('',(#18218,#18219,#18220,#18221));
#4193=EDGE_LOOP('',(#18222,#18223,#18224,#18225));
#4194=EDGE_LOOP('',(#18226,#18227,#18228,#18229));
#4195=EDGE_LOOP('',(#18230,#18231,#18232,#18233));
#4196=EDGE_LOOP('',(#18234,#18235,#18236,#18237));
#4197=EDGE_LOOP('',(#18238,#18239,#18240,#18241));
#4198=EDGE_LOOP('',(#18242,#18243,#18244,#18245));
#4199=EDGE_LOOP('',(#18246,#18247,#18248,#18249));
#4200=EDGE_LOOP('',(#18250,#18251,#18252));
#4201=EDGE_LOOP('',(#18253,#18254,#18255,#18256,#18257));
#4202=EDGE_LOOP('',(#18258,#18259,#18260,#18261));
#4203=EDGE_LOOP('',(#18262,#18263,#18264,#18265));
#4204=EDGE_LOOP('',(#18266,#18267,#18268,#18269));
#4205=EDGE_LOOP('',(#18270,#18271,#18272,#18273));
#4206=EDGE_LOOP('',(#18274,#18275,#18276,#18277));
#4207=EDGE_LOOP('',(#18278,#18279,#18280,#18281));
#4208=EDGE_LOOP('',(#18282,#18283,#18284,#18285));
#4209=EDGE_LOOP('',(#18286,#18287,#18288,#18289));
#4210=EDGE_LOOP('',(#18290,#18291,#18292,#18293));
#4211=EDGE_LOOP('',(#18294,#18295,#18296,#18297));
#4212=EDGE_LOOP('',(#18298,#18299,#18300,#18301));
#4213=EDGE_LOOP('',(#18302,#18303,#18304,#18305,#18306,#18307));
#4214=EDGE_LOOP('',(#18308,#18309,#18310,#18311,#18312,#18313,#18314,#18315,
#18316,#18317,#18318,#18319,#18320,#18321,#18322,#18323,#18324,#18325,#18326,
#18327,#18328,#18329,#18330,#18331,#18332,#18333,#18334,#18335,#18336));
#4215=EDGE_LOOP('',(#18337,#18338,#18339,#18340,#18341));
#4216=EDGE_LOOP('',(#18342,#18343,#18344,#18345));
#4217=EDGE_LOOP('',(#18346,#18347,#18348,#18349,#18350,#18351,#18352,#18353,
#18354,#18355,#18356,#18357,#18358,#18359,#18360,#18361,#18362,#18363,#18364,
#18365,#18366,#18367,#18368,#18369,#18370,#18371,#18372,#18373,#18374,#18375));
#4218=EDGE_LOOP('',(#18376,#18377,#18378,#18379));
#4219=EDGE_LOOP('',(#18380));
#4220=EDGE_LOOP('',(#18381,#18382,#18383,#18384));
#4221=EDGE_LOOP('',(#18385,#18386,#18387,#18388));
#4222=EDGE_LOOP('',(#18389));
#4223=EDGE_LOOP('',(#18390));
#4224=EDGE_LOOP('',(#18391,#18392,#18393,#18394,#18395,#18396));
#4225=EDGE_LOOP('',(#18397,#18398,#18399,#18400,#18401,#18402));
#4226=EDGE_LOOP('',(#18403));
#4227=EDGE_LOOP('',(#18404,#18405,#18406,#18407,#18408,#18409));
#4228=EDGE_LOOP('',(#18410,#18411,#18412,#18413));
#4229=EDGE_LOOP('',(#18414,#18415,#18416,#18417,#18418,#18419));
#4230=EDGE_LOOP('',(#18420,#18421,#18422,#18423,#18424,#18425));
#4231=EDGE_LOOP('',(#18426,#18427,#18428,#18429,#18430,#18431));
#4232=EDGE_LOOP('',(#18432,#18433,#18434,#18435,#18436));
#4233=EDGE_LOOP('',(#18437,#18438,#18439,#18440));
#4234=EDGE_LOOP('',(#18441,#18442,#18443,#18444,#18445,#18446));
#4235=EDGE_LOOP('',(#18447,#18448,#18449,#18450));
#4236=EDGE_LOOP('',(#18451,#18452,#18453,#18454,#18455));
#4237=EDGE_LOOP('',(#18456,#18457,#18458,#18459,#18460,#18461,#18462,#18463,
#18464,#18465,#18466,#18467,#18468,#18469,#18470,#18471));
#4238=EDGE_LOOP('',(#18472));
#4239=EDGE_LOOP('',(#18473,#18474,#18475,#18476,#18477,#18478));
#4240=EDGE_LOOP('',(#18479,#18480,#18481,#18482,#18483,#18484));
#4241=EDGE_LOOP('',(#18485,#18486,#18487,#18488,#18489,#18490));
#4242=EDGE_LOOP('',(#18491,#18492,#18493,#18494));
#4243=EDGE_LOOP('',(#18495,#18496,#18497,#18498,#18499));
#4244=EDGE_LOOP('',(#18500,#18501,#18502,#18503,#18504,#18505));
#4245=EDGE_LOOP('',(#18506,#18507,#18508,#18509,#18510));
#4246=EDGE_LOOP('',(#18511,#18512,#18513,#18514));
#4247=EDGE_LOOP('',(#18515,#18516,#18517,#18518,#18519,#18520));
#4248=EDGE_LOOP('',(#18521,#18522,#18523,#18524));
#4249=EDGE_LOOP('',(#18525,#18526,#18527,#18528));
#4250=EDGE_LOOP('',(#18529,#18530,#18531,#18532));
#4251=EDGE_LOOP('',(#18533,#18534,#18535,#18536));
#4252=EDGE_LOOP('',(#18537,#18538,#18539,#18540,#18541,#18542));
#4253=EDGE_LOOP('',(#18543,#18544,#18545,#18546,#18547,#18548));
#4254=EDGE_LOOP('',(#18549,#18550,#18551,#18552));
#4255=EDGE_LOOP('',(#18553,#18554,#18555,#18556,#18557));
#4256=EDGE_LOOP('',(#18558,#18559,#18560,#18561,#18562,#18563));
#4257=EDGE_LOOP('',(#18564,#18565,#18566,#18567));
#4258=EDGE_LOOP('',(#18568,#18569,#18570,#18571,#18572,#18573));
#4259=EDGE_LOOP('',(#18574,#18575,#18576,#18577,#18578));
#4260=EDGE_LOOP('',(#18579,#18580,#18581,#18582));
#4261=EDGE_LOOP('',(#18583,#18584,#18585,#18586));
#4262=EDGE_LOOP('',(#18587,#18588,#18589,#18590));
#4263=EDGE_LOOP('',(#18591,#18592,#18593,#18594,#18595,#18596));
#4264=EDGE_LOOP('',(#18597,#18598,#18599,#18600,#18601,#18602));
#4265=EDGE_LOOP('',(#18603,#18604,#18605,#18606));
#4266=EDGE_LOOP('',(#18607,#18608,#18609,#18610,#18611));
#4267=EDGE_LOOP('',(#18612,#18613,#18614,#18615,#18616,#18617));
#4268=EDGE_LOOP('',(#18618,#18619,#18620,#18621));
#4269=EDGE_LOOP('',(#18622,#18623,#18624,#18625,#18626));
#4270=EDGE_LOOP('',(#18627,#18628,#18629,#18630));
#4271=EDGE_LOOP('',(#18631,#18632,#18633,#18634));
#4272=EDGE_LOOP('',(#18635,#18636,#18637,#18638));
#4273=EDGE_LOOP('',(#18639,#18640,#18641,#18642));
#4274=EDGE_LOOP('',(#18643,#18644,#18645,#18646));
#4275=EDGE_LOOP('',(#18647,#18648,#18649,#18650));
#4276=EDGE_LOOP('',(#18651,#18652,#18653,#18654));
#4277=EDGE_LOOP('',(#18655,#18656,#18657,#18658));
#4278=EDGE_LOOP('',(#18659,#18660,#18661,#18662,#18663,#18664));
#4279=EDGE_LOOP('',(#18665,#18666,#18667,#18668));
#4280=EDGE_LOOP('',(#18669,#18670,#18671,#18672,#18673,#18674));
#4281=EDGE_LOOP('',(#18675,#18676,#18677,#18678));
#4282=EDGE_LOOP('',(#18679,#18680,#18681,#18682));
#4283=EDGE_LOOP('',(#18683,#18684,#18685,#18686,#18687,#18688));
#4284=EDGE_LOOP('',(#18689,#18690,#18691,#18692,#18693,#18694));
#4285=EDGE_LOOP('',(#18695,#18696,#18697,#18698,#18699,#18700));
#4286=EDGE_LOOP('',(#18701,#18702,#18703,#18704,#18705,#18706,#18707,#18708,
#18709,#18710,#18711,#18712,#18713,#18714,#18715,#18716));
#4287=EDGE_LOOP('',(#18717));
#4288=EDGE_LOOP('',(#18718,#18719,#18720,#18721));
#4289=EDGE_LOOP('',(#18722,#18723,#18724,#18725));
#4290=EDGE_LOOP('',(#18726,#18727,#18728,#18729));
#4291=EDGE_LOOP('',(#18730,#18731,#18732,#18733,#18734,#18735));
#4292=EDGE_LOOP('',(#18736,#18737,#18738,#18739));
#4293=EDGE_LOOP('',(#18740,#18741,#18742,#18743,#18744,#18745));
#4294=EDGE_LOOP('',(#18746));
#4295=EDGE_LOOP('',(#18747,#18748,#18749,#18750));
#4296=EDGE_LOOP('',(#18751,#18752,#18753,#18754));
#4297=EDGE_LOOP('',(#18755,#18756,#18757,#18758));
#4298=EDGE_LOOP('',(#18759));
#4299=EDGE_LOOP('',(#18760,#18761,#18762,#18763));
#4300=EDGE_LOOP('',(#18764,#18765,#18766,#18767,#18768));
#4301=EDGE_LOOP('',(#18769,#18770,#18771,#18772,#18773,#18774,#18775,#18776,
#18777));
#4302=EDGE_LOOP('',(#18778));
#4303=EDGE_LOOP('',(#18779));
#4304=EDGE_LOOP('',(#18780));
#4305=EDGE_LOOP('',(#18781));
#4306=EDGE_LOOP('',(#18782));
#4307=EDGE_LOOP('',(#18783));
#4308=EDGE_LOOP('',(#18784,#18785,#18786,#18787,#18788,#18789,#18790));
#4309=EDGE_LOOP('',(#18791,#18792,#18793,#18794));
#4310=EDGE_LOOP('',(#18795,#18796,#18797));
#4311=EDGE_LOOP('',(#18798,#18799,#18800,#18801,#18802,#18803,#18804,#18805,
#18806,#18807,#18808,#18809,#18810,#18811,#18812,#18813,#18814,#18815,#18816,
#18817,#18818,#18819,#18820,#18821,#18822,#18823,#18824,#18825,#18826,#18827,
#18828,#18829,#18830,#18831));
#4312=EDGE_LOOP('',(#18832,#18833,#18834,#18835,#18836,#18837));
#4313=EDGE_LOOP('',(#18838,#18839,#18840,#18841,#18842,#18843));
#4314=EDGE_LOOP('',(#18844,#18845,#18846,#18847,#18848,#18849,#18850,#18851));
#4315=EDGE_LOOP('',(#18852,#18853,#18854,#18855,#18856,#18857));
#4316=EDGE_LOOP('',(#18858,#18859,#18860,#18861,#18862,#18863));
#4317=EDGE_LOOP('',(#18864,#18865,#18866,#18867,#18868,#18869));
#4318=EDGE_LOOP('',(#18870,#18871,#18872,#18873));
#4319=EDGE_LOOP('',(#18874));
#4320=EDGE_LOOP('',(#18875));
#4321=EDGE_LOOP('',(#18876,#18877,#18878,#18879));
#4322=EDGE_LOOP('',(#18880,#18881,#18882,#18883));
#4323=EDGE_LOOP('',(#18884));
#4324=EDGE_LOOP('',(#18885));
#4325=EDGE_LOOP('',(#18886,#18887,#18888,#18889));
#4326=EDGE_LOOP('',(#18890,#18891,#18892,#18893));
#4327=EDGE_LOOP('',(#18894,#18895,#18896,#18897));
#4328=EDGE_LOOP('',(#18898,#18899,#18900,#18901));
#4329=EDGE_LOOP('',(#18902,#18903,#18904,#18905));
#4330=EDGE_LOOP('',(#18906,#18907,#18908,#18909));
#4331=EDGE_LOOP('',(#18910,#18911,#18912,#18913));
#4332=EDGE_LOOP('',(#18914,#18915,#18916,#18917));
#4333=EDGE_LOOP('',(#18918,#18919,#18920));
#4334=EDGE_LOOP('',(#18921,#18922,#18923,#18924,#18925));
#4335=EDGE_LOOP('',(#18926,#18927,#18928,#18929));
#4336=EDGE_LOOP('',(#18930,#18931,#18932,#18933));
#4337=EDGE_LOOP('',(#18934,#18935,#18936,#18937));
#4338=EDGE_LOOP('',(#18938,#18939,#18940,#18941));
#4339=EDGE_LOOP('',(#18942,#18943,#18944,#18945));
#4340=EDGE_LOOP('',(#18946,#18947,#18948,#18949,#18950,#18951));
#4341=EDGE_LOOP('',(#18952,#18953,#18954,#18955,#18956,#18957,#18958,#18959,
#18960,#18961,#18962,#18963,#18964,#18965,#18966,#18967,#18968));
#4342=EDGE_LOOP('',(#18969,#18970,#18971,#18972,#18973));
#4343=EDGE_LOOP('',(#18974,#18975,#18976,#18977));
#4344=EDGE_LOOP('',(#18978,#18979,#18980,#18981,#18982,#18983,#18984,#18985,
#18986,#18987,#18988,#18989,#18990,#18991,#18992,#18993,#18994,#18995));
#4345=EDGE_LOOP('',(#18996,#18997));
#4346=EDGE_LOOP('',(#18998,#18999));
#4347=EDGE_LOOP('',(#19000,#19001));
#4348=EDGE_LOOP('',(#19002,#19003));
#4349=EDGE_LOOP('',(#19004,#19005));
#4350=EDGE_LOOP('',(#19006,#19007));
#4351=EDGE_LOOP('',(#19008,#19009,#19010,#19011,#19012,#19013,#19014,#19015,
#19016,#19017,#19018,#19019,#19020,#19021,#19022,#19023,#19024,#19025,#19026,
#19027,#19028,#19029,#19030,#19031,#19032,#19033,#19034));
#4352=EDGE_LOOP('',(#19035,#19036,#19037,#19038));
#4353=EDGE_LOOP('',(#19039,#19040,#19041));
#4354=EDGE_LOOP('',(#19042,#19043,#19044,#19045));
#4355=EDGE_LOOP('',(#19046,#19047,#19048));
#4356=EDGE_LOOP('',(#19049,#19050,#19051));
#4357=EDGE_LOOP('',(#19052,#19053,#19054,#19055));
#4358=EDGE_LOOP('',(#19056,#19057,#19058));
#4359=EDGE_LOOP('',(#19059,#19060,#19061,#19062));
#4360=EDGE_LOOP('',(#19063,#19064,#19065));
#4361=EDGE_LOOP('',(#19066,#19067,#19068));
#4362=EDGE_LOOP('',(#19069,#19070,#19071));
#4363=EDGE_LOOP('',(#19072,#19073,#19074));
#4364=EDGE_LOOP('',(#19075,#19076,#19077));
#4365=EDGE_LOOP('',(#19078,#19079,#19080));
#4366=EDGE_LOOP('',(#19081,#19082,#19083));
#4367=EDGE_LOOP('',(#19084,#19085,#19086,#19087));
#4368=EDGE_LOOP('',(#19088,#19089,#19090,#19091));
#4369=EDGE_LOOP('',(#19092,#19093,#19094));
#4370=EDGE_LOOP('',(#19095,#19096,#19097));
#4371=EDGE_LOOP('',(#19098,#19099,#19100));
#4372=EDGE_LOOP('',(#19101,#19102,#19103,#19104));
#4373=EDGE_LOOP('',(#19105,#19106,#19107));
#4374=EDGE_LOOP('',(#19108,#19109,#19110));
#4375=EDGE_LOOP('',(#19111,#19112,#19113));
#4376=EDGE_LOOP('',(#19114));
#4377=EDGE_LOOP('',(#19115,#19116,#19117,#19118,#19119,#19120));
#4378=EDGE_LOOP('',(#19121,#19122,#19123,#19124));
#4379=EDGE_LOOP('',(#19125,#19126,#19127,#19128,#19129,#19130));
#4380=EDGE_LOOP('',(#19131));
#4381=EDGE_LOOP('',(#19132,#19133,#19134,#19135,#19136,#19137));
#4382=EDGE_LOOP('',(#19138,#19139,#19140,#19141));
#4383=EDGE_LOOP('',(#19142,#19143,#19144,#19145));
#4384=EDGE_LOOP('',(#19146,#19147,#19148,#19149));
#4385=EDGE_LOOP('',(#19150,#19151,#19152,#19153));
#4386=EDGE_LOOP('',(#19154,#19155,#19156,#19157));
#4387=EDGE_LOOP('',(#19158,#19159,#19160,#19161));
#4388=EDGE_LOOP('',(#19162,#19163,#19164,#19165));
#4389=EDGE_LOOP('',(#19166,#19167,#19168,#19169));
#4390=EDGE_LOOP('',(#19170,#19171,#19172,#19173));
#4391=EDGE_LOOP('',(#19174,#19175,#19176,#19177));
#4392=EDGE_LOOP('',(#19178,#19179,#19180));
#4393=EDGE_LOOP('',(#19181,#19182,#19183));
#4394=EDGE_LOOP('',(#19184,#19185,#19186));
#4395=EDGE_LOOP('',(#19187,#19188,#19189));
#4396=EDGE_LOOP('',(#19190,#19191,#19192));
#4397=EDGE_LOOP('',(#19193,#19194,#19195,#19196));
#4398=EDGE_LOOP('',(#19197,#19198,#19199));
#4399=EDGE_LOOP('',(#19200,#19201,#19202));
#4400=EDGE_LOOP('',(#19203,#19204,#19205,#19206));
#4401=EDGE_LOOP('',(#19207,#19208,#19209,#19210));
#4402=EDGE_LOOP('',(#19211,#19212,#19213));
#4403=EDGE_LOOP('',(#19214,#19215,#19216,#19217));
#4404=EDGE_LOOP('',(#19218,#19219,#19220,#19221));
#4405=EDGE_LOOP('',(#19222,#19223,#19224,#19225));
#4406=EDGE_LOOP('',(#19226,#19227,#19228,#19229));
#4407=EDGE_LOOP('',(#19230,#19231,#19232,#19233));
#4408=EDGE_LOOP('',(#19234,#19235,#19236,#19237));
#4409=EDGE_LOOP('',(#19238,#19239,#19240,#19241));
#4410=EDGE_LOOP('',(#19242,#19243,#19244,#19245));
#4411=EDGE_LOOP('',(#19246,#19247,#19248,#19249));
#4412=EDGE_LOOP('',(#19250,#19251,#19252,#19253));
#4413=EDGE_LOOP('',(#19254,#19255,#19256,#19257));
#4414=EDGE_LOOP('',(#19258,#19259,#19260,#19261));
#4415=EDGE_LOOP('',(#19262,#19263,#19264,#19265));
#4416=EDGE_LOOP('',(#19266,#19267,#19268,#19269));
#4417=EDGE_LOOP('',(#19270,#19271,#19272,#19273));
#4418=EDGE_LOOP('',(#19274,#19275,#19276,#19277));
#4419=EDGE_LOOP('',(#19278,#19279,#19280,#19281));
#4420=EDGE_LOOP('',(#19282,#19283,#19284,#19285));
#4421=EDGE_LOOP('',(#19286,#19287,#19288,#19289));
#4422=EDGE_LOOP('',(#19290,#19291,#19292,#19293));
#4423=EDGE_LOOP('',(#19294,#19295,#19296,#19297));
#4424=EDGE_LOOP('',(#19298,#19299,#19300,#19301));
#4425=EDGE_LOOP('',(#19302,#19303,#19304,#19305));
#4426=EDGE_LOOP('',(#19306,#19307,#19308,#19309));
#4427=EDGE_LOOP('',(#19310,#19311,#19312,#19313));
#4428=EDGE_LOOP('',(#19314,#19315,#19316,#19317));
#4429=EDGE_LOOP('',(#19318,#19319,#19320,#19321));
#4430=EDGE_LOOP('',(#19322,#19323,#19324,#19325));
#4431=EDGE_LOOP('',(#19326,#19327,#19328,#19329));
#4432=EDGE_LOOP('',(#19330,#19331,#19332,#19333));
#4433=EDGE_LOOP('',(#19334,#19335,#19336,#19337));
#4434=EDGE_LOOP('',(#19338,#19339,#19340,#19341));
#4435=EDGE_LOOP('',(#19342,#19343,#19344,#19345));
#4436=EDGE_LOOP('',(#19346,#19347,#19348,#19349));
#4437=EDGE_LOOP('',(#19350,#19351,#19352,#19353));
#4438=EDGE_LOOP('',(#19354,#19355,#19356,#19357));
#4439=EDGE_LOOP('',(#19358,#19359,#19360,#19361));
#4440=EDGE_LOOP('',(#19362,#19363,#19364,#19365));
#4441=EDGE_LOOP('',(#19366,#19367,#19368,#19369));
#4442=EDGE_LOOP('',(#19370,#19371,#19372,#19373));
#4443=EDGE_LOOP('',(#19374,#19375,#19376,#19377));
#4444=EDGE_LOOP('',(#19378,#19379,#19380,#19381));
#4445=EDGE_LOOP('',(#19382,#19383,#19384,#19385));
#4446=EDGE_LOOP('',(#19386,#19387,#19388,#19389));
#4447=EDGE_LOOP('',(#19390,#19391,#19392,#19393));
#4448=EDGE_LOOP('',(#19394,#19395,#19396,#19397));
#4449=EDGE_LOOP('',(#19398,#19399,#19400));
#4450=EDGE_LOOP('',(#19401,#19402,#19403,#19404,#19405));
#4451=EDGE_LOOP('',(#19406,#19407,#19408,#19409));
#4452=EDGE_LOOP('',(#19410,#19411,#19412,#19413));
#4453=EDGE_LOOP('',(#19414,#19415,#19416,#19417));
#4454=EDGE_LOOP('',(#19418,#19419,#19420,#19421));
#4455=EDGE_LOOP('',(#19422,#19423,#19424,#19425));
#4456=EDGE_LOOP('',(#19426,#19427,#19428,#19429));
#4457=EDGE_LOOP('',(#19430,#19431,#19432,#19433));
#4458=EDGE_LOOP('',(#19434,#19435,#19436,#19437));
#4459=EDGE_LOOP('',(#19438,#19439,#19440,#19441));
#4460=EDGE_LOOP('',(#19442,#19443,#19444,#19445));
#4461=EDGE_LOOP('',(#19446,#19447,#19448,#19449));
#4462=EDGE_LOOP('',(#19450,#19451,#19452,#19453));
#4463=EDGE_LOOP('',(#19454,#19455,#19456,#19457));
#4464=EDGE_LOOP('',(#19458,#19459,#19460,#19461));
#4465=EDGE_LOOP('',(#19462,#19463,#19464,#19465));
#4466=EDGE_LOOP('',(#19466,#19467,#19468,#19469));
#4467=EDGE_LOOP('',(#19470,#19471,#19472,#19473));
#4468=EDGE_LOOP('',(#19474,#19475,#19476,#19477));
#4469=EDGE_LOOP('',(#19478,#19479,#19480,#19481));
#4470=EDGE_LOOP('',(#19482,#19483,#19484,#19485));
#4471=EDGE_LOOP('',(#19486,#19487,#19488,#19489));
#4472=EDGE_LOOP('',(#19490,#19491,#19492,#19493));
#4473=EDGE_LOOP('',(#19494,#19495,#19496,#19497));
#4474=EDGE_LOOP('',(#19498,#19499,#19500,#19501));
#4475=EDGE_LOOP('',(#19502,#19503,#19504,#19505));
#4476=EDGE_LOOP('',(#19506,#19507,#19508,#19509));
#4477=EDGE_LOOP('',(#19510,#19511,#19512,#19513));
#4478=EDGE_LOOP('',(#19514,#19515,#19516,#19517,#19518,#19519));
#4479=EDGE_LOOP('',(#19520,#19521,#19522,#19523,#19524,#19525,#19526,#19527,
#19528,#19529,#19530,#19531,#19532,#19533,#19534,#19535,#19536,#19537,#19538,
#19539,#19540,#19541,#19542,#19543,#19544,#19545,#19546,#19547,#19548,#19549,
#19550,#19551,#19552,#19553,#19554,#19555,#19556,#19557,#19558,#19559,#19560,
#19561,#19562,#19563,#19564,#19565,#19566,#19567,#19568,#19569,#19570,#19571,
#19572,#19573,#19574,#19575,#19576,#19577,#19578,#19579,#19580));
#4480=EDGE_LOOP('',(#19581,#19582,#19583,#19584,#19585));
#4481=EDGE_LOOP('',(#19586,#19587,#19588,#19589));
#4482=EDGE_LOOP('',(#19590,#19591,#19592,#19593,#19594,#19595,#19596,#19597,
#19598,#19599,#19600,#19601,#19602,#19603,#19604,#19605,#19606,#19607,#19608,
#19609,#19610,#19611,#19612,#19613,#19614,#19615,#19616,#19617,#19618,#19619,
#19620,#19621,#19622,#19623,#19624,#19625,#19626,#19627,#19628,#19629,#19630,
#19631,#19632,#19633,#19634,#19635,#19636,#19637,#19638,#19639,#19640,#19641,
#19642,#19643,#19644,#19645,#19646,#19647,#19648,#19649,#19650,#19651));
#4483=EDGE_LOOP('',(#19652,#19653));
#4484=EDGE_LOOP('',(#19654,#19655));
#4485=EDGE_LOOP('',(#19656,#19657));
#4486=EDGE_LOOP('',(#19658,#19659));
#4487=EDGE_LOOP('',(#19660,#19661));
#4488=EDGE_LOOP('',(#19662,#19663));
#4489=EDGE_LOOP('',(#19664,#19665,#19666,#19667,#19668,#19669,#19670,#19671,
#19672,#19673,#19674,#19675,#19676,#19677,#19678,#19679,#19680,#19681,#19682,
#19683,#19684,#19685,#19686,#19687,#19688,#19689,#19690));
#4490=EDGE_LOOP('',(#19691,#19692,#19693,#19694));
#4491=EDGE_LOOP('',(#19695,#19696,#19697));
#4492=EDGE_LOOP('',(#19698,#19699,#19700,#19701));
#4493=EDGE_LOOP('',(#19702,#19703,#19704));
#4494=EDGE_LOOP('',(#19705,#19706,#19707));
#4495=EDGE_LOOP('',(#19708,#19709,#19710,#19711));
#4496=EDGE_LOOP('',(#19712,#19713,#19714));
#4497=EDGE_LOOP('',(#19715,#19716,#19717,#19718));
#4498=EDGE_LOOP('',(#19719,#19720,#19721));
#4499=EDGE_LOOP('',(#19722,#19723,#19724));
#4500=EDGE_LOOP('',(#19725,#19726,#19727));
#4501=EDGE_LOOP('',(#19728,#19729,#19730));
#4502=EDGE_LOOP('',(#19731,#19732,#19733));
#4503=EDGE_LOOP('',(#19734,#19735,#19736));
#4504=EDGE_LOOP('',(#19737,#19738,#19739));
#4505=EDGE_LOOP('',(#19740,#19741,#19742,#19743));
#4506=EDGE_LOOP('',(#19744,#19745,#19746,#19747));
#4507=EDGE_LOOP('',(#19748,#19749,#19750));
#4508=EDGE_LOOP('',(#19751,#19752,#19753));
#4509=EDGE_LOOP('',(#19754,#19755,#19756));
#4510=EDGE_LOOP('',(#19757,#19758,#19759,#19760));
#4511=EDGE_LOOP('',(#19761,#19762,#19763));
#4512=EDGE_LOOP('',(#19764,#19765,#19766));
#4513=EDGE_LOOP('',(#19767,#19768,#19769));
#4514=EDGE_LOOP('',(#19770));
#4515=EDGE_LOOP('',(#19771,#19772,#19773,#19774,#19775,#19776));
#4516=EDGE_LOOP('',(#19777,#19778,#19779,#19780));
#4517=EDGE_LOOP('',(#19781,#19782,#19783,#19784,#19785,#19786));
#4518=EDGE_LOOP('',(#19787));
#4519=EDGE_LOOP('',(#19788,#19789,#19790,#19791,#19792,#19793));
#4520=EDGE_LOOP('',(#19794,#19795,#19796,#19797));
#4521=EDGE_LOOP('',(#19798,#19799,#19800,#19801));
#4522=EDGE_LOOP('',(#19802));
#4523=EDGE_LOOP('',(#19803));
#4524=EDGE_LOOP('',(#19804,#19805,#19806,#19807));
#4525=EDGE_LOOP('',(#19808));
#4526=EDGE_LOOP('',(#19809));
#4527=EDGE_LOOP('',(#19810,#19811,#19812,#19813,#19814,#19815,#19816,#19817,
#19818,#19819));
#4528=EDGE_LOOP('',(#19820,#19821,#19822,#19823));
#4529=EDGE_LOOP('',(#19824,#19825,#19826,#19827));
#4530=EDGE_LOOP('',(#19828,#19829,#19830,#19831));
#4531=EDGE_LOOP('',(#19832,#19833,#19834,#19835,#19836,#19837,#19838,#19839,
#19840,#19841));
#4532=EDGE_LOOP('',(#19842,#19843,#19844,#19845));
#4533=EDGE_LOOP('',(#19846,#19847,#19848,#19849));
#4534=EDGE_LOOP('',(#19850,#19851,#19852,#19853,#19854,#19855));
#4535=EDGE_LOOP('',(#19856,#19857,#19858,#19859));
#4536=EDGE_LOOP('',(#19860,#19861,#19862,#19863));
#4537=EDGE_LOOP('',(#19864,#19865,#19866,#19867));
#4538=EDGE_LOOP('',(#19868,#19869,#19870,#19871));
#4539=EDGE_LOOP('',(#19872,#19873,#19874,#19875));
#4540=EDGE_LOOP('',(#19876,#19877,#19878,#19879));
#4541=EDGE_LOOP('',(#19880,#19881,#19882,#19883));
#4542=EDGE_LOOP('',(#19884,#19885,#19886,#19887));
#4543=EDGE_LOOP('',(#19888,#19889,#19890,#19891));
#4544=EDGE_LOOP('',(#19892,#19893,#19894,#19895));
#4545=EDGE_LOOP('',(#19896,#19897,#19898,#19899));
#4546=EDGE_LOOP('',(#19900,#19901,#19902,#19903));
#4547=EDGE_LOOP('',(#19904,#19905,#19906,#19907));
#4548=EDGE_LOOP('',(#19908,#19909,#19910,#19911));
#4549=EDGE_LOOP('',(#19912,#19913,#19914,#19915));
#4550=EDGE_LOOP('',(#19916,#19917,#19918,#19919));
#4551=EDGE_LOOP('',(#19920,#19921,#19922,#19923));
#4552=EDGE_LOOP('',(#19924,#19925,#19926,#19927));
#4553=EDGE_LOOP('',(#19928,#19929,#19930,#19931));
#4554=EDGE_LOOP('',(#19932,#19933,#19934));
#4555=EDGE_LOOP('',(#19935,#19936,#19937,#19938,#19939));
#4556=EDGE_LOOP('',(#19940,#19941,#19942,#19943));
#4557=EDGE_LOOP('',(#19944,#19945,#19946,#19947));
#4558=EDGE_LOOP('',(#19948,#19949,#19950,#19951));
#4559=EDGE_LOOP('',(#19952,#19953,#19954,#19955));
#4560=EDGE_LOOP('',(#19956,#19957,#19958,#19959));
#4561=EDGE_LOOP('',(#19960,#19961,#19962,#19963));
#4562=EDGE_LOOP('',(#19964,#19965,#19966,#19967));
#4563=EDGE_LOOP('',(#19968,#19969,#19970,#19971));
#4564=EDGE_LOOP('',(#19972,#19973,#19974,#19975));
#4565=EDGE_LOOP('',(#19976,#19977,#19978,#19979));
#4566=EDGE_LOOP('',(#19980,#19981,#19982,#19983));
#4567=EDGE_LOOP('',(#19984,#19985,#19986,#19987));
#4568=EDGE_LOOP('',(#19988,#19989,#19990,#19991));
#4569=EDGE_LOOP('',(#19992,#19993,#19994,#19995));
#4570=EDGE_LOOP('',(#19996,#19997,#19998,#19999));
#4571=EDGE_LOOP('',(#20000,#20001,#20002,#20003));
#4572=EDGE_LOOP('',(#20004,#20005,#20006,#20007));
#4573=EDGE_LOOP('',(#20008,#20009,#20010,#20011,#20012,#20013));
#4574=EDGE_LOOP('',(#20014,#20015,#20016,#20017,#20018,#20019,#20020,#20021,
#20022,#20023,#20024,#20025,#20026,#20027,#20028,#20029,#20030,#20031,#20032,
#20033,#20034,#20035,#20036,#20037,#20038,#20039,#20040,#20041,#20042,#20043,
#20044,#20045,#20046,#20047,#20048,#20049,#20050,#20051,#20052,#20053,#20054));
#4575=EDGE_LOOP('',(#20055,#20056,#20057,#20058,#20059));
#4576=EDGE_LOOP('',(#20060,#20061,#20062,#20063));
#4577=EDGE_LOOP('',(#20064,#20065,#20066,#20067,#20068,#20069,#20070,#20071,
#20072,#20073,#20074,#20075,#20076,#20077,#20078,#20079,#20080,#20081,#20082,
#20083,#20084,#20085,#20086,#20087,#20088,#20089,#20090,#20091,#20092,#20093,
#20094,#20095,#20096,#20097,#20098,#20099,#20100,#20101,#20102,#20103,#20104,
#20105));
#4578=EDGE_LOOP('',(#20106,#20107));
#4579=EDGE_LOOP('',(#20108,#20109));
#4580=EDGE_LOOP('',(#20110,#20111));
#4581=EDGE_LOOP('',(#20112,#20113));
#4582=EDGE_LOOP('',(#20114,#20115));
#4583=EDGE_LOOP('',(#20116,#20117));
#4584=EDGE_LOOP('',(#20118,#20119,#20120,#20121,#20122,#20123,#20124,#20125,
#20126,#20127,#20128,#20129,#20130,#20131,#20132,#20133,#20134,#20135,#20136,
#20137,#20138,#20139,#20140,#20141,#20142,#20143,#20144));
#4585=EDGE_LOOP('',(#20145,#20146,#20147,#20148));
#4586=EDGE_LOOP('',(#20149,#20150,#20151));
#4587=EDGE_LOOP('',(#20152,#20153,#20154,#20155));
#4588=EDGE_LOOP('',(#20156,#20157,#20158));
#4589=EDGE_LOOP('',(#20159,#20160,#20161));
#4590=EDGE_LOOP('',(#20162,#20163,#20164,#20165));
#4591=EDGE_LOOP('',(#20166,#20167,#20168));
#4592=EDGE_LOOP('',(#20169,#20170,#20171,#20172));
#4593=EDGE_LOOP('',(#20173,#20174,#20175));
#4594=EDGE_LOOP('',(#20176,#20177,#20178));
#4595=EDGE_LOOP('',(#20179,#20180,#20181));
#4596=EDGE_LOOP('',(#20182,#20183,#20184));
#4597=EDGE_LOOP('',(#20185,#20186,#20187));
#4598=EDGE_LOOP('',(#20188,#20189,#20190));
#4599=EDGE_LOOP('',(#20191,#20192,#20193));
#4600=EDGE_LOOP('',(#20194,#20195,#20196,#20197));
#4601=EDGE_LOOP('',(#20198,#20199,#20200,#20201));
#4602=EDGE_LOOP('',(#20202,#20203,#20204));
#4603=EDGE_LOOP('',(#20205,#20206,#20207));
#4604=EDGE_LOOP('',(#20208,#20209,#20210));
#4605=EDGE_LOOP('',(#20211,#20212,#20213,#20214));
#4606=EDGE_LOOP('',(#20215,#20216,#20217));
#4607=EDGE_LOOP('',(#20218,#20219,#20220));
#4608=EDGE_LOOP('',(#20221,#20222,#20223));
#4609=EDGE_LOOP('',(#20224));
#4610=EDGE_LOOP('',(#20225,#20226,#20227,#20228,#20229,#20230));
#4611=EDGE_LOOP('',(#20231,#20232,#20233,#20234));
#4612=EDGE_LOOP('',(#20235,#20236,#20237,#20238,#20239,#20240));
#4613=EDGE_LOOP('',(#20241));
#4614=EDGE_LOOP('',(#20242,#20243,#20244,#20245,#20246,#20247));
#4615=EDGE_LOOP('',(#20248,#20249,#20250,#20251));
#4616=EDGE_LOOP('',(#20252,#20253,#20254,#20255));
#4617=EDGE_LOOP('',(#20256));
#4618=EDGE_LOOP('',(#20257));
#4619=EDGE_LOOP('',(#20258));
#4620=EDGE_LOOP('',(#20259,#20260,#20261,#20262));
#4621=EDGE_LOOP('',(#20263,#20264,#20265,#20266));
#4622=EDGE_LOOP('',(#20267,#20268,#20269,#20270));
#4623=EDGE_LOOP('',(#20271,#20272,#20273,#20274));
#4624=EDGE_LOOP('',(#20275,#20276,#20277,#20278,#20279,#20280,#20281,#20282));
#4625=EDGE_LOOP('',(#20283));
#4626=EDGE_LOOP('',(#20284));
#4627=EDGE_LOOP('',(#20285,#20286,#20287,#20288));
#4628=EDGE_LOOP('',(#20289,#20290,#20291,#20292));
#4629=EDGE_LOOP('',(#20293,#20294,#20295,#20296,#20297,#20298,#20299));
#4630=EDGE_LOOP('',(#20300,#20301,#20302,#20303,#20304));
#4631=EDGE_LOOP('',(#20305,#20306,#20307,#20308));
#4632=EDGE_LOOP('',(#20309,#20310,#20311));
#4633=EDGE_LOOP('',(#20312,#20313,#20314,#20315));
#4634=EDGE_LOOP('',(#20316,#20317,#20318,#20319,#20320));
#4635=EDGE_LOOP('',(#20321,#20322,#20323,#20324));
#4636=EDGE_LOOP('',(#20325));
#4637=EDGE_LOOP('',(#20326,#20327,#20328,#20329));
#4638=EDGE_LOOP('',(#20330));
#4639=EDGE_LOOP('',(#20331));
#4640=EDGE_LOOP('',(#20332,#20333,#20334,#20335));
#4641=EDGE_LOOP('',(#20336,#20337,#20338,#20339));
#4642=EDGE_LOOP('',(#20340,#20341,#20342,#20343,#20344,#20345));
#4643=EDGE_LOOP('',(#20346,#20347,#20348,#20349,#20350));
#4644=EDGE_LOOP('',(#20351,#20352,#20353,#20354));
#4645=EDGE_LOOP('',(#20355,#20356,#20357,#20358,#20359));
#4646=EDGE_LOOP('',(#20360,#20361,#20362,#20363,#20364,#20365));
#4647=EDGE_LOOP('',(#20366,#20367,#20368,#20369,#20370));
#4648=EDGE_LOOP('',(#20371,#20372,#20373,#20374));
#4649=EDGE_LOOP('',(#20375,#20376,#20377,#20378,#20379));
#4650=EDGE_LOOP('',(#20380,#20381,#20382,#20383,#20384,#20385));
#4651=EDGE_LOOP('',(#20386,#20387,#20388,#20389));
#4652=EDGE_LOOP('',(#20390,#20391,#20392,#20393,#20394));
#4653=EDGE_LOOP('',(#20395,#20396,#20397,#20398,#20399,#20400));
#4654=EDGE_LOOP('',(#20401,#20402,#20403,#20404,#20405,#20406));
#4655=EDGE_LOOP('',(#20407,#20408,#20409,#20410,#20411));
#4656=EDGE_LOOP('',(#20412,#20413,#20414,#20415));
#4657=EDGE_LOOP('',(#20416,#20417,#20418,#20419,#20420));
#4658=EDGE_LOOP('',(#20421,#20422,#20423,#20424,#20425,#20426));
#4659=EDGE_LOOP('',(#20427,#20428,#20429,#20430));
#4660=EDGE_LOOP('',(#20431,#20432,#20433,#20434,#20435,#20436));
#4661=EDGE_LOOP('',(#20437,#20438,#20439,#20440,#20441));
#4662=EDGE_LOOP('',(#20442,#20443,#20444,#20445,#20446,#20447));
#4663=EDGE_LOOP('',(#20448,#20449,#20450,#20451,#20452));
#4664=EDGE_LOOP('',(#20453,#20454,#20455,#20456,#20457,#20458));
#4665=EDGE_LOOP('',(#20459,#20460,#20461,#20462));
#4666=EDGE_LOOP('',(#20463,#20464,#20465,#20466,#20467,#20468));
#4667=EDGE_LOOP('',(#20469,#20470,#20471,#20472,#20473));
#4668=EDGE_LOOP('',(#20474,#20475,#20476,#20477,#20478,#20479));
#4669=EDGE_LOOP('',(#20480,#20481,#20482,#20483));
#4670=EDGE_LOOP('',(#20484,#20485,#20486,#20487,#20488));
#4671=EDGE_LOOP('',(#20489,#20490,#20491,#20492,#20493,#20494));
#4672=EDGE_LOOP('',(#20495,#20496,#20497,#20498,#20499,#20500));
#4673=EDGE_LOOP('',(#20501,#20502,#20503,#20504));
#4674=EDGE_LOOP('',(#20505,#20506,#20507,#20508,#20509,#20510));
#4675=EDGE_LOOP('',(#20511,#20512,#20513,#20514,#20515));
#4676=EDGE_LOOP('',(#20516,#20517,#20518,#20519,#20520,#20521));
#4677=EDGE_LOOP('',(#20522,#20523,#20524,#20525,#20526));
#4678=EDGE_LOOP('',(#20527,#20528,#20529,#20530,#20531,#20532));
#4679=EDGE_LOOP('',(#20533,#20534,#20535,#20536));
#4680=EDGE_LOOP('',(#20537,#20538,#20539,#20540,#20541,#20542));
#4681=EDGE_LOOP('',(#20543,#20544,#20545,#20546,#20547));
#4682=EDGE_LOOP('',(#20548,#20549,#20550,#20551,#20552,#20553));
#4683=EDGE_LOOP('',(#20554,#20555,#20556,#20557));
#4684=EDGE_LOOP('',(#20558,#20559,#20560,#20561,#20562));
#4685=EDGE_LOOP('',(#20563,#20564,#20565,#20566,#20567,#20568));
#4686=EDGE_LOOP('',(#20569,#20570,#20571,#20572,#20573,#20574));
#4687=EDGE_LOOP('',(#20575,#20576,#20577,#20578,#20579));
#4688=EDGE_LOOP('',(#20580,#20581,#20582,#20583,#20584,#20585));
#4689=EDGE_LOOP('',(#20586,#20587,#20588,#20589));
#4690=EDGE_LOOP('',(#20590,#20591,#20592,#20593,#20594,#20595));
#4691=EDGE_LOOP('',(#20596,#20597,#20598,#20599,#20600));
#4692=EDGE_LOOP('',(#20601,#20602,#20603,#20604,#20605,#20606));
#4693=EDGE_LOOP('',(#20607,#20608,#20609,#20610));
#4694=EDGE_LOOP('',(#20611,#20612,#20613,#20614,#20615));
#4695=EDGE_LOOP('',(#20616,#20617,#20618,#20619,#20620,#20621));
#4696=EDGE_LOOP('',(#20622,#20623,#20624,#20625,#20626,#20627));
#4697=EDGE_LOOP('',(#20628,#20629,#20630,#20631));
#4698=EDGE_LOOP('',(#20632,#20633,#20634,#20635,#20636));
#4699=EDGE_LOOP('',(#20637,#20638,#20639,#20640,#20641,#20642));
#4700=EDGE_LOOP('',(#20643,#20644,#20645,#20646,#20647,#20648));
#4701=EDGE_LOOP('',(#20649,#20650,#20651,#20652,#20653));
#4702=EDGE_LOOP('',(#20654,#20655,#20656,#20657,#20658,#20659));
#4703=EDGE_LOOP('',(#20660,#20661,#20662,#20663));
#4704=EDGE_LOOP('',(#20664,#20665,#20666,#20667,#20668,#20669));
#4705=EDGE_LOOP('',(#20670,#20671,#20672,#20673,#20674));
#4706=EDGE_LOOP('',(#20675,#20676,#20677,#20678,#20679,#20680));
#4707=EDGE_LOOP('',(#20681,#20682,#20683,#20684,#20685));
#4708=EDGE_LOOP('',(#20686,#20687,#20688,#20689,#20690,#20691));
#4709=EDGE_LOOP('',(#20692,#20693,#20694,#20695));
#4710=EDGE_LOOP('',(#20696,#20697,#20698,#20699,#20700,#20701));
#4711=EDGE_LOOP('',(#20702,#20703,#20704,#20705,#20706));
#4712=EDGE_LOOP('',(#20707,#20708,#20709,#20710,#20711,#20712));
#4713=EDGE_LOOP('',(#20713,#20714,#20715,#20716,#20717));
#4714=EDGE_LOOP('',(#20718,#20719,#20720,#20721));
#4715=EDGE_LOOP('',(#20722,#20723,#20724,#20725,#20726));
#4716=EDGE_LOOP('',(#20727,#20728,#20729,#20730,#20731,#20732));
#4717=EDGE_LOOP('',(#20733,#20734,#20735,#20736,#20737));
#4718=EDGE_LOOP('',(#20738,#20739,#20740,#20741,#20742,#20743));
#4719=EDGE_LOOP('',(#20744,#20745,#20746,#20747));
#4720=EDGE_LOOP('',(#20748,#20749,#20750,#20751,#20752,#20753));
#4721=EDGE_LOOP('',(#20754,#20755,#20756,#20757,#20758));
#4722=EDGE_LOOP('',(#20759,#20760,#20761,#20762,#20763,#20764));
#4723=EDGE_LOOP('',(#20765,#20766,#20767,#20768,#20769));
#4724=EDGE_LOOP('',(#20770,#20771,#20772,#20773,#20774,#20775));
#4725=EDGE_LOOP('',(#20776,#20777,#20778,#20779));
#4726=EDGE_LOOP('',(#20780,#20781,#20782,#20783,#20784,#20785));
#4727=EDGE_LOOP('',(#20786,#20787,#20788,#20789,#20790));
#4728=EDGE_LOOP('',(#20791,#20792,#20793,#20794,#20795,#20796));
#4729=EDGE_LOOP('',(#20797,#20798,#20799,#20800,#20801));
#4730=EDGE_LOOP('',(#20802,#20803,#20804,#20805));
#4731=EDGE_LOOP('',(#20806,#20807,#20808,#20809,#20810));
#4732=EDGE_LOOP('',(#20811,#20812,#20813,#20814));
#4733=EDGE_LOOP('',(#20815,#20816,#20817,#20818));
#4734=EDGE_LOOP('',(#20819));
#4735=EDGE_LOOP('',(#20820,#20821,#20822,#20823,#20824,#20825));
#4736=EDGE_LOOP('',(#20826,#20827,#20828,#20829,#20830,#20831));
#4737=EDGE_LOOP('',(#20832,#20833,#20834,#20835));
#4738=EDGE_LOOP('',(#20836,#20837,#20838,#20839,#20840,#20841));
#4739=EDGE_LOOP('',(#20842,#20843,#20844,#20845,#20846,#20847));
#4740=EDGE_LOOP('',(#20848,#20849,#20850,#20851));
#4741=EDGE_LOOP('',(#20852,#20853,#20854,#20855,#20856,#20857));
#4742=EDGE_LOOP('',(#20858,#20859,#20860,#20861,#20862,#20863));
#4743=EDGE_LOOP('',(#20864,#20865,#20866,#20867,#20868,#20869));
#4744=EDGE_LOOP('',(#20870,#20871,#20872,#20873));
#4745=EDGE_LOOP('',(#20874,#20875,#20876,#20877,#20878,#20879));
#4746=EDGE_LOOP('',(#20880,#20881,#20882,#20883,#20884));
#4747=EDGE_LOOP('',(#20885,#20886,#20887,#20888,#20889,#20890));
#4748=EDGE_LOOP('',(#20891,#20892,#20893,#20894));
#4749=EDGE_LOOP('',(#20895,#20896,#20897,#20898,#20899,#20900));
#4750=EDGE_LOOP('',(#20901,#20902,#20903,#20904,#20905));
#4751=EDGE_LOOP('',(#20906,#20907,#20908,#20909,#20910,#20911));
#4752=EDGE_LOOP('',(#20912,#20913,#20914,#20915,#20916));
#4753=EDGE_LOOP('',(#20917,#20918,#20919,#20920,#20921,#20922));
#4754=EDGE_LOOP('',(#20923,#20924,#20925,#20926));
#4755=EDGE_LOOP('',(#20927,#20928,#20929,#20930,#20931,#20932));
#4756=EDGE_LOOP('',(#20933,#20934,#20935,#20936,#20937));
#4757=EDGE_LOOP('',(#20938,#20939,#20940,#20941,#20942,#20943));
#4758=EDGE_LOOP('',(#20944,#20945,#20946,#20947,#20948));
#4759=EDGE_LOOP('',(#20949,#20950,#20951,#20952,#20953,#20954));
#4760=EDGE_LOOP('',(#20955,#20956,#20957,#20958));
#4761=EDGE_LOOP('',(#20959,#20960,#20961,#20962,#20963,#20964));
#4762=EDGE_LOOP('',(#20965,#20966,#20967,#20968,#20969));
#4763=EDGE_LOOP('',(#20970,#20971,#20972,#20973,#20974,#20975));
#4764=EDGE_LOOP('',(#20976,#20977,#20978,#20979,#20980));
#4765=EDGE_LOOP('',(#20981,#20982,#20983,#20984,#20985,#20986));
#4766=EDGE_LOOP('',(#20987,#20988,#20989,#20990));
#4767=EDGE_LOOP('',(#20991,#20992,#20993,#20994,#20995,#20996));
#4768=EDGE_LOOP('',(#20997,#20998,#20999,#21000,#21001));
#4769=EDGE_LOOP('',(#21002,#21003,#21004,#21005,#21006,#21007));
#4770=EDGE_LOOP('',(#21008,#21009,#21010,#21011));
#4771=EDGE_LOOP('',(#21012,#21013,#21014,#21015,#21016));
#4772=EDGE_LOOP('',(#21017,#21018,#21019,#21020,#21021,#21022));
#4773=EDGE_LOOP('',(#21023,#21024,#21025,#21026));
#4774=EDGE_LOOP('',(#21027,#21028,#21029,#21030));
#4775=EDGE_LOOP('',(#21031,#21032,#21033,#21034));
#4776=EDGE_LOOP('',(#21035,#21036,#21037,#21038));
#4777=EDGE_LOOP('',(#21039,#21040,#21041,#21042));
#4778=EDGE_LOOP('',(#21043,#21044,#21045,#21046));
#4779=EDGE_LOOP('',(#21047,#21048,#21049,#21050));
#4780=EDGE_LOOP('',(#21051,#21052,#21053,#21054));
#4781=EDGE_LOOP('',(#21055,#21056,#21057,#21058));
#4782=EDGE_LOOP('',(#21059,#21060,#21061,#21062));
#4783=EDGE_LOOP('',(#21063,#21064,#21065,#21066,#21067,#21068,#21069,#21070,
#21071,#21072,#21073,#21074,#21075,#21076,#21077,#21078,#21079,#21080,#21081,
#21082,#21083,#21084,#21085,#21086,#21087,#21088,#21089,#21090,#21091,#21092,
#21093,#21094,#21095,#21096,#21097,#21098,#21099,#21100,#21101,#21102,#21103,
#21104,#21105,#21106,#21107,#21108,#21109,#21110,#21111,#21112,#21113,#21114,
#21115,#21116,#21117,#21118,#21119,#21120,#21121,#21122,#21123,#21124,#21125,
#21126,#21127,#21128,#21129,#21130,#21131,#21132,#21133,#21134,#21135,#21136,
#21137,#21138,#21139,#21140,#21141,#21142,#21143,#21144,#21145,#21146,#21147,
#21148,#21149,#21150,#21151,#21152,#21153,#21154,#21155,#21156,#21157,#21158,
#21159,#21160,#21161,#21162,#21163,#21164,#21165,#21166,#21167,#21168,#21169,
#21170,#21171,#21172,#21173,#21174,#21175,#21176,#21177,#21178,#21179,#21180,
#21181,#21182,#21183,#21184,#21185,#21186,#21187,#21188,#21189,#21190,#21191,
#21192,#21193,#21194));
#4784=EDGE_LOOP('',(#21195,#21196,#21197,#21198));
#4785=EDGE_LOOP('',(#21199,#21200,#21201,#21202));
#4786=EDGE_LOOP('',(#21203,#21204,#21205,#21206));
#4787=EDGE_LOOP('',(#21207,#21208,#21209,#21210));
#4788=EDGE_LOOP('',(#21211,#21212,#21213,#21214));
#4789=EDGE_LOOP('',(#21215,#21216,#21217,#21218));
#4790=EDGE_LOOP('',(#21219,#21220,#21221,#21222));
#4791=EDGE_LOOP('',(#21223,#21224,#21225,#21226));
#4792=EDGE_LOOP('',(#21227,#21228,#21229,#21230));
#4793=EDGE_LOOP('',(#21231,#21232,#21233,#21234));
#4794=EDGE_LOOP('',(#21235,#21236,#21237,#21238));
#4795=EDGE_LOOP('',(#21239,#21240,#21241,#21242));
#4796=EDGE_LOOP('',(#21243,#21244,#21245,#21246));
#4797=EDGE_LOOP('',(#21247,#21248,#21249,#21250));
#4798=EDGE_LOOP('',(#21251,#21252,#21253,#21254));
#4799=EDGE_LOOP('',(#21255,#21256,#21257,#21258));
#4800=EDGE_LOOP('',(#21259,#21260,#21261,#21262));
#4801=EDGE_LOOP('',(#21263,#21264,#21265,#21266));
#4802=EDGE_LOOP('',(#21267,#21268,#21269,#21270));
#4803=EDGE_LOOP('',(#21271,#21272,#21273,#21274,#21275));
#4804=EDGE_LOOP('',(#21276,#21277,#21278,#21279));
#4805=EDGE_LOOP('',(#21280,#21281,#21282,#21283,#21284,#21285));
#4806=EDGE_LOOP('',(#21286,#21287,#21288,#21289,#21290,#21291));
#4807=EDGE_LOOP('',(#21292,#21293,#21294,#21295,#21296,#21297));
#4808=EDGE_LOOP('',(#21298,#21299,#21300,#21301,#21302,#21303));
#4809=EDGE_LOOP('',(#21304,#21305,#21306,#21307,#21308));
#4810=EDGE_LOOP('',(#21309,#21310,#21311,#21312,#21313,#21314));
#4811=EDGE_LOOP('',(#21315,#21316,#21317,#21318,#21319));
#4812=EDGE_LOOP('',(#21320,#21321,#21322,#21323,#21324,#21325));
#4813=EDGE_LOOP('',(#21326,#21327,#21328,#21329));
#4814=EDGE_LOOP('',(#21330,#21331,#21332,#21333,#21334,#21335));
#4815=EDGE_LOOP('',(#21336,#21337,#21338,#21339,#21340));
#4816=EDGE_LOOP('',(#21341,#21342,#21343,#21344));
#4817=EDGE_LOOP('',(#21345,#21346,#21347,#21348));
#4818=EDGE_LOOP('',(#21349,#21350,#21351,#21352));
#4819=EDGE_LOOP('',(#21353,#21354,#21355,#21356));
#4820=EDGE_LOOP('',(#21357,#21358,#21359,#21360));
#4821=EDGE_LOOP('',(#21361,#21362,#21363,#21364));
#4822=EDGE_LOOP('',(#21365,#21366,#21367,#21368));
#4823=EDGE_LOOP('',(#21369,#21370,#21371,#21372));
#4824=EDGE_LOOP('',(#21373,#21374,#21375,#21376));
#4825=EDGE_LOOP('',(#21377,#21378,#21379,#21380));
#4826=EDGE_LOOP('',(#21381,#21382,#21383,#21384));
#4827=EDGE_LOOP('',(#21385,#21386,#21387,#21388));
#4828=EDGE_LOOP('',(#21389,#21390,#21391,#21392,#21393));
#4829=EDGE_LOOP('',(#21394,#21395,#21396,#21397));
#4830=EDGE_LOOP('',(#21398,#21399,#21400,#21401));
#4831=EDGE_LOOP('',(#21402,#21403,#21404,#21405));
#4832=EDGE_LOOP('',(#21406,#21407,#21408,#21409));
#4833=EDGE_LOOP('',(#21410,#21411,#21412,#21413));
#4834=EDGE_LOOP('',(#21414,#21415,#21416,#21417));
#4835=EDGE_LOOP('',(#21418,#21419,#21420,#21421));
#4836=EDGE_LOOP('',(#21422,#21423,#21424,#21425));
#4837=EDGE_LOOP('',(#21426,#21427,#21428,#21429));
#4838=EDGE_LOOP('',(#21430,#21431,#21432,#21433));
#4839=EDGE_LOOP('',(#21434,#21435,#21436,#21437));
#4840=EDGE_LOOP('',(#21438,#21439,#21440,#21441));
#4841=EDGE_LOOP('',(#21442,#21443,#21444,#21445));
#4842=EDGE_LOOP('',(#21446,#21447,#21448,#21449));
#4843=EDGE_LOOP('',(#21450,#21451,#21452,#21453));
#4844=EDGE_LOOP('',(#21454,#21455,#21456,#21457));
#4845=EDGE_LOOP('',(#21458,#21459,#21460,#21461,#21462,#21463));
#4846=EDGE_LOOP('',(#21464,#21465,#21466,#21467,#21468));
#4847=EDGE_LOOP('',(#21469,#21470,#21471,#21472,#21473,#21474));
#4848=EDGE_LOOP('',(#21475,#21476,#21477,#21478));
#4849=EDGE_LOOP('',(#21479,#21480,#21481,#21482,#21483,#21484));
#4850=EDGE_LOOP('',(#21485,#21486,#21487,#21488,#21489));
#4851=EDGE_LOOP('',(#21490,#21491,#21492,#21493,#21494,#21495));
#4852=EDGE_LOOP('',(#21496,#21497,#21498,#21499,#21500));
#4853=EDGE_LOOP('',(#21501,#21502,#21503,#21504,#21505,#21506));
#4854=EDGE_LOOP('',(#21507,#21508,#21509,#21510));
#4855=EDGE_LOOP('',(#21511,#21512,#21513,#21514,#21515,#21516));
#4856=EDGE_LOOP('',(#21517,#21518,#21519,#21520,#21521));
#4857=EDGE_LOOP('',(#21522,#21523,#21524,#21525,#21526,#21527));
#4858=EDGE_LOOP('',(#21528,#21529,#21530,#21531,#21532));
#4859=EDGE_LOOP('',(#21533,#21534,#21535,#21536,#21537,#21538));
#4860=EDGE_LOOP('',(#21539,#21540,#21541,#21542));
#4861=EDGE_LOOP('',(#21543,#21544,#21545,#21546,#21547,#21548));
#4862=EDGE_LOOP('',(#21549,#21550,#21551,#21552,#21553));
#4863=EDGE_LOOP('',(#21554,#21555,#21556,#21557,#21558,#21559));
#4864=EDGE_LOOP('',(#21560,#21561,#21562,#21563));
#4865=EDGE_LOOP('',(#21564,#21565,#21566,#21567,#21568));
#4866=EDGE_LOOP('',(#21569,#21570,#21571,#21572,#21573,#21574));
#4867=EDGE_LOOP('',(#21575,#21576,#21577,#21578,#21579,#21580));
#4868=EDGE_LOOP('',(#21581,#21582,#21583,#21584));
#4869=EDGE_LOOP('',(#21585,#21586,#21587,#21588,#21589));
#4870=EDGE_LOOP('',(#21590,#21591,#21592,#21593,#21594,#21595));
#4871=EDGE_LOOP('',(#21596,#21597,#21598,#21599,#21600,#21601));
#4872=EDGE_LOOP('',(#21602,#21603,#21604,#21605,#21606));
#4873=EDGE_LOOP('',(#21607,#21608,#21609,#21610,#21611,#21612));
#4874=EDGE_LOOP('',(#21613,#21614,#21615,#21616));
#4875=EDGE_LOOP('',(#21617,#21618,#21619,#21620,#21621,#21622));
#4876=EDGE_LOOP('',(#21623,#21624,#21625,#21626,#21627));
#4877=EDGE_LOOP('',(#21628,#21629,#21630,#21631,#21632,#21633));
#4878=EDGE_LOOP('',(#21634,#21635,#21636,#21637,#21638));
#4879=EDGE_LOOP('',(#21639,#21640,#21641,#21642,#21643,#21644));
#4880=EDGE_LOOP('',(#21645,#21646,#21647,#21648));
#4881=EDGE_LOOP('',(#21649,#21650,#21651,#21652,#21653,#21654));
#4882=EDGE_LOOP('',(#21655,#21656,#21657,#21658,#21659));
#4883=EDGE_LOOP('',(#21660,#21661,#21662,#21663,#21664,#21665));
#4884=EDGE_LOOP('',(#21666,#21667,#21668,#21669,#21670));
#4885=EDGE_LOOP('',(#21671,#21672,#21673,#21674));
#4886=EDGE_LOOP('',(#21675,#21676,#21677,#21678,#21679));
#4887=EDGE_LOOP('',(#21680,#21681,#21682,#21683));
#4888=EDGE_LOOP('',(#21684,#21685,#21686,#21687));
#4889=EDGE_LOOP('',(#21688,#21689,#21690,#21691));
#4890=EDGE_LOOP('',(#21692,#21693,#21694,#21695));
#4891=EDGE_LOOP('',(#21696,#21697,#21698,#21699));
#4892=EDGE_LOOP('',(#21700,#21701,#21702,#21703));
#4893=EDGE_LOOP('',(#21704,#21705,#21706,#21707));
#4894=EDGE_LOOP('',(#21708,#21709,#21710,#21711,#21712));
#4895=EDGE_LOOP('',(#21713,#21714,#21715,#21716));
#4896=EDGE_LOOP('',(#21717,#21718,#21719,#21720));
#4897=EDGE_LOOP('',(#21721,#21722,#21723,#21724));
#4898=EDGE_LOOP('',(#21725,#21726,#21727,#21728));
#4899=EDGE_LOOP('',(#21729,#21730,#21731,#21732));
#4900=EDGE_LOOP('',(#21733,#21734,#21735,#21736));
#4901=EDGE_LOOP('',(#21737,#21738,#21739,#21740));
#4902=EDGE_LOOP('',(#21741,#21742,#21743,#21744));
#4903=EDGE_LOOP('',(#21745,#21746,#21747,#21748));
#4904=EDGE_LOOP('',(#21749,#21750,#21751,#21752));
#4905=EDGE_LOOP('',(#21753,#21754,#21755,#21756));
#4906=EDGE_LOOP('',(#21757,#21758,#21759,#21760));
#4907=EDGE_LOOP('',(#21761,#21762,#21763,#21764));
#4908=EDGE_LOOP('',(#21765,#21766,#21767,#21768));
#4909=EDGE_LOOP('',(#21769,#21770,#21771,#21772));
#4910=EDGE_LOOP('',(#21773,#21774,#21775,#21776));
#4911=EDGE_LOOP('',(#21777,#21778,#21779,#21780));
#4912=EDGE_LOOP('',(#21781,#21782,#21783,#21784));
#4913=EDGE_LOOP('',(#21785,#21786,#21787,#21788));
#4914=EDGE_LOOP('',(#21789,#21790,#21791,#21792));
#4915=EDGE_LOOP('',(#21793,#21794,#21795,#21796));
#4916=EDGE_LOOP('',(#21797,#21798,#21799,#21800));
#4917=EDGE_LOOP('',(#21801,#21802,#21803,#21804));
#4918=EDGE_LOOP('',(#21805,#21806,#21807,#21808));
#4919=EDGE_LOOP('',(#21809,#21810,#21811,#21812,#21813,#21814));
#4920=EDGE_LOOP('',(#21815,#21816,#21817,#21818,#21819));
#4921=EDGE_LOOP('',(#21820,#21821,#21822,#21823,#21824,#21825));
#4922=EDGE_LOOP('',(#21826,#21827,#21828,#21829));
#4923=EDGE_LOOP('',(#21830,#21831,#21832,#21833,#21834,#21835));
#4924=EDGE_LOOP('',(#21836,#21837,#21838,#21839,#21840));
#4925=EDGE_LOOP('',(#21841,#21842,#21843,#21844,#21845,#21846));
#4926=EDGE_LOOP('',(#21847,#21848,#21849,#21850,#21851));
#4927=EDGE_LOOP('',(#21852,#21853,#21854,#21855,#21856,#21857));
#4928=EDGE_LOOP('',(#21858,#21859,#21860,#21861));
#4929=EDGE_LOOP('',(#21862,#21863,#21864,#21865,#21866,#21867));
#4930=EDGE_LOOP('',(#21868,#21869,#21870,#21871,#21872));
#4931=EDGE_LOOP('',(#21873,#21874,#21875,#21876,#21877,#21878));
#4932=EDGE_LOOP('',(#21879,#21880,#21881,#21882,#21883));
#4933=EDGE_LOOP('',(#21884,#21885,#21886,#21887,#21888,#21889));
#4934=EDGE_LOOP('',(#21890,#21891,#21892,#21893));
#4935=EDGE_LOOP('',(#21894,#21895,#21896,#21897,#21898,#21899));
#4936=EDGE_LOOP('',(#21900,#21901,#21902,#21903,#21904));
#4937=EDGE_LOOP('',(#21905,#21906,#21907,#21908,#21909,#21910));
#4938=EDGE_LOOP('',(#21911,#21912,#21913,#21914,#21915));
#4939=EDGE_LOOP('',(#21916,#21917,#21918,#21919,#21920,#21921));
#4940=EDGE_LOOP('',(#21922,#21923,#21924,#21925));
#4941=EDGE_LOOP('',(#21926,#21927,#21928,#21929,#21930,#21931));
#4942=EDGE_LOOP('',(#21932,#21933,#21934,#21935,#21936));
#4943=EDGE_LOOP('',(#21937,#21938,#21939,#21940,#21941,#21942));
#4944=EDGE_LOOP('',(#21943,#21944,#21945,#21946,#21947));
#4945=EDGE_LOOP('',(#21948,#21949,#21950,#21951,#21952,#21953));
#4946=EDGE_LOOP('',(#21954,#21955,#21956,#21957));
#4947=EDGE_LOOP('',(#21958,#21959,#21960,#21961,#21962,#21963));
#4948=EDGE_LOOP('',(#21964,#21965,#21966,#21967,#21968));
#4949=EDGE_LOOP('',(#21969,#21970,#21971,#21972,#21973,#21974));
#4950=EDGE_LOOP('',(#21975,#21976,#21977,#21978,#21979));
#4951=EDGE_LOOP('',(#21980,#21981,#21982,#21983,#21984,#21985));
#4952=EDGE_LOOP('',(#21986,#21987,#21988,#21989));
#4953=EDGE_LOOP('',(#21990,#21991,#21992,#21993,#21994,#21995));
#4954=EDGE_LOOP('',(#21996,#21997,#21998,#21999,#22000));
#4955=EDGE_LOOP('',(#22001,#22002,#22003,#22004,#22005,#22006));
#4956=EDGE_LOOP('',(#22007,#22008,#22009,#22010,#22011));
#4957=EDGE_LOOP('',(#22012,#22013,#22014,#22015));
#4958=EDGE_LOOP('',(#22016,#22017,#22018,#22019,#22020));
#4959=EDGE_LOOP('',(#22021,#22022,#22023,#22024));
#4960=EDGE_LOOP('',(#22025,#22026,#22027,#22028));
#4961=EDGE_LOOP('',(#22029,#22030,#22031,#22032));
#4962=EDGE_LOOP('',(#22033,#22034,#22035,#22036));
#4963=EDGE_LOOP('',(#22037,#22038,#22039,#22040));
#4964=EDGE_LOOP('',(#22041,#22042,#22043,#22044));
#4965=EDGE_LOOP('',(#22045,#22046,#22047,#22048));
#4966=EDGE_LOOP('',(#22049,#22050,#22051,#22052));
#4967=EDGE_LOOP('',(#22053,#22054,#22055,#22056));
#4968=EDGE_LOOP('',(#22057,#22058,#22059,#22060));
#4969=EDGE_LOOP('',(#22061,#22062,#22063,#22064));
#4970=EDGE_LOOP('',(#22065,#22066,#22067,#22068));
#4971=EDGE_LOOP('',(#22069,#22070,#22071,#22072));
#4972=EDGE_LOOP('',(#22073,#22074,#22075,#22076));
#4973=EDGE_LOOP('',(#22077,#22078,#22079,#22080));
#4974=EDGE_LOOP('',(#22081,#22082,#22083,#22084));
#4975=EDGE_LOOP('',(#22085,#22086,#22087,#22088));
#4976=EDGE_LOOP('',(#22089,#22090,#22091,#22092));
#4977=EDGE_LOOP('',(#22093,#22094,#22095,#22096));
#4978=EDGE_LOOP('',(#22097,#22098,#22099,#22100));
#4979=EDGE_LOOP('',(#22101,#22102,#22103,#22104));
#4980=EDGE_LOOP('',(#22105,#22106,#22107,#22108));
#4981=EDGE_LOOP('',(#22109,#22110,#22111,#22112));
#4982=EDGE_LOOP('',(#22113,#22114,#22115,#22116));
#4983=EDGE_LOOP('',(#22117,#22118,#22119,#22120));
#4984=EDGE_LOOP('',(#22121,#22122,#22123,#22124));
#4985=EDGE_LOOP('',(#22125,#22126,#22127,#22128,#22129));
#4986=EDGE_LOOP('',(#22130,#22131,#22132,#22133,#22134));
#4987=EDGE_LOOP('',(#22135,#22136,#22137,#22138));
#4988=EDGE_LOOP('',(#22139,#22140,#22141,#22142,#22143));
#4989=EDGE_LOOP('',(#22144,#22145,#22146,#22147,#22148,#22149,#22150,#22151,
#22152,#22153,#22154,#22155,#22156,#22157,#22158,#22159,#22160,#22161,#22162,
#22163,#22164,#22165,#22166,#22167,#22168,#22169,#22170,#22171,#22172,#22173,
#22174,#22175,#22176,#22177,#22178,#22179,#22180,#22181,#22182,#22183,#22184,
#22185,#22186,#22187,#22188,#22189,#22190,#22191,#22192,#22193,#22194,#22195,
#22196,#22197,#22198,#22199,#22200,#22201,#22202,#22203,#22204,#22205,#22206,
#22207,#22208,#22209,#22210,#22211,#22212,#22213,#22214,#22215,#22216,#22217,
#22218,#22219,#22220,#22221,#22222,#22223,#22224,#22225,#22226,#22227,#22228,
#22229,#22230,#22231,#22232,#22233,#22234,#22235,#22236,#22237,#22238,#22239,
#22240,#22241,#22242,#22243,#22244,#22245,#22246,#22247,#22248,#22249,#22250,
#22251,#22252,#22253,#22254,#22255,#22256,#22257,#22258,#22259,#22260,#22261,
#22262,#22263,#22264,#22265,#22266,#22267,#22268,#22269,#22270,#22271,#22272,
#22273,#22274,#22275));
#4990=EDGE_LOOP('',(#22276));
#4991=EDGE_LOOP('',(#22277,#22278,#22279,#22280,#22281,#22282));
#4992=EDGE_LOOP('',(#22283,#22284,#22285,#22286,#22287));
#4993=EDGE_LOOP('',(#22288,#22289,#22290,#22291));
#4994=EDGE_LOOP('',(#22292,#22293,#22294,#22295,#22296));
#4995=EDGE_LOOP('',(#22297,#22298,#22299,#22300,#22301,#22302));
#4996=EDGE_LOOP('',(#22303,#22304,#22305,#22306,#22307));
#4997=EDGE_LOOP('',(#22308,#22309,#22310,#22311));
#4998=EDGE_LOOP('',(#22312,#22313,#22314,#22315,#22316));
#4999=EDGE_LOOP('',(#22317,#22318,#22319,#22320,#22321,#22322));
#5000=EDGE_LOOP('',(#22323,#22324,#22325,#22326,#22327));
#5001=EDGE_LOOP('',(#22328,#22329,#22330,#22331));
#5002=EDGE_LOOP('',(#22332,#22333,#22334,#22335,#22336));
#5003=EDGE_LOOP('',(#22337,#22338,#22339,#22340,#22341,#22342));
#5004=EDGE_LOOP('',(#22343,#22344,#22345,#22346));
#5005=EDGE_LOOP('',(#22347,#22348,#22349,#22350,#22351));
#5006=EDGE_LOOP('',(#22352,#22353,#22354,#22355,#22356,#22357));
#5007=EDGE_LOOP('',(#22358,#22359,#22360,#22361,#22362));
#5008=EDGE_LOOP('',(#22363,#22364,#22365,#22366));
#5009=EDGE_LOOP('',(#22367,#22368,#22369,#22370,#22371));
#5010=EDGE_LOOP('',(#22372,#22373,#22374,#22375,#22376,#22377));
#5011=EDGE_LOOP('',(#22378,#22379,#22380,#22381,#22382));
#5012=EDGE_LOOP('',(#22383,#22384,#22385,#22386));
#5013=EDGE_LOOP('',(#22387,#22388,#22389,#22390));
#5014=EDGE_LOOP('',(#22391,#22392,#22393,#22394,#22395));
#5015=EDGE_LOOP('',(#22396,#22397,#22398,#22399,#22400));
#5016=EDGE_LOOP('',(#22401,#22402,#22403,#22404));
#5017=EDGE_LOOP('',(#22405,#22406,#22407,#22408,#22409));
#5018=EDGE_LOOP('',(#22410,#22411,#22412,#22413,#22414,#22415));
#5019=EDGE_LOOP('',(#22416,#22417,#22418,#22419,#22420));
#5020=EDGE_LOOP('',(#22421,#22422,#22423,#22424));
#5021=EDGE_LOOP('',(#22425,#22426,#22427,#22428,#22429));
#5022=EDGE_LOOP('',(#22430,#22431,#22432,#22433,#22434,#22435));
#5023=EDGE_LOOP('',(#22436,#22437,#22438,#22439,#22440));
#5024=EDGE_LOOP('',(#22441,#22442,#22443,#22444));
#5025=EDGE_LOOP('',(#22445,#22446,#22447,#22448,#22449));
#5026=EDGE_LOOP('',(#22450,#22451,#22452,#22453,#22454,#22455));
#5027=EDGE_LOOP('',(#22456,#22457,#22458,#22459,#22460));
#5028=EDGE_LOOP('',(#22461,#22462,#22463,#22464));
#5029=EDGE_LOOP('',(#22465,#22466,#22467,#22468,#22469));
#5030=EDGE_LOOP('',(#22470,#22471,#22472,#22473,#22474,#22475));
#5031=EDGE_LOOP('',(#22476,#22477,#22478,#22479,#22480));
#5032=EDGE_LOOP('',(#22481,#22482,#22483,#22484));
#5033=EDGE_LOOP('',(#22485,#22486,#22487,#22488,#22489));
#5034=EDGE_LOOP('',(#22490,#22491,#22492,#22493,#22494,#22495));
#5035=EDGE_LOOP('',(#22496,#22497,#22498,#22499,#22500));
#5036=EDGE_LOOP('',(#22501,#22502,#22503,#22504));
#5037=EDGE_LOOP('',(#22505,#22506,#22507,#22508,#22509,#22510));
#5038=EDGE_LOOP('',(#22511,#22512,#22513,#22514,#22515));
#5039=EDGE_LOOP('',(#22516,#22517,#22518,#22519));
#5040=EDGE_LOOP('',(#22520,#22521,#22522,#22523,#22524));
#5041=EDGE_LOOP('',(#22525,#22526,#22527,#22528,#22529,#22530));
#5042=EDGE_LOOP('',(#22531,#22532,#22533,#22534,#22535));
#5043=EDGE_LOOP('',(#22536,#22537,#22538,#22539));
#5044=EDGE_LOOP('',(#22540,#22541,#22542,#22543,#22544));
#5045=EDGE_LOOP('',(#22545,#22546,#22547,#22548,#22549,#22550));
#5046=EDGE_LOOP('',(#22551,#22552,#22553,#22554));
#5047=EDGE_LOOP('',(#22555,#22556,#22557,#22558,#22559));
#5048=EDGE_LOOP('',(#22560,#22561,#22562,#22563,#22564,#22565));
#5049=EDGE_LOOP('',(#22566,#22567,#22568,#22569,#22570));
#5050=EDGE_LOOP('',(#22571,#22572,#22573,#22574));
#5051=EDGE_LOOP('',(#22575,#22576,#22577,#22578,#22579));
#5052=EDGE_LOOP('',(#22580,#22581,#22582,#22583,#22584,#22585));
#5053=EDGE_LOOP('',(#22586,#22587,#22588,#22589,#22590));
#5054=EDGE_LOOP('',(#22591,#22592,#22593,#22594));
#5055=EDGE_LOOP('',(#22595,#22596,#22597,#22598,#22599));
#5056=EDGE_LOOP('',(#22600,#22601,#22602,#22603,#22604,#22605));
#5057=EDGE_LOOP('',(#22606,#22607,#22608,#22609,#22610));
#5058=EDGE_LOOP('',(#22611,#22612,#22613,#22614));
#5059=EDGE_LOOP('',(#22615,#22616,#22617,#22618,#22619));
#5060=EDGE_LOOP('',(#22620,#22621,#22622,#22623));
#5061=EDGE_LOOP('',(#22624,#22625,#22626,#22627,#22628));
#5062=EDGE_LOOP('',(#22629,#22630,#22631,#22632,#22633));
#5063=EDGE_LOOP('',(#22634,#22635,#22636,#22637));
#5064=EDGE_LOOP('',(#22638,#22639,#22640,#22641,#22642));
#5065=EDGE_LOOP('',(#22643,#22644,#22645,#22646,#22647,#22648));
#5066=EDGE_LOOP('',(#22649,#22650,#22651,#22652,#22653));
#5067=EDGE_LOOP('',(#22654,#22655,#22656,#22657));
#5068=EDGE_LOOP('',(#22658,#22659,#22660,#22661,#22662,#22663));
#5069=EDGE_LOOP('',(#22664,#22665,#22666,#22667,#22668));
#5070=EDGE_LOOP('',(#22669,#22670,#22671,#22672));
#5071=EDGE_LOOP('',(#22673,#22674,#22675,#22676,#22677));
#5072=EDGE_LOOP('',(#22678,#22679,#22680,#22681,#22682,#22683));
#5073=EDGE_LOOP('',(#22684,#22685,#22686,#22687,#22688));
#5074=EDGE_LOOP('',(#22689,#22690,#22691,#22692));
#5075=EDGE_LOOP('',(#22693,#22694,#22695,#22696,#22697));
#5076=EDGE_LOOP('',(#22698,#22699,#22700,#22701,#22702,#22703));
#5077=EDGE_LOOP('',(#22704,#22705,#22706,#22707));
#5078=EDGE_LOOP('',(#22708,#22709,#22710,#22711,#22712));
#5079=EDGE_LOOP('',(#22713,#22714,#22715,#22716,#22717,#22718));
#5080=EDGE_LOOP('',(#22719,#22720,#22721,#22722,#22723));
#5081=EDGE_LOOP('',(#22724,#22725,#22726,#22727));
#5082=EDGE_LOOP('',(#22728,#22729,#22730,#22731,#22732));
#5083=EDGE_LOOP('',(#22733,#22734,#22735,#22736));
#5084=EDGE_LOOP('',(#22737,#22738,#22739,#22740,#22741));
#5085=EDGE_LOOP('',(#22742,#22743,#22744,#22745,#22746));
#5086=EDGE_LOOP('',(#22747,#22748,#22749,#22750));
#5087=EDGE_LOOP('',(#22751,#22752,#22753,#22754,#22755));
#5088=EDGE_LOOP('',(#22756,#22757,#22758,#22759,#22760,#22761));
#5089=EDGE_LOOP('',(#22762,#22763,#22764,#22765,#22766));
#5090=EDGE_LOOP('',(#22767,#22768,#22769,#22770));
#5091=EDGE_LOOP('',(#22771,#22772,#22773,#22774,#22775,#22776));
#5092=EDGE_LOOP('',(#22777,#22778,#22779,#22780,#22781,#22782));
#5093=EDGE_LOOP('',(#22783,#22784,#22785,#22786,#22787));
#5094=EDGE_LOOP('',(#22788,#22789,#22790,#22791));
#5095=EDGE_LOOP('',(#22792,#22793,#22794,#22795,#22796));
#5096=EDGE_LOOP('',(#22797,#22798,#22799,#22800,#22801,#22802));
#5097=EDGE_LOOP('',(#22803,#22804,#22805,#22806,#22807));
#5098=EDGE_LOOP('',(#22808,#22809,#22810,#22811));
#5099=EDGE_LOOP('',(#22812,#22813,#22814,#22815,#22816));
#5100=EDGE_LOOP('',(#22817,#22818,#22819,#22820,#22821,#22822));
#5101=EDGE_LOOP('',(#22823,#22824,#22825,#22826,#22827));
#5102=EDGE_LOOP('',(#22828,#22829,#22830,#22831,#22832));
#5103=EDGE_LOOP('',(#22833,#22834,#22835,#22836));
#5104=EDGE_LOOP('',(#22837));
#5105=EDGE_LOOP('',(#22838,#22839,#22840,#22841));
#5106=EDGE_LOOP('',(#22842,#22843,#22844,#22845));
#5107=EDGE_LOOP('',(#22846,#22847,#22848));
#5108=EDGE_LOOP('',(#22849,#22850,#22851,#22852,#22853,#22854));
#5109=EDGE_LOOP('',(#22855,#22856,#22857,#22858,#22859,#22860));
#5110=EDGE_LOOP('',(#22861,#22862,#22863,#22864));
#5111=EDGE_LOOP('',(#22865,#22866,#22867,#22868));
#5112=EDGE_LOOP('',(#22869,#22870,#22871,#22872));
#5113=EDGE_LOOP('',(#22873,#22874,#22875,#22876));
#5114=EDGE_LOOP('',(#22877,#22878,#22879,#22880));
#5115=EDGE_LOOP('',(#22881,#22882,#22883,#22884));
#5116=EDGE_LOOP('',(#22885,#22886,#22887,#22888));
#5117=EDGE_LOOP('',(#22889,#22890,#22891,#22892,#22893,#22894));
#5118=EDGE_LOOP('',(#22895,#22896,#22897,#22898,#22899,#22900));
#5119=EDGE_LOOP('',(#22901,#22902,#22903,#22904,#22905,#22906));
#5120=EDGE_LOOP('',(#22907,#22908,#22909,#22910,#22911,#22912));
#5121=EDGE_LOOP('',(#22913,#22914,#22915,#22916,#22917));
#5122=EDGE_LOOP('',(#22918,#22919,#22920,#22921,#22922,#22923,#22924,#22925));
#5123=EDGE_LOOP('',(#22926,#22927,#22928,#22929));
#5124=EDGE_LOOP('',(#22930,#22931,#22932,#22933,#22934,#22935));
#5125=EDGE_LOOP('',(#22936,#22937,#22938,#22939));
#5126=EDGE_LOOP('',(#22940,#22941,#22942,#22943));
#5127=EDGE_LOOP('',(#22944,#22945,#22946,#22947));
#5128=EDGE_LOOP('',(#22948,#22949,#22950,#22951));
#5129=EDGE_LOOP('',(#22952,#22953,#22954,#22955));
#5130=EDGE_LOOP('',(#22956,#22957,#22958,#22959));
#5131=EDGE_LOOP('',(#22960,#22961,#22962,#22963));
#5132=EDGE_LOOP('',(#22964,#22965,#22966,#22967));
#5133=EDGE_LOOP('',(#22968,#22969,#22970,#22971));
#5134=EDGE_LOOP('',(#22972,#22973,#22974,#22975));
#5135=EDGE_LOOP('',(#22976,#22977,#22978,#22979));
#5136=EDGE_LOOP('',(#22980,#22981,#22982,#22983));
#5137=EDGE_LOOP('',(#22984,#22985,#22986,#22987));
#5138=EDGE_LOOP('',(#22988,#22989,#22990,#22991));
#5139=EDGE_LOOP('',(#22992,#22993,#22994,#22995));
#5140=EDGE_LOOP('',(#22996,#22997,#22998,#22999));
#5141=EDGE_LOOP('',(#23000,#23001,#23002,#23003));
#5142=EDGE_LOOP('',(#23004,#23005,#23006,#23007));
#5143=EDGE_LOOP('',(#23008,#23009,#23010,#23011));
#5144=EDGE_LOOP('',(#23012,#23013,#23014,#23015));
#5145=EDGE_LOOP('',(#23016,#23017,#23018,#23019));
#5146=EDGE_LOOP('',(#23020,#23021,#23022,#23023));
#5147=EDGE_LOOP('',(#23024,#23025,#23026,#23027));
#5148=EDGE_LOOP('',(#23028,#23029,#23030,#23031));
#5149=EDGE_LOOP('',(#23032,#23033,#23034,#23035));
#5150=EDGE_LOOP('',(#23036,#23037,#23038,#23039));
#5151=EDGE_LOOP('',(#23040,#23041,#23042,#23043));
#5152=EDGE_LOOP('',(#23044,#23045,#23046,#23047));
#5153=EDGE_LOOP('',(#23048,#23049,#23050,#23051,#23052));
#5154=EDGE_LOOP('',(#23053,#23054,#23055,#23056,#23057));
#5155=EDGE_LOOP('',(#23058,#23059,#23060,#23061));
#5156=EDGE_LOOP('',(#23062,#23063,#23064,#23065));
#5157=EDGE_LOOP('',(#23066,#23067,#23068,#23069));
#5158=EDGE_LOOP('',(#23070,#23071,#23072,#23073));
#5159=EDGE_LOOP('',(#23074,#23075,#23076,#23077));
#5160=EDGE_LOOP('',(#23078,#23079,#23080,#23081));
#5161=EDGE_LOOP('',(#23082,#23083,#23084,#23085));
#5162=EDGE_LOOP('',(#23086,#23087,#23088,#23089));
#5163=EDGE_LOOP('',(#23090,#23091,#23092,#23093));
#5164=EDGE_LOOP('',(#23094,#23095,#23096,#23097));
#5165=EDGE_LOOP('',(#23098,#23099,#23100,#23101));
#5166=EDGE_LOOP('',(#23102,#23103,#23104,#23105));
#5167=EDGE_LOOP('',(#23106,#23107,#23108,#23109));
#5168=EDGE_LOOP('',(#23110));
#5169=EDGE_LOOP('',(#23111));
#5170=EDGE_LOOP('',(#23112,#23113,#23114,#23115));
#5171=EDGE_LOOP('',(#23116,#23117,#23118));
#5172=EDGE_LOOP('',(#23119));
#5173=EDGE_LOOP('',(#23120));
#5174=EDGE_LOOP('',(#23121,#23122,#23123,#23124));
#5175=EDGE_LOOP('',(#23125,#23126,#23127,#23128,#23129,#23130,#23131,#23132,
#23133,#23134,#23135,#23136));
#5176=EDGE_LOOP('',(#23137,#23138,#23139,#23140));
#5177=EDGE_LOOP('',(#23141,#23142,#23143,#23144));
#5178=EDGE_LOOP('',(#23145,#23146,#23147,#23148));
#5179=EDGE_LOOP('',(#23149,#23150,#23151,#23152));
#5180=EDGE_LOOP('',(#23153,#23154,#23155,#23156));
#5181=EDGE_LOOP('',(#23157,#23158,#23159,#23160));
#5182=EDGE_LOOP('',(#23161,#23162,#23163,#23164));
#5183=EDGE_LOOP('',(#23165,#23166,#23167));
#5184=EDGE_LOOP('',(#23168,#23169,#23170,#23171,#23172));
#5185=EDGE_LOOP('',(#23173,#23174,#23175,#23176,#23177,#23178));
#5186=EDGE_LOOP('',(#23179,#23180,#23181,#23182,#23183,#23184));
#5187=EDGE_LOOP('',(#23185,#23186,#23187,#23188,#23189));
#5188=EDGE_LOOP('',(#23190,#23191,#23192,#23193));
#5189=EDGE_LOOP('',(#23194,#23195,#23196,#23197,#23198,#23199,#23200,#23201,
#23202));
#5190=EDGE_LOOP('',(#23203,#23204,#23205,#23206,#23207,#23208,#23209,#23210,
#23211,#23212,#23213,#23214));
#5191=EDGE_LOOP('',(#23215,#23216,#23217,#23218,#23219));
#5192=EDGE_LOOP('',(#23220,#23221,#23222,#23223,#23224,#23225));
#5193=EDGE_LOOP('',(#23226,#23227,#23228,#23229));
#5194=EDGE_LOOP('',(#23230,#23231,#23232,#23233));
#5195=EDGE_LOOP('',(#23234,#23235,#23236,#23237,#23238));
#5196=EDGE_LOOP('',(#23239,#23240,#23241,#23242));
#5197=EDGE_LOOP('',(#23243,#23244,#23245,#23246,#23247,#23248));
#5198=EDGE_LOOP('',(#23249,#23250,#23251,#23252,#23253));
#5199=EDGE_LOOP('',(#23254,#23255,#23256));
#5200=EDGE_LOOP('',(#23257,#23258,#23259,#23260));
#5201=EDGE_LOOP('',(#23261,#23262,#23263));
#5202=EDGE_LOOP('',(#23264,#23265,#23266,#23267));
#5203=EDGE_LOOP('',(#23268,#23269,#23270,#23271));
#5204=EDGE_LOOP('',(#23272,#23273,#23274,#23275));
#5205=EDGE_LOOP('',(#23276,#23277,#23278,#23279));
#5206=EDGE_LOOP('',(#23280,#23281,#23282,#23283));
#5207=EDGE_LOOP('',(#23284,#23285,#23286,#23287));
#5208=EDGE_LOOP('',(#23288,#23289,#23290,#23291));
#5209=EDGE_LOOP('',(#23292,#23293,#23294,#23295));
#5210=EDGE_LOOP('',(#23296,#23297,#23298,#23299));
#5211=EDGE_LOOP('',(#23300,#23301,#23302,#23303,#23304));
#5212=EDGE_LOOP('',(#23305,#23306,#23307,#23308,#23309));
#5213=EDGE_LOOP('',(#23310,#23311,#23312,#23313,#23314,#23315,#23316,#23317,
#23318,#23319,#23320,#23321,#23322,#23323,#23324,#23325));
#5214=EDGE_LOOP('',(#23326));
#5215=EDGE_LOOP('',(#23327));
#5216=EDGE_LOOP('',(#23328));
#5217=EDGE_LOOP('',(#23329));
#5218=EDGE_LOOP('',(#23330,#23331,#23332,#23333,#23334,#23335,#23336,#23337));
#5219=EDGE_LOOP('',(#23338));
#5220=EDGE_LOOP('',(#23339,#23340,#23341,#23342));
#5221=EDGE_LOOP('',(#23343,#23344,#23345,#23346));
#5222=EDGE_LOOP('',(#23347,#23348,#23349,#23350));
#5223=EDGE_LOOP('',(#23351,#23352,#23353,#23354));
#5224=EDGE_LOOP('',(#23355));
#5225=EDGE_LOOP('',(#23356));
#5226=EDGE_LOOP('',(#23357,#23358,#23359,#23360));
#5227=EDGE_LOOP('',(#23361,#23362,#23363,#23364));
#5228=EDGE_LOOP('',(#23365,#23366,#23367,#23368));
#5229=EDGE_LOOP('',(#23369));
#5230=EDGE_LOOP('',(#23370));
#5231=EDGE_LOOP('',(#23371,#23372,#23373,#23374));
#5232=EDGE_LOOP('',(#23375,#23376,#23377,#23378));
#5233=EDGE_LOOP('',(#23379,#23380,#23381,#23382));
#5234=EDGE_LOOP('',(#23383,#23384,#23385,#23386));
#5235=EDGE_LOOP('',(#23387,#23388,#23389,#23390));
#5236=EDGE_LOOP('',(#23391,#23392,#23393));
#5237=EDGE_LOOP('',(#23394,#23395,#23396));
#5238=EDGE_LOOP('',(#23397,#23398,#23399,#23400));
#5239=EDGE_LOOP('',(#23401,#23402,#23403,#23404));
#5240=EDGE_LOOP('',(#23405,#23406,#23407,#23408));
#5241=EDGE_LOOP('',(#23409,#23410,#23411,#23412));
#5242=EDGE_LOOP('',(#23413,#23414,#23415,#23416));
#5243=EDGE_LOOP('',(#23417,#23418,#23419,#23420,#23421,#23422));
#5244=EDGE_LOOP('',(#23423,#23424,#23425,#23426,#23427,#23428,#23429,#23430));
#5245=EDGE_LOOP('',(#23431,#23432,#23433,#23434));
#5246=EDGE_LOOP('',(#23435,#23436,#23437,#23438,#23439,#23440));
#5247=EDGE_LOOP('',(#23441,#23442,#23443));
#5248=EDGE_LOOP('',(#23444,#23445,#23446,#23447,#23448,#23449,#23450,#23451,
#23452,#23453,#23454));
#5249=EDGE_LOOP('',(#23455,#23456,#23457,#23458,#23459,#23460));
#5250=EDGE_LOOP('',(#23461,#23462,#23463,#23464));
#5251=EDGE_LOOP('',(#23465,#23466,#23467,#23468,#23469,#23470,#23471,#23472));
#5252=EDGE_LOOP('',(#23473,#23474,#23475,#23476));
#5253=EDGE_LOOP('',(#23477,#23478,#23479,#23480,#23481,#23482));
#5254=EDGE_LOOP('',(#23483,#23484,#23485,#23486));
#5255=EDGE_LOOP('',(#23487,#23488,#23489));
#5256=EDGE_LOOP('',(#23490,#23491,#23492,#23493));
#5257=EDGE_LOOP('',(#23494,#23495,#23496,#23497,#23498,#23499));
#5258=EDGE_LOOP('',(#23500,#23501,#23502,#23503,#23504,#23505,#23506,#23507,
#23508,#23509,#23510));
#5259=EDGE_LOOP('',(#23511,#23512,#23513,#23514));
#5260=EDGE_LOOP('',(#23515,#23516,#23517,#23518,#23519,#23520));
#5261=EDGE_LOOP('',(#23521,#23522,#23523,#23524,#23525));
#5262=EDGE_LOOP('',(#23526,#23527,#23528,#23529,#23530,#23531,#23532,#23533,
#23534,#23535,#23536));
#5263=EDGE_LOOP('',(#23537));
#5264=EDGE_LOOP('',(#23538));
#5265=EDGE_LOOP('',(#23539));
#5266=EDGE_LOOP('',(#23540,#23541,#23542,#23543,#23544));
#5267=EDGE_LOOP('',(#23545,#23546,#23547,#23548,#23549));
#5268=EDGE_LOOP('',(#23550,#23551,#23552,#23553,#23554));
#5269=EDGE_LOOP('',(#23555,#23556,#23557,#23558,#23559));
#5270=EDGE_LOOP('',(#23560,#23561,#23562,#23563,#23564));
#5271=EDGE_LOOP('',(#23565,#23566,#23567,#23568,#23569,#23570,#23571));
#5272=EDGE_LOOP('',(#23572,#23573,#23574,#23575,#23576,#23577,#23578,#23579,
#23580,#23581));
#5273=EDGE_LOOP('',(#23582,#23583,#23584,#23585,#23586));
#5274=EDGE_LOOP('',(#23587,#23588,#23589,#23590,#23591,#23592));
#5275=EDGE_LOOP('',(#23593,#23594,#23595,#23596,#23597,#23598,#23599,#23600,
#23601,#23602));
#5276=EDGE_LOOP('',(#23603));
#5277=EDGE_LOOP('',(#23604));
#5278=EDGE_LOOP('',(#23605));
#5279=EDGE_LOOP('',(#23606));
#5280=EDGE_LOOP('',(#23607,#23608,#23609,#23610));
#5281=EDGE_LOOP('',(#23611,#23612,#23613,#23614,#23615));
#5282=EDGE_LOOP('',(#23616,#23617,#23618,#23619));
#5283=EDGE_LOOP('',(#23620,#23621,#23622,#23623));
#5284=EDGE_LOOP('',(#23624,#23625,#23626,#23627));
#5285=EDGE_LOOP('',(#23628,#23629,#23630,#23631));
#5286=EDGE_LOOP('',(#23632,#23633,#23634,#23635));
#5287=EDGE_LOOP('',(#23636,#23637,#23638,#23639));
#5288=EDGE_LOOP('',(#23640,#23641,#23642,#23643,#23644));
#5289=EDGE_LOOP('',(#23645,#23646,#23647,#23648,#23649,#23650,#23651,#23652,
#23653,#23654,#23655,#23656));
#5290=EDGE_LOOP('',(#23657));
#5291=EDGE_LOOP('',(#23658));
#5292=EDGE_LOOP('',(#23659));
#5293=EDGE_LOOP('',(#23660));
#5294=EDGE_LOOP('',(#23661,#23662,#23663,#23664,#23665,#23666,#23667,#23668,
#23669,#23670,#23671,#23672));
#5295=EDGE_LOOP('',(#23673));
#5296=EDGE_LOOP('',(#23674,#23675,#23676,#23677,#23678,#23679));
#5297=EDGE_LOOP('',(#23680,#23681,#23682,#23683));
#5298=EDGE_LOOP('',(#23684,#23685,#23686,#23687));
#5299=EDGE_LOOP('',(#23688,#23689,#23690,#23691));
#5300=EDGE_LOOP('',(#23692,#23693,#23694,#23695));
#5301=EDGE_LOOP('',(#23696,#23697,#23698,#23699,#23700,#23701,#23702,#23703));
#5302=EDGE_LOOP('',(#23704,#23705,#23706,#23707,#23708));
#5303=EDGE_LOOP('',(#23709,#23710,#23711,#23712,#23713,#23714));
#5304=EDGE_LOOP('',(#23715,#23716,#23717,#23718));
#5305=EDGE_LOOP('',(#23719,#23720,#23721,#23722,#23723,#23724,#23725,#23726,
#23727,#23728));
#5306=EDGE_LOOP('',(#23729,#23730,#23731,#23732));
#5307=EDGE_LOOP('',(#23733,#23734,#23735,#23736,#23737));
#5308=EDGE_LOOP('',(#23738,#23739,#23740,#23741,#23742,#23743));
#5309=EDGE_LOOP('',(#23744,#23745,#23746,#23747,#23748));
#5310=EDGE_LOOP('',(#23749,#23750,#23751,#23752,#23753,#23754));
#5311=EDGE_LOOP('',(#23755,#23756,#23757,#23758,#23759));
#5312=EDGE_LOOP('',(#23760,#23761,#23762,#23763,#23764,#23765));
#5313=EDGE_LOOP('',(#23766,#23767,#23768,#23769));
#5314=EDGE_LOOP('',(#23770,#23771,#23772,#23773,#23774));
#5315=EDGE_LOOP('',(#23775,#23776,#23777,#23778,#23779,#23780));
#5316=EDGE_LOOP('',(#23781,#23782,#23783,#23784));
#5317=EDGE_LOOP('',(#23785,#23786,#23787,#23788,#23789,#23790,#23791,#23792,
#23793,#23794,#23795,#23796,#23797,#23798,#23799,#23800,#23801,#23802,#23803,
#23804));
#5318=EDGE_LOOP('',(#23805,#23806,#23807,#23808,#23809,#23810,#23811,#23812,
#23813,#23814));
#5319=EDGE_LOOP('',(#23815,#23816,#23817,#23818));
#5320=EDGE_LOOP('',(#23819));
#5321=EDGE_LOOP('',(#23820,#23821,#23822,#23823,#23824,#23825,#23826,#23827,
#23828,#23829));
#5322=EDGE_LOOP('',(#23830,#23831,#23832,#23833,#23834,#23835,#23836,#23837,
#23838));
#5323=EDGE_LOOP('',(#23839,#23840,#23841,#23842,#23843));
#5324=EDGE_LOOP('',(#23844,#23845,#23846,#23847));
#5325=EDGE_LOOP('',(#23848,#23849,#23850,#23851,#23852));
#5326=EDGE_LOOP('',(#23853,#23854,#23855,#23856));
#5327=EDGE_LOOP('',(#23857,#23858,#23859,#23860));
#5328=EDGE_LOOP('',(#23861,#23862,#23863,#23864));
#5329=EDGE_LOOP('',(#23865,#23866,#23867,#23868,#23869,#23870,#23871,#23872,
#23873,#23874,#23875,#23876,#23877,#23878,#23879,#23880,#23881,#23882,#23883,
#23884));
#5330=EDGE_LOOP('',(#23885));
#5331=EDGE_LOOP('',(#23886,#23887,#23888,#23889,#23890,#23891));
#5332=EDGE_LOOP('',(#23892,#23893,#23894,#23895,#23896));
#5333=EDGE_LOOP('',(#23897,#23898,#23899,#23900));
#5334=EDGE_LOOP('',(#23901,#23902,#23903,#23904));
#5335=EDGE_LOOP('',(#23905,#23906,#23907,#23908));
#5336=EDGE_LOOP('',(#23909,#23910,#23911,#23912,#23913,#23914));
#5337=EDGE_LOOP('',(#23915,#23916,#23917,#23918,#23919,#23920));
#5338=EDGE_LOOP('',(#23921,#23922,#23923));
#5339=EDGE_LOOP('',(#23924,#23925,#23926));
#5340=EDGE_LOOP('',(#23927,#23928,#23929,#23930,#23931,#23932));
#5341=EDGE_LOOP('',(#23933,#23934,#23935,#23936,#23937,#23938));
#5342=EDGE_LOOP('',(#23939,#23940,#23941,#23942,#23943));
#5343=EDGE_LOOP('',(#23944,#23945,#23946,#23947));
#5344=EDGE_LOOP('',(#23948,#23949,#23950));
#5345=EDGE_LOOP('',(#23951,#23952,#23953,#23954));
#5346=EDGE_LOOP('',(#23955,#23956,#23957,#23958,#23959,#23960));
#5347=EDGE_LOOP('',(#23961,#23962,#23963));
#5348=EDGE_LOOP('',(#23964,#23965,#23966));
#5349=EDGE_LOOP('',(#23967,#23968,#23969,#23970));
#5350=EDGE_LOOP('',(#23971,#23972,#23973,#23974));
#5351=EDGE_LOOP('',(#23975,#23976,#23977,#23978));
#5352=EDGE_LOOP('',(#23979,#23980,#23981,#23982));
#5353=EDGE_LOOP('',(#23983,#23984,#23985,#23986));
#5354=EDGE_LOOP('',(#23987,#23988,#23989,#23990,#23991,#23992,#23993,#23994));
#5355=EDGE_LOOP('',(#23995,#23996,#23997,#23998));
#5356=EDGE_LOOP('',(#23999,#24000,#24001,#24002));
#5357=EDGE_LOOP('',(#24003,#24004,#24005,#24006));
#5358=EDGE_LOOP('',(#24007,#24008,#24009,#24010));
#5359=EDGE_LOOP('',(#24011,#24012,#24013,#24014,#24015,#24016,#24017,#24018));
#5360=EDGE_LOOP('',(#24019,#24020,#24021,#24022));
#5361=EDGE_LOOP('',(#24023,#24024,#24025,#24026));
#5362=EDGE_LOOP('',(#24027,#24028,#24029,#24030));
#5363=EDGE_LOOP('',(#24031,#24032,#24033,#24034,#24035,#24036));
#5364=EDGE_LOOP('',(#24037,#24038,#24039,#24040));
#5365=EDGE_LOOP('',(#24041,#24042,#24043,#24044,#24045,#24046,#24047,#24048));
#5366=EDGE_LOOP('',(#24049,#24050,#24051,#24052,#24053,#24054));
#5367=EDGE_LOOP('',(#24055,#24056,#24057,#24058));
#5368=EDGE_LOOP('',(#24059,#24060,#24061,#24062,#24063));
#5369=EDGE_LOOP('',(#24064,#24065,#24066,#24067));
#5370=EDGE_LOOP('',(#24068,#24069,#24070,#24071));
#5371=EDGE_LOOP('',(#24072,#24073,#24074,#24075));
#5372=EDGE_LOOP('',(#24076,#24077,#24078,#24079));
#5373=EDGE_LOOP('',(#24080,#24081,#24082,#24083));
#5374=EDGE_LOOP('',(#24084,#24085,#24086,#24087,#24088,#24089));
#5375=EDGE_LOOP('',(#24090,#24091,#24092,#24093,#24094,#24095,#24096,#24097,
#24098,#24099));
#5376=EDGE_LOOP('',(#24100,#24101,#24102,#24103,#24104,#24105));
#5377=EDGE_LOOP('',(#24106,#24107,#24108,#24109));
#5378=EDGE_LOOP('',(#24110,#24111,#24112,#24113));
#5379=EDGE_LOOP('',(#24114,#24115,#24116,#24117));
#5380=EDGE_LOOP('',(#24118,#24119,#24120,#24121));
#5381=EDGE_LOOP('',(#24122,#24123,#24124,#24125));
#5382=EDGE_LOOP('',(#24126,#24127,#24128,#24129));
#5383=EDGE_LOOP('',(#24130,#24131,#24132,#24133));
#5384=EDGE_LOOP('',(#24134,#24135,#24136,#24137));
#5385=EDGE_LOOP('',(#24138,#24139,#24140,#24141));
#5386=EDGE_LOOP('',(#24142,#24143,#24144,#24145));
#5387=EDGE_LOOP('',(#24146,#24147,#24148,#24149,#24150,#24151,#24152,#24153,
#24154));
#5388=EDGE_LOOP('',(#24155,#24156,#24157,#24158));
#5389=EDGE_LOOP('',(#24159,#24160,#24161,#24162));
#5390=EDGE_LOOP('',(#24163,#24164,#24165,#24166));
#5391=EDGE_LOOP('',(#24167,#24168,#24169,#24170));
#5392=EDGE_LOOP('',(#24171,#24172,#24173,#24174));
#5393=EDGE_LOOP('',(#24175,#24176,#24177,#24178));
#5394=EDGE_LOOP('',(#24179,#24180,#24181,#24182));
#5395=EDGE_LOOP('',(#24183,#24184,#24185,#24186));
#5396=EDGE_LOOP('',(#24187,#24188,#24189,#24190));
#5397=EDGE_LOOP('',(#24191,#24192,#24193,#24194));
#5398=EDGE_LOOP('',(#24195,#24196,#24197,#24198,#24199,#24200,#24201,#24202,
#24203,#24204));
#5399=EDGE_LOOP('',(#24205,#24206,#24207,#24208));
#5400=EDGE_LOOP('',(#24209,#24210,#24211,#24212));
#5401=EDGE_LOOP('',(#24213,#24214,#24215,#24216));
#5402=EDGE_LOOP('',(#24217,#24218,#24219,#24220));
#5403=EDGE_LOOP('',(#24221,#24222,#24223,#24224));
#5404=EDGE_LOOP('',(#24225,#24226,#24227,#24228));
#5405=EDGE_LOOP('',(#24229,#24230,#24231,#24232));
#5406=EDGE_LOOP('',(#24233,#24234,#24235,#24236));
#5407=EDGE_LOOP('',(#24237,#24238,#24239,#24240));
#5408=EDGE_LOOP('',(#24241,#24242,#24243,#24244));
#5409=EDGE_LOOP('',(#24245,#24246,#24247,#24248));
#5410=EDGE_LOOP('',(#24249,#24250,#24251,#24252));
#5411=EDGE_LOOP('',(#24253,#24254,#24255,#24256));
#5412=EDGE_LOOP('',(#24257,#24258,#24259,#24260));
#5413=EDGE_LOOP('',(#24261,#24262,#24263,#24264));
#5414=EDGE_LOOP('',(#24265,#24266,#24267,#24268));
#5415=EDGE_LOOP('',(#24269,#24270,#24271,#24272));
#5416=EDGE_LOOP('',(#24273,#24274,#24275,#24276));
#5417=EDGE_LOOP('',(#24277,#24278,#24279,#24280,#24281,#24282,#24283,#24284,
#24285,#24286));
#5418=EDGE_LOOP('',(#24287,#24288,#24289,#24290,#24291,#24292,#24293,#24294));
#5419=EDGE_LOOP('',(#24295,#24296,#24297,#24298));
#5420=EDGE_LOOP('',(#24299,#24300,#24301,#24302));
#5421=EDGE_LOOP('',(#24303,#24304,#24305,#24306));
#5422=EDGE_LOOP('',(#24307,#24308,#24309,#24310));
#5423=EDGE_LOOP('',(#24311,#24312,#24313,#24314));
#5424=EDGE_LOOP('',(#24315));
#5425=EDGE_LOOP('',(#24316));
#5426=EDGE_LOOP('',(#24317,#24318,#24319,#24320));
#5427=EDGE_LOOP('',(#24321));
#5428=EDGE_LOOP('',(#24322));
#5429=EDGE_LOOP('',(#24323,#24324,#24325,#24326));
#5430=EDGE_LOOP('',(#24327,#24328,#24329,#24330));
#5431=EDGE_LOOP('',(#24331,#24332,#24333,#24334));
#5432=EDGE_LOOP('',(#24335,#24336,#24337,#24338));
#5433=EDGE_LOOP('',(#24339,#24340,#24341,#24342));
#5434=EDGE_LOOP('',(#24343,#24344,#24345,#24346));
#5435=EDGE_LOOP('',(#24347,#24348,#24349,#24350));
#5436=EDGE_LOOP('',(#24351,#24352,#24353,#24354,#24355));
#5437=EDGE_LOOP('',(#24356,#24357,#24358,#24359));
#5438=EDGE_LOOP('',(#24360,#24361,#24362,#24363));
#5439=EDGE_LOOP('',(#24364,#24365,#24366,#24367,#24368));
#5440=EDGE_LOOP('',(#24369,#24370,#24371,#24372,#24373,#24374,#24375,#24376,
#24377));
#5441=EDGE_LOOP('',(#24378,#24379,#24380,#24381));
#5442=EDGE_LOOP('',(#24382,#24383,#24384,#24385,#24386));
#5443=EDGE_LOOP('',(#24387,#24388,#24389,#24390));
#5444=EDGE_LOOP('',(#24391,#24392,#24393,#24394));
#5445=EDGE_LOOP('',(#24395));
#5446=EDGE_LOOP('',(#24396));
#5447=EDGE_LOOP('',(#24397,#24398,#24399,#24400));
#5448=EDGE_LOOP('',(#24401));
#5449=EDGE_LOOP('',(#24402));
#5450=EDGE_LOOP('',(#24403,#24404,#24405,#24406));
#5451=EDGE_LOOP('',(#24407,#24408,#24409,#24410));
#5452=EDGE_LOOP('',(#24411,#24412,#24413,#24414,#24415,#24416,#24417,#24418));
#5453=EDGE_LOOP('',(#24419,#24420,#24421,#24422));
#5454=EDGE_LOOP('',(#24423,#24424,#24425,#24426));
#5455=EDGE_LOOP('',(#24427,#24428,#24429,#24430));
#5456=EDGE_LOOP('',(#24431,#24432,#24433,#24434));
#5457=EDGE_LOOP('',(#24435,#24436,#24437,#24438,#24439,#24440));
#5458=EDGE_LOOP('',(#24441,#24442,#24443,#24444));
#5459=EDGE_LOOP('',(#24445,#24446,#24447,#24448));
#5460=EDGE_LOOP('',(#24449,#24450,#24451,#24452));
#5461=EDGE_LOOP('',(#24453,#24454,#24455,#24456));
#5462=EDGE_LOOP('',(#24457,#24458,#24459,#24460));
#5463=EDGE_LOOP('',(#24461,#24462,#24463,#24464));
#5464=EDGE_LOOP('',(#24465,#24466,#24467,#24468,#24469));
#5465=EDGE_LOOP('',(#24470,#24471,#24472,#24473,#24474,#24475));
#5466=EDGE_LOOP('',(#24476,#24477,#24478,#24479,#24480,#24481));
#5467=EDGE_LOOP('',(#24482,#24483,#24484,#24485));
#5468=EDGE_LOOP('',(#24486,#24487,#24488));
#5469=EDGE_LOOP('',(#24489,#24490,#24491,#24492,#24493,#24494));
#5470=EDGE_LOOP('',(#24495,#24496,#24497,#24498));
#5471=EDGE_LOOP('',(#24499,#24500,#24501,#24502,#24503));
#5472=EDGE_LOOP('',(#24504,#24505,#24506,#24507));
#5473=EDGE_LOOP('',(#24508,#24509,#24510,#24511));
#5474=EDGE_LOOP('',(#24512,#24513,#24514,#24515));
#5475=EDGE_LOOP('',(#24516,#24517,#24518,#24519));
#5476=EDGE_LOOP('',(#24520,#24521,#24522,#24523));
#5477=EDGE_LOOP('',(#24524,#24525,#24526,#24527));
#5478=EDGE_LOOP('',(#24528,#24529,#24530,#24531));
#5479=EDGE_LOOP('',(#24532,#24533,#24534,#24535));
#5480=EDGE_LOOP('',(#24536,#24537,#24538,#24539));
#5481=EDGE_LOOP('',(#24540,#24541,#24542,#24543));
#5482=EDGE_LOOP('',(#24544,#24545,#24546,#24547));
#5483=EDGE_LOOP('',(#24548,#24549,#24550,#24551));
#5484=EDGE_LOOP('',(#24552,#24553,#24554,#24555));
#5485=EDGE_LOOP('',(#24556,#24557,#24558,#24559));
#5486=EDGE_LOOP('',(#24560,#24561,#24562,#24563));
#5487=EDGE_LOOP('',(#24564,#24565,#24566,#24567,#24568,#24569,#24570,#24571,
#24572,#24573));
#5488=EDGE_LOOP('',(#24574,#24575,#24576,#24577));
#5489=EDGE_LOOP('',(#24578,#24579,#24580,#24581));
#5490=EDGE_LOOP('',(#24582,#24583,#24584,#24585));
#5491=EDGE_LOOP('',(#24586,#24587,#24588,#24589));
#5492=EDGE_LOOP('',(#24590,#24591,#24592,#24593));
#5493=EDGE_LOOP('',(#24594,#24595,#24596,#24597));
#5494=EDGE_LOOP('',(#24598,#24599,#24600,#24601));
#5495=EDGE_LOOP('',(#24602,#24603,#24604,#24605));
#5496=EDGE_LOOP('',(#24606,#24607,#24608,#24609));
#5497=EDGE_LOOP('',(#24610,#24611,#24612,#24613));
#5498=EDGE_LOOP('',(#24614,#24615,#24616,#24617));
#5499=EDGE_LOOP('',(#24618,#24619,#24620,#24621));
#5500=EDGE_LOOP('',(#24622,#24623,#24624,#24625));
#5501=EDGE_LOOP('',(#24626,#24627,#24628,#24629));
#5502=EDGE_LOOP('',(#24630,#24631,#24632,#24633));
#5503=EDGE_LOOP('',(#24634,#24635,#24636,#24637));
#5504=EDGE_LOOP('',(#24638,#24639,#24640,#24641));
#5505=EDGE_LOOP('',(#24642,#24643,#24644,#24645));
#5506=EDGE_LOOP('',(#24646,#24647,#24648,#24649));
#5507=EDGE_LOOP('',(#24650,#24651,#24652,#24653));
#5508=EDGE_LOOP('',(#24654,#24655,#24656,#24657));
#5509=EDGE_LOOP('',(#24658,#24659,#24660,#24661));
#5510=EDGE_LOOP('',(#24662,#24663,#24664,#24665));
#5511=EDGE_LOOP('',(#24666,#24667,#24668,#24669));
#5512=EDGE_LOOP('',(#24670,#24671,#24672,#24673,#24674));
#5513=EDGE_LOOP('',(#24675,#24676,#24677,#24678));
#5514=EDGE_LOOP('',(#24679,#24680,#24681,#24682));
#5515=EDGE_LOOP('',(#24683,#24684,#24685,#24686));
#5516=EDGE_LOOP('',(#24687,#24688,#24689,#24690));
#5517=EDGE_LOOP('',(#24691,#24692,#24693,#24694));
#5518=EDGE_LOOP('',(#24695,#24696,#24697,#24698));
#5519=EDGE_LOOP('',(#24699,#24700,#24701,#24702));
#5520=EDGE_LOOP('',(#24703,#24704,#24705,#24706));
#5521=EDGE_LOOP('',(#24707,#24708,#24709,#24710));
#5522=EDGE_LOOP('',(#24711,#24712,#24713,#24714));
#5523=EDGE_LOOP('',(#24715,#24716,#24717,#24718));
#5524=EDGE_LOOP('',(#24719,#24720,#24721,#24722));
#5525=EDGE_LOOP('',(#24723,#24724,#24725,#24726));
#5526=EDGE_LOOP('',(#24727,#24728,#24729,#24730));
#5527=EDGE_LOOP('',(#24731,#24732,#24733,#24734));
#5528=EDGE_LOOP('',(#24735,#24736,#24737,#24738));
#5529=EDGE_LOOP('',(#24739,#24740,#24741,#24742));
#5530=EDGE_LOOP('',(#24743,#24744,#24745,#24746));
#5531=EDGE_LOOP('',(#24747,#24748,#24749,#24750));
#5532=EDGE_LOOP('',(#24751,#24752,#24753,#24754));
#5533=EDGE_LOOP('',(#24755,#24756,#24757,#24758));
#5534=EDGE_LOOP('',(#24759,#24760,#24761,#24762));
#5535=EDGE_LOOP('',(#24763,#24764,#24765,#24766));
#5536=EDGE_LOOP('',(#24767,#24768,#24769,#24770));
#5537=EDGE_LOOP('',(#24771,#24772,#24773,#24774));
#5538=EDGE_LOOP('',(#24775,#24776,#24777,#24778));
#5539=EDGE_LOOP('',(#24779,#24780,#24781,#24782));
#5540=EDGE_LOOP('',(#24783,#24784,#24785,#24786));
#5541=EDGE_LOOP('',(#24787,#24788,#24789,#24790));
#5542=EDGE_LOOP('',(#24791,#24792,#24793,#24794));
#5543=EDGE_LOOP('',(#24795,#24796,#24797,#24798));
#5544=EDGE_LOOP('',(#24799,#24800,#24801,#24802));
#5545=EDGE_LOOP('',(#24803,#24804,#24805,#24806));
#5546=EDGE_LOOP('',(#24807,#24808,#24809,#24810));
#5547=EDGE_LOOP('',(#24811,#24812,#24813,#24814));
#5548=EDGE_LOOP('',(#24815,#24816,#24817,#24818));
#5549=EDGE_LOOP('',(#24819,#24820,#24821,#24822));
#5550=EDGE_LOOP('',(#24823,#24824,#24825,#24826));
#5551=EDGE_LOOP('',(#24827,#24828,#24829,#24830));
#5552=EDGE_LOOP('',(#24831,#24832,#24833,#24834));
#5553=EDGE_LOOP('',(#24835,#24836,#24837,#24838));
#5554=EDGE_LOOP('',(#24839,#24840,#24841,#24842));
#5555=EDGE_LOOP('',(#24843,#24844,#24845,#24846));
#5556=EDGE_LOOP('',(#24847,#24848,#24849,#24850));
#5557=EDGE_LOOP('',(#24851,#24852,#24853,#24854));
#5558=EDGE_LOOP('',(#24855,#24856,#24857,#24858));
#5559=EDGE_LOOP('',(#24859,#24860,#24861,#24862));
#5560=EDGE_LOOP('',(#24863,#24864,#24865,#24866,#24867,#24868,#24869,#24870,
#24871,#24872,#24873,#24874,#24875,#24876,#24877,#24878));
#5561=EDGE_LOOP('',(#24879,#24880,#24881,#24882,#24883,#24884,#24885,#24886,
#24887));
#5562=EDGE_LOOP('',(#24888,#24889,#24890,#24891,#24892,#24893,#24894,#24895));
#5563=EDGE_LOOP('',(#24896,#24897,#24898,#24899));
#5564=EDGE_LOOP('',(#24900,#24901,#24902,#24903));
#5565=EDGE_LOOP('',(#24904,#24905,#24906,#24907));
#5566=EDGE_LOOP('',(#24908,#24909,#24910,#24911));
#5567=EDGE_LOOP('',(#24912,#24913,#24914,#24915));
#5568=EDGE_LOOP('',(#24916,#24917,#24918,#24919));
#5569=EDGE_LOOP('',(#24920,#24921,#24922,#24923));
#5570=EDGE_LOOP('',(#24924,#24925,#24926,#24927));
#5571=EDGE_LOOP('',(#24928,#24929,#24930,#24931));
#5572=EDGE_LOOP('',(#24932,#24933,#24934,#24935));
#5573=EDGE_LOOP('',(#24936,#24937,#24938,#24939));
#5574=EDGE_LOOP('',(#24940,#24941,#24942,#24943));
#5575=EDGE_LOOP('',(#24944,#24945,#24946,#24947));
#5576=EDGE_LOOP('',(#24948,#24949,#24950,#24951));
#5577=EDGE_LOOP('',(#24952,#24953,#24954,#24955));
#5578=EDGE_LOOP('',(#24956,#24957,#24958,#24959));
#5579=EDGE_LOOP('',(#24960,#24961,#24962,#24963));
#5580=EDGE_LOOP('',(#24964,#24965,#24966,#24967));
#5581=EDGE_LOOP('',(#24968,#24969,#24970,#24971));
#5582=EDGE_LOOP('',(#24972,#24973,#24974,#24975));
#5583=EDGE_LOOP('',(#24976,#24977,#24978,#24979));
#5584=EDGE_LOOP('',(#24980,#24981,#24982,#24983));
#5585=EDGE_LOOP('',(#24984,#24985,#24986,#24987));
#5586=EDGE_LOOP('',(#24988,#24989,#24990,#24991));
#5587=EDGE_LOOP('',(#24992,#24993,#24994,#24995));
#5588=EDGE_LOOP('',(#24996,#24997,#24998,#24999));
#5589=EDGE_LOOP('',(#25000,#25001,#25002,#25003));
#5590=EDGE_LOOP('',(#25004,#25005,#25006,#25007));
#5591=EDGE_LOOP('',(#25008,#25009,#25010,#25011));
#5592=EDGE_LOOP('',(#25012,#25013,#25014,#25015));
#5593=EDGE_LOOP('',(#25016,#25017,#25018,#25019));
#5594=EDGE_LOOP('',(#25020,#25021,#25022,#25023));
#5595=EDGE_LOOP('',(#25024,#25025,#25026,#25027));
#5596=EDGE_LOOP('',(#25028,#25029,#25030,#25031));
#5597=EDGE_LOOP('',(#25032,#25033,#25034,#25035));
#5598=EDGE_LOOP('',(#25036,#25037,#25038,#25039));
#5599=EDGE_LOOP('',(#25040,#25041,#25042,#25043));
#5600=EDGE_LOOP('',(#25044,#25045,#25046,#25047));
#5601=EDGE_LOOP('',(#25048,#25049,#25050,#25051,#25052,#25053,#25054,#25055,
#25056,#25057,#25058,#25059,#25060,#25061,#25062,#25063));
#5602=EDGE_LOOP('',(#25064,#25065,#25066,#25067,#25068,#25069,#25070,#25071,
#25072));
#5603=EDGE_LOOP('',(#25073,#25074,#25075,#25076,#25077,#25078,#25079,#25080));
#5604=EDGE_LOOP('',(#25081,#25082,#25083,#25084,#25085,#25086,#25087,#25088,
#25089));
#5605=EDGE_LOOP('',(#25090,#25091,#25092,#25093,#25094,#25095,#25096,#25097));
#5606=EDGE_LOOP('',(#25098,#25099,#25100,#25101,#25102,#25103,#25104,#25105,
#25106));
#5607=EDGE_LOOP('',(#25107,#25108,#25109,#25110,#25111,#25112,#25113,#25114));
#5608=EDGE_LOOP('',(#25115,#25116,#25117,#25118,#25119));
#5609=EDGE_LOOP('',(#25120,#25121,#25122,#25123,#25124,#25125,#25126,#25127,
#25128,#25129,#25130,#25131,#25132,#25133,#25134,#25135,#25136,#25137,#25138,
#25139,#25140,#25141,#25142,#25143,#25144,#25145,#25146,#25147,#25148,#25149,
#25150,#25151,#25152));
#5610=EDGE_LOOP('',(#25153,#25154,#25155,#25156,#25157));
#5611=EDGE_LOOP('',(#25158,#25159,#25160,#25161));
#5612=EDGE_LOOP('',(#25162,#25163,#25164,#25165,#25166,#25167,#25168,#25169,
#25170,#25171,#25172,#25173,#25174,#25175,#25176,#25177,#25178,#25179,#25180,
#25181,#25182,#25183,#25184,#25185,#25186,#25187,#25188,#25189,#25190,#25191,
#25192,#25193));
#5613=EDGE_LOOP('',(#25194,#25195,#25196,#25197,#25198,#25199,#25200));
#5614=EDGE_LOOP('',(#25201,#25202,#25203,#25204,#25205,#25206));
#5615=EDGE_LOOP('',(#25207));
#5616=EDGE_LOOP('',(#25208,#25209,#25210));
#5617=EDGE_LOOP('',(#25211,#25212,#25213,#25214,#25215,#25216,#25217,#25218,
#25219,#25220));
#5618=EDGE_LOOP('',(#25221,#25222,#25223,#25224));
#5619=EDGE_LOOP('',(#25225,#25226,#25227,#25228));
#5620=EDGE_LOOP('',(#25229,#25230,#25231,#25232));
#5621=EDGE_LOOP('',(#25233,#25234,#25235,#25236));
#5622=EDGE_LOOP('',(#25237,#25238,#25239,#25240));
#5623=EDGE_LOOP('',(#25241,#25242,#25243,#25244,#25245));
#5624=EDGE_LOOP('',(#25246));
#5625=EDGE_LOOP('',(#25247,#25248,#25249,#25250,#25251,#25252,#25253,#25254,
#25255,#25256,#25257,#25258,#25259,#25260,#25261,#25262));
#5626=EDGE_LOOP('',(#25263,#25264,#25265,#25266));
#5627=EDGE_LOOP('',(#25267,#25268,#25269,#25270,#25271,#25272,#25273,#25274,
#25275,#25276,#25277,#25278,#25279,#25280,#25281,#25282));
#5628=EDGE_LOOP('',(#25283));
#5629=EDGE_LOOP('',(#25284,#25285,#25286,#25287,#25288,#25289));
#5630=LINE('',#35354,#8127);
#5631=LINE('',#35417,#8128);
#5632=LINE('',#35421,#8129);
#5633=LINE('',#35481,#8130);
#5634=LINE('',#35485,#8131);
#5635=LINE('',#35507,#8132);
#5636=LINE('',#35511,#8133);
#5637=LINE('',#35533,#8134);
#5638=LINE('',#35537,#8135);
#5639=LINE('',#35597,#8136);
#5640=LINE('',#35601,#8137);
#5641=LINE('',#35661,#8138);
#5642=LINE('',#35665,#8139);
#5643=LINE('',#35725,#8140);
#5644=LINE('',#35729,#8141);
#5645=LINE('',#35789,#8142);
#5646=LINE('',#35793,#8143);
#5647=LINE('',#35853,#8144);
#5648=LINE('',#35857,#8145);
#5649=LINE('',#35877,#8146);
#5650=LINE('',#35881,#8147);
#5651=LINE('',#35903,#8148);
#5652=LINE('',#35907,#8149);
#5653=LINE('',#35967,#8150);
#5654=LINE('',#35971,#8151);
#5655=LINE('',#36031,#8152);
#5656=LINE('',#36035,#8153);
#5657=LINE('',#36095,#8154);
#5658=LINE('',#36099,#8155);
#5659=LINE('',#36159,#8156);
#5660=LINE('',#36163,#8157);
#5661=LINE('',#36223,#8158);
#5662=LINE('',#36227,#8159);
#5663=LINE('',#36287,#8160);
#5664=LINE('',#36291,#8161);
#5665=LINE('',#36351,#8162);
#5666=LINE('',#36354,#8163);
#5667=LINE('',#36358,#8164);
#5668=LINE('',#36363,#8165);
#5669=LINE('',#36417,#8166);
#5670=LINE('',#36421,#8167);
#5671=LINE('',#36481,#8168);
#5672=LINE('',#36485,#8169);
#5673=LINE('',#36545,#8170);
#5674=LINE('',#36549,#8171);
#5675=LINE('',#36609,#8172);
#5676=LINE('',#36613,#8173);
#5677=LINE('',#36635,#8174);
#5678=LINE('',#36639,#8175);
#5679=LINE('',#36699,#8176);
#5680=LINE('',#36703,#8177);
#5681=LINE('',#36763,#8178);
#5682=LINE('',#36767,#8179);
#5683=LINE('',#36827,#8180);
#5684=LINE('',#36831,#8181);
#5685=LINE('',#36891,#8182);
#5686=LINE('',#36895,#8183);
#5687=LINE('',#36955,#8184);
#5688=LINE('',#36959,#8185);
#5689=LINE('',#36981,#8186);
#5690=LINE('',#36985,#8187);
#5691=LINE('',#37045,#8188);
#5692=LINE('',#37049,#8189);
#5693=LINE('',#37109,#8190);
#5694=LINE('',#37113,#8191);
#5695=LINE('',#37173,#8192);
#5696=LINE('',#37177,#8193);
#5697=LINE('',#37199,#8194);
#5698=LINE('',#37203,#8195);
#5699=LINE('',#37263,#8196);
#5700=LINE('',#37267,#8197);
#5701=LINE('',#37327,#8198);
#5702=LINE('',#37331,#8199);
#5703=LINE('',#37391,#8200);
#5704=LINE('',#37395,#8201);
#5705=LINE('',#37408,#8202);
#5706=LINE('',#37416,#8203);
#5707=LINE('',#37420,#8204);
#5708=LINE('',#37425,#8205);
#5709=LINE('',#37429,#8206);
#5710=LINE('',#37436,#8207);
#5711=LINE('',#37440,#8208);
#5712=LINE('',#37512,#8209);
#5713=LINE('',#37520,#8210);
#5714=LINE('',#37521,#8211);
#5715=LINE('',#37599,#8212);
#5716=LINE('',#37671,#8213);
#5717=LINE('',#37679,#8214);
#5718=LINE('',#37680,#8215);
#5719=LINE('',#37758,#8216);
#5720=LINE('',#37830,#8217);
#5721=LINE('',#37838,#8218);
#5722=LINE('',#37839,#8219);
#5723=LINE('',#37917,#8220);
#5724=LINE('',#37989,#8221);
#5725=LINE('',#37997,#8222);
#5726=LINE('',#37998,#8223);
#5727=LINE('',#38076,#8224);
#5728=LINE('',#38148,#8225);
#5729=LINE('',#38156,#8226);
#5730=LINE('',#38157,#8227);
#5731=LINE('',#38235,#8228);
#5732=LINE('',#38307,#8229);
#5733=LINE('',#38315,#8230);
#5734=LINE('',#38316,#8231);
#5735=LINE('',#38394,#8232);
#5736=LINE('',#38466,#8233);
#5737=LINE('',#38474,#8234);
#5738=LINE('',#38475,#8235);
#5739=LINE('',#38553,#8236);
#5740=LINE('',#38625,#8237);
#5741=LINE('',#38633,#8238);
#5742=LINE('',#38634,#8239);
#5743=LINE('',#38712,#8240);
#5744=LINE('',#38784,#8241);
#5745=LINE('',#38792,#8242);
#5746=LINE('',#38793,#8243);
#5747=LINE('',#38871,#8244);
#5748=LINE('',#38943,#8245);
#5749=LINE('',#38951,#8246);
#5750=LINE('',#38952,#8247);
#5751=LINE('',#39030,#8248);
#5752=LINE('',#39102,#8249);
#5753=LINE('',#39110,#8250);
#5754=LINE('',#39111,#8251);
#5755=LINE('',#39189,#8252);
#5756=LINE('',#39261,#8253);
#5757=LINE('',#39269,#8254);
#5758=LINE('',#39270,#8255);
#5759=LINE('',#39348,#8256);
#5760=LINE('',#39420,#8257);
#5761=LINE('',#39428,#8258);
#5762=LINE('',#39429,#8259);
#5763=LINE('',#39507,#8260);
#5764=LINE('',#39579,#8261);
#5765=LINE('',#39587,#8262);
#5766=LINE('',#39588,#8263);
#5767=LINE('',#39666,#8264);
#5768=LINE('',#39738,#8265);
#5769=LINE('',#39746,#8266);
#5770=LINE('',#39747,#8267);
#5771=LINE('',#39825,#8268);
#5772=LINE('',#39897,#8269);
#5773=LINE('',#39905,#8270);
#5774=LINE('',#39906,#8271);
#5775=LINE('',#39984,#8272);
#5776=LINE('',#40056,#8273);
#5777=LINE('',#40064,#8274);
#5778=LINE('',#40065,#8275);
#5779=LINE('',#40143,#8276);
#5780=LINE('',#40215,#8277);
#5781=LINE('',#40223,#8278);
#5782=LINE('',#40224,#8279);
#5783=LINE('',#40302,#8280);
#5784=LINE('',#40326,#8281);
#5785=LINE('',#40359,#8282);
#5786=LINE('',#40443,#8283);
#5787=LINE('',#40533,#8284);
#5788=LINE('',#40623,#8285);
#5789=LINE('',#40707,#8286);
#5790=LINE('',#40797,#8287);
#5791=LINE('',#40881,#8288);
#5792=LINE('',#40971,#8289);
#5793=LINE('',#41061,#8290);
#5794=LINE('',#41145,#8291);
#5795=LINE('',#41235,#8292);
#5796=LINE('',#41325,#8293);
#5797=LINE('',#41409,#8294);
#5798=LINE('',#41419,#8295);
#5799=LINE('',#41455,#8296);
#5800=LINE('',#41492,#8297);
#5801=LINE('',#41530,#8298);
#5802=LINE('',#41567,#8299);
#5803=LINE('',#41604,#8300);
#5804=LINE('',#41642,#8301);
#5805=LINE('',#41679,#8302);
#5806=LINE('',#41716,#8303);
#5807=LINE('',#41753,#8304);
#5808=LINE('',#41790,#8305);
#5809=LINE('',#41828,#8306);
#5810=LINE('',#43606,#8307);
#5811=LINE('',#43610,#8308);
#5812=LINE('',#43615,#8309);
#5813=LINE('',#43619,#8310);
#5814=LINE('',#43629,#8311);
#5815=LINE('',#43635,#8312);
#5816=LINE('',#43637,#8313);
#5817=LINE('',#43638,#8314);
#5818=LINE('',#43643,#8315);
#5819=LINE('',#43661,#8316);
#5820=LINE('',#43663,#8317);
#5821=LINE('',#43665,#8318);
#5822=LINE('',#43677,#8319);
#5823=LINE('',#43683,#8320);
#5824=LINE('',#43685,#8321);
#5825=LINE('',#43686,#8322);
#5826=LINE('',#43689,#8323);
#5827=LINE('',#43691,#8324);
#5828=LINE('',#43693,#8325);
#5829=LINE('',#43699,#8326);
#5830=LINE('',#43700,#8327);
#5831=LINE('',#43712,#8328);
#5832=LINE('',#43713,#8329);
#5833=LINE('',#43717,#8330);
#5834=LINE('',#43725,#8331);
#5835=LINE('',#43726,#8332);
#5836=LINE('',#43731,#8333);
#5837=LINE('',#43735,#8334);
#5838=LINE('',#43739,#8335);
#5839=LINE('',#43743,#8336);
#5840=LINE('',#43747,#8337);
#5841=LINE('',#43751,#8338);
#5842=LINE('',#43770,#8339);
#5843=LINE('',#43776,#8340);
#5844=LINE('',#43778,#8341);
#5845=LINE('',#43779,#8342);
#5846=LINE('',#43782,#8343);
#5847=LINE('',#43784,#8344);
#5848=LINE('',#43786,#8345);
#5849=LINE('',#43797,#8346);
#5850=LINE('',#43798,#8347);
#5851=LINE('',#43803,#8348);
#5852=LINE('',#43806,#8349);
#5853=LINE('',#43808,#8350);
#5854=LINE('',#43809,#8351);
#5855=LINE('',#43812,#8352);
#5856=LINE('',#43813,#8353);
#5857=LINE('',#43828,#8354);
#5858=LINE('',#43831,#8355);
#5859=LINE('',#43834,#8356);
#5860=LINE('',#43839,#8357);
#5861=LINE('',#43847,#8358);
#5862=LINE('',#43853,#8359);
#5863=LINE('',#43855,#8360);
#5864=LINE('',#43856,#8361);
#5865=LINE('',#43859,#8362);
#5866=LINE('',#43861,#8363);
#5867=LINE('',#43863,#8364);
#5868=LINE('',#43874,#8365);
#5869=LINE('',#43875,#8366);
#5870=LINE('',#43880,#8367);
#5871=LINE('',#43888,#8368);
#5872=LINE('',#43894,#8369);
#5873=LINE('',#43896,#8370);
#5874=LINE('',#43897,#8371);
#5875=LINE('',#43902,#8372);
#5876=LINE('',#43917,#8373);
#5877=LINE('',#43918,#8374);
#5878=LINE('',#43923,#8375);
#5879=LINE('',#43926,#8376);
#5880=LINE('',#43933,#8377);
#5881=LINE('',#43935,#8378);
#5882=LINE('',#43936,#8379);
#5883=LINE('',#43939,#8380);
#5884=LINE('',#43941,#8381);
#5885=LINE('',#43943,#8382);
#5886=LINE('',#43954,#8383);
#5887=LINE('',#43955,#8384);
#5888=LINE('',#43957,#8385);
#5889=LINE('',#43960,#8386);
#5890=LINE('',#43966,#8387);
#5891=LINE('',#43968,#8388);
#5892=LINE('',#43969,#8389);
#5893=LINE('',#43974,#8390);
#5894=LINE('',#43975,#8391);
#5895=LINE('',#43980,#8392);
#5896=LINE('',#43983,#8393);
#5897=LINE('',#44014,#8394);
#5898=LINE('',#44017,#8395);
#5899=LINE('',#44020,#8396);
#5900=LINE('',#44026,#8397);
#5901=LINE('',#44032,#8398);
#5902=LINE('',#44038,#8399);
#5903=LINE('',#44045,#8400);
#5904=LINE('',#44047,#8401);
#5905=LINE('',#44061,#8402);
#5906=LINE('',#44065,#8403);
#5907=LINE('',#44069,#8404);
#5908=LINE('',#44334,#8405);
#5909=LINE('',#44495,#8406);
#5910=LINE('',#44500,#8407);
#5911=LINE('',#44529,#8408);
#5912=LINE('',#44908,#8409);
#5913=LINE('',#44946,#8410);
#5914=LINE('',#45313,#8411);
#5915=LINE('',#45315,#8412);
#5916=LINE('',#45317,#8413);
#5917=LINE('',#45319,#8414);
#5918=LINE('',#45321,#8415);
#5919=LINE('',#45323,#8416);
#5920=LINE('',#45326,#8417);
#5921=LINE('',#45332,#8418);
#5922=LINE('',#45336,#8419);
#5923=LINE('',#45341,#8420);
#5924=LINE('',#45346,#8421);
#5925=LINE('',#45379,#8422);
#5926=LINE('',#45463,#8423);
#5927=LINE('',#45553,#8424);
#5928=LINE('',#45643,#8425);
#5929=LINE('',#45733,#8426);
#5930=LINE('',#45817,#8427);
#5931=LINE('',#45907,#8428);
#5932=LINE('',#45918,#8429);
#5933=LINE('',#45956,#8430);
#5934=LINE('',#45993,#8431);
#5935=LINE('',#46030,#8432);
#5936=LINE('',#46068,#8433);
#5937=LINE('',#46106,#8434);
#5938=LINE('',#47281,#8435);
#5939=LINE('',#47285,#8436);
#5940=LINE('',#47289,#8437);
#5941=LINE('',#47293,#8438);
#5942=LINE('',#47297,#8439);
#5943=LINE('',#47300,#8440);
#5944=LINE('',#47305,#8441);
#5945=LINE('',#47363,#8442);
#5946=LINE('',#47365,#8443);
#5947=LINE('',#47366,#8444);
#5948=LINE('',#47369,#8445);
#5949=LINE('',#47370,#8446);
#5950=LINE('',#47373,#8447);
#5951=LINE('',#47374,#8448);
#5952=LINE('',#47377,#8449);
#5953=LINE('',#47378,#8450);
#5954=LINE('',#47381,#8451);
#5955=LINE('',#47382,#8452);
#5956=LINE('',#47385,#8453);
#5957=LINE('',#47386,#8454);
#5958=LINE('',#47389,#8455);
#5959=LINE('',#47390,#8456);
#5960=LINE('',#47393,#8457);
#5961=LINE('',#47394,#8458);
#5962=LINE('',#47397,#8459);
#5963=LINE('',#47398,#8460);
#5964=LINE('',#47400,#8461);
#5965=LINE('',#47402,#8462);
#5966=LINE('',#47405,#8463);
#5967=LINE('',#47408,#8464);
#5968=LINE('',#47409,#8465);
#5969=LINE('',#47411,#8466);
#5970=LINE('',#47413,#8467);
#5971=LINE('',#47416,#8468);
#5972=LINE('',#47417,#8469);
#5973=LINE('',#47419,#8470);
#5974=LINE('',#47423,#8471);
#5975=LINE('',#47431,#8472);
#5976=LINE('',#47437,#8473);
#5977=LINE('',#47443,#8474);
#5978=LINE('',#47445,#8475);
#5979=LINE('',#47447,#8476);
#5980=LINE('',#47448,#8477);
#5981=LINE('',#47451,#8478);
#5982=LINE('',#47453,#8479);
#5983=LINE('',#47454,#8480);
#5984=LINE('',#47457,#8481);
#5985=LINE('',#47459,#8482);
#5986=LINE('',#47460,#8483);
#5987=LINE('',#47462,#8484);
#5988=LINE('',#47463,#8485);
#5989=LINE('',#47468,#8486);
#5990=LINE('',#47470,#8487);
#5991=LINE('',#47472,#8488);
#5992=LINE('',#47473,#8489);
#5993=LINE('',#47476,#8490);
#5994=LINE('',#47478,#8491);
#5995=LINE('',#47479,#8492);
#5996=LINE('',#47482,#8493);
#5997=LINE('',#47484,#8494);
#5998=LINE('',#47485,#8495);
#5999=LINE('',#47487,#8496);
#6000=LINE('',#47488,#8497);
#6001=LINE('',#47493,#8498);
#6002=LINE('',#47495,#8499);
#6003=LINE('',#47496,#8500);
#6004=LINE('',#47500,#8501);
#6005=LINE('',#47502,#8502);
#6006=LINE('',#47503,#8503);
#6007=LINE('',#47507,#8504);
#6008=LINE('',#47509,#8505);
#6009=LINE('',#47510,#8506);
#6010=LINE('',#47514,#8507);
#6011=LINE('',#47516,#8508);
#6012=LINE('',#47517,#8509);
#6013=LINE('',#47521,#8510);
#6014=LINE('',#47523,#8511);
#6015=LINE('',#47524,#8512);
#6016=LINE('',#47526,#8513);
#6017=LINE('',#47527,#8514);
#6018=LINE('',#47531,#8515);
#6019=LINE('',#47533,#8516);
#6020=LINE('',#47534,#8517);
#6021=LINE('',#47538,#8518);
#6022=LINE('',#47540,#8519);
#6023=LINE('',#47541,#8520);
#6024=LINE('',#47543,#8521);
#6025=LINE('',#47544,#8522);
#6026=LINE('',#47546,#8523);
#6027=LINE('',#47547,#8524);
#6028=LINE('',#47551,#8525);
#6029=LINE('',#47553,#8526);
#6030=LINE('',#47554,#8527);
#6031=LINE('',#47556,#8528);
#6032=LINE('',#47557,#8529);
#6033=LINE('',#47559,#8530);
#6034=LINE('',#47560,#8531);
#6035=LINE('',#47562,#8532);
#6036=LINE('',#47563,#8533);
#6037=LINE('',#47565,#8534);
#6038=LINE('',#47566,#8535);
#6039=LINE('',#47568,#8536);
#6040=LINE('',#47569,#8537);
#6041=LINE('',#47571,#8538);
#6042=LINE('',#47572,#8539);
#6043=LINE('',#47574,#8540);
#6044=LINE('',#47575,#8541);
#6045=LINE('',#47577,#8542);
#6046=LINE('',#47578,#8543);
#6047=LINE('',#47580,#8544);
#6048=LINE('',#47581,#8545);
#6049=LINE('',#47592,#8546);
#6050=LINE('',#47625,#8547);
#6051=LINE('',#47709,#8548);
#6052=LINE('',#47799,#8549);
#6053=LINE('',#47889,#8550);
#6054=LINE('',#47973,#8551);
#6055=LINE('',#48063,#8552);
#6056=LINE('',#48147,#8553);
#6057=LINE('',#48237,#8554);
#6058=LINE('',#48327,#8555);
#6059=LINE('',#48411,#8556);
#6060=LINE('',#48501,#8557);
#6061=LINE('',#48585,#8558);
#6062=LINE('',#48675,#8559);
#6063=LINE('',#48765,#8560);
#6064=LINE('',#48849,#8561);
#6065=LINE('',#48939,#8562);
#6066=LINE('',#49029,#8563);
#6067=LINE('',#49113,#8564);
#6068=LINE('',#49203,#8565);
#6069=LINE('',#49287,#8566);
#6070=LINE('',#49377,#8567);
#6071=LINE('',#49467,#8568);
#6072=LINE('',#49551,#8569);
#6073=LINE('',#49641,#8570);
#6074=LINE('',#49725,#8571);
#6075=LINE('',#49815,#8572);
#6076=LINE('',#49905,#8573);
#6077=LINE('',#49989,#8574);
#6078=LINE('',#50079,#8575);
#6079=LINE('',#50089,#8576);
#6080=LINE('',#50126,#8577);
#6081=LINE('',#50163,#8578);
#6082=LINE('',#50200,#8579);
#6083=LINE('',#50238,#8580);
#6084=LINE('',#50275,#8581);
#6085=LINE('',#50312,#8582);
#6086=LINE('',#50349,#8583);
#6087=LINE('',#50386,#8584);
#6088=LINE('',#50424,#8585);
#6089=LINE('',#50461,#8586);
#6090=LINE('',#50498,#8587);
#6091=LINE('',#50535,#8588);
#6092=LINE('',#50572,#8589);
#6093=LINE('',#50610,#8590);
#6094=LINE('',#50647,#8591);
#6095=LINE('',#50684,#8592);
#6096=LINE('',#50722,#8593);
#6097=LINE('',#50759,#8594);
#6098=LINE('',#50796,#8595);
#6099=LINE('',#50833,#8596);
#6100=LINE('',#50870,#8597);
#6101=LINE('',#50908,#8598);
#6102=LINE('',#50945,#8599);
#6103=LINE('',#50982,#8600);
#6104=LINE('',#51019,#8601);
#6105=LINE('',#51056,#8602);
#6106=LINE('',#51094,#8603);
#6107=LINE('',#54459,#8604);
#6108=LINE('',#54463,#8605);
#6109=LINE('',#54467,#8606);
#6110=LINE('',#54471,#8607);
#6111=LINE('',#54475,#8608);
#6112=LINE('',#54478,#8609);
#6113=LINE('',#54483,#8610);
#6114=LINE('',#54541,#8611);
#6115=LINE('',#54543,#8612);
#6116=LINE('',#54544,#8613);
#6117=LINE('',#54547,#8614);
#6118=LINE('',#54548,#8615);
#6119=LINE('',#54551,#8616);
#6120=LINE('',#54552,#8617);
#6121=LINE('',#54555,#8618);
#6122=LINE('',#54556,#8619);
#6123=LINE('',#54559,#8620);
#6124=LINE('',#54560,#8621);
#6125=LINE('',#54563,#8622);
#6126=LINE('',#54564,#8623);
#6127=LINE('',#54567,#8624);
#6128=LINE('',#54568,#8625);
#6129=LINE('',#54571,#8626);
#6130=LINE('',#54572,#8627);
#6131=LINE('',#54575,#8628);
#6132=LINE('',#54576,#8629);
#6133=LINE('',#54578,#8630);
#6134=LINE('',#54580,#8631);
#6135=LINE('',#54583,#8632);
#6136=LINE('',#54586,#8633);
#6137=LINE('',#54587,#8634);
#6138=LINE('',#54589,#8635);
#6139=LINE('',#54591,#8636);
#6140=LINE('',#54594,#8637);
#6141=LINE('',#54595,#8638);
#6142=LINE('',#54597,#8639);
#6143=LINE('',#54601,#8640);
#6144=LINE('',#54609,#8641);
#6145=LINE('',#54615,#8642);
#6146=LINE('',#54622,#8643);
#6147=LINE('',#54627,#8644);
#6148=LINE('',#54634,#8645);
#6149=LINE('',#54640,#8646);
#6150=LINE('',#54670,#8647);
#6151=LINE('',#54675,#8648);
#6152=LINE('',#54678,#8649);
#6153=LINE('',#54684,#8650);
#6154=LINE('',#54697,#8651);
#6155=LINE('',#54706,#8652);
#6156=LINE('',#54708,#8653);
#6157=LINE('',#54714,#8654);
#6158=LINE('',#54747,#8655);
#6159=LINE('',#54831,#8656);
#6160=LINE('',#54921,#8657);
#6161=LINE('',#55011,#8658);
#6162=LINE('',#55095,#8659);
#6163=LINE('',#55185,#8660);
#6164=LINE('',#55269,#8661);
#6165=LINE('',#55359,#8662);
#6166=LINE('',#55449,#8663);
#6167=LINE('',#55533,#8664);
#6168=LINE('',#55623,#8665);
#6169=LINE('',#55713,#8666);
#6170=LINE('',#55797,#8667);
#6171=LINE('',#55887,#8668);
#6172=LINE('',#55971,#8669);
#6173=LINE('',#56061,#8670);
#6174=LINE('',#56151,#8671);
#6175=LINE('',#56235,#8672);
#6176=LINE('',#56325,#8673);
#6177=LINE('',#56335,#8674);
#6178=LINE('',#56372,#8675);
#6179=LINE('',#56409,#8676);
#6180=LINE('',#56446,#8677);
#6181=LINE('',#56484,#8678);
#6182=LINE('',#56521,#8679);
#6183=LINE('',#56558,#8680);
#6184=LINE('',#56595,#8681);
#6185=LINE('',#56632,#8682);
#6186=LINE('',#56670,#8683);
#6187=LINE('',#56707,#8684);
#6188=LINE('',#56744,#8685);
#6189=LINE('',#56782,#8686);
#6190=LINE('',#56819,#8687);
#6191=LINE('',#56856,#8688);
#6192=LINE('',#56893,#8689);
#6193=LINE('',#56930,#8690);
#6194=LINE('',#56968,#8691);
#6195=LINE('',#59325,#8692);
#6196=LINE('',#59329,#8693);
#6197=LINE('',#59333,#8694);
#6198=LINE('',#59337,#8695);
#6199=LINE('',#59341,#8696);
#6200=LINE('',#59344,#8697);
#6201=LINE('',#59349,#8698);
#6202=LINE('',#59407,#8699);
#6203=LINE('',#59409,#8700);
#6204=LINE('',#59410,#8701);
#6205=LINE('',#59413,#8702);
#6206=LINE('',#59414,#8703);
#6207=LINE('',#59417,#8704);
#6208=LINE('',#59418,#8705);
#6209=LINE('',#59421,#8706);
#6210=LINE('',#59422,#8707);
#6211=LINE('',#59425,#8708);
#6212=LINE('',#59426,#8709);
#6213=LINE('',#59429,#8710);
#6214=LINE('',#59430,#8711);
#6215=LINE('',#59433,#8712);
#6216=LINE('',#59434,#8713);
#6217=LINE('',#59437,#8714);
#6218=LINE('',#59438,#8715);
#6219=LINE('',#59441,#8716);
#6220=LINE('',#59442,#8717);
#6221=LINE('',#59444,#8718);
#6222=LINE('',#59446,#8719);
#6223=LINE('',#59449,#8720);
#6224=LINE('',#59452,#8721);
#6225=LINE('',#59453,#8722);
#6226=LINE('',#59455,#8723);
#6227=LINE('',#59457,#8724);
#6228=LINE('',#59460,#8725);
#6229=LINE('',#59461,#8726);
#6230=LINE('',#59463,#8727);
#6231=LINE('',#59467,#8728);
#6232=LINE('',#59475,#8729);
#6233=LINE('',#59481,#8730);
#6234=LINE('',#59670,#8731);
#6235=LINE('',#59767,#8732);
#6236=LINE('',#59885,#8733);
#6237=LINE('',#59942,#8734);
#6238=LINE('',#59954,#8735);
#6239=LINE('',#60181,#8736);
#6240=LINE('',#60186,#8737);
#6241=LINE('',#60225,#8738);
#6242=LINE('',#60468,#8739);
#6243=LINE('',#60592,#8740);
#6244=LINE('',#60597,#8741);
#6245=LINE('',#60831,#8742);
#6246=LINE('',#60837,#8743);
#6247=LINE('',#60843,#8744);
#6248=LINE('',#60845,#8745);
#6249=LINE('',#60850,#8746);
#6250=LINE('',#60852,#8747);
#6251=LINE('',#60854,#8748);
#6252=LINE('',#60856,#8749);
#6253=LINE('',#60858,#8750);
#6254=LINE('',#60859,#8751);
#6255=LINE('',#60862,#8752);
#6256=LINE('',#60864,#8753);
#6257=LINE('',#60866,#8754);
#6258=LINE('',#60867,#8755);
#6259=LINE('',#60870,#8756);
#6260=LINE('',#60871,#8757);
#6261=LINE('',#60874,#8758);
#6262=LINE('',#60876,#8759);
#6263=LINE('',#60877,#8760);
#6264=LINE('',#60881,#8761);
#6265=LINE('',#60883,#8762);
#6266=LINE('',#60885,#8763);
#6267=LINE('',#60887,#8764);
#6268=LINE('',#60889,#8765);
#6269=LINE('',#60890,#8766);
#6270=LINE('',#60893,#8767);
#6271=LINE('',#60895,#8768);
#6272=LINE('',#60897,#8769);
#6273=LINE('',#60898,#8770);
#6274=LINE('',#60901,#8771);
#6275=LINE('',#60902,#8772);
#6276=LINE('',#60905,#8773);
#6277=LINE('',#60907,#8774);
#6278=LINE('',#60908,#8775);
#6279=LINE('',#60912,#8776);
#6280=LINE('',#60914,#8777);
#6281=LINE('',#60916,#8778);
#6282=LINE('',#60918,#8779);
#6283=LINE('',#60920,#8780);
#6284=LINE('',#60921,#8781);
#6285=LINE('',#60924,#8782);
#6286=LINE('',#60926,#8783);
#6287=LINE('',#60927,#8784);
#6288=LINE('',#60930,#8785);
#6289=LINE('',#60932,#8786);
#6290=LINE('',#60933,#8787);
#6291=LINE('',#60936,#8788);
#6292=LINE('',#60938,#8789);
#6293=LINE('',#60940,#8790);
#6294=LINE('',#60941,#8791);
#6295=LINE('',#60945,#8792);
#6296=LINE('',#60947,#8793);
#6297=LINE('',#60949,#8794);
#6298=LINE('',#60951,#8795);
#6299=LINE('',#60953,#8796);
#6300=LINE('',#60954,#8797);
#6301=LINE('',#60957,#8798);
#6302=LINE('',#60959,#8799);
#6303=LINE('',#60961,#8800);
#6304=LINE('',#60962,#8801);
#6305=LINE('',#60965,#8802);
#6306=LINE('',#60966,#8803);
#6307=LINE('',#60969,#8804);
#6308=LINE('',#60971,#8805);
#6309=LINE('',#60972,#8806);
#6310=LINE('',#60976,#8807);
#6311=LINE('',#60978,#8808);
#6312=LINE('',#60980,#8809);
#6313=LINE('',#60982,#8810);
#6314=LINE('',#60984,#8811);
#6315=LINE('',#60985,#8812);
#6316=LINE('',#60988,#8813);
#6317=LINE('',#60990,#8814);
#6318=LINE('',#60991,#8815);
#6319=LINE('',#60994,#8816);
#6320=LINE('',#60996,#8817);
#6321=LINE('',#60998,#8818);
#6322=LINE('',#60999,#8819);
#6323=LINE('',#61002,#8820);
#6324=LINE('',#61004,#8821);
#6325=LINE('',#61005,#8822);
#6326=LINE('',#61009,#8823);
#6327=LINE('',#61011,#8824);
#6328=LINE('',#61013,#8825);
#6329=LINE('',#61015,#8826);
#6330=LINE('',#61017,#8827);
#6331=LINE('',#61018,#8828);
#6332=LINE('',#61021,#8829);
#6333=LINE('',#61023,#8830);
#6334=LINE('',#61025,#8831);
#6335=LINE('',#61026,#8832);
#6336=LINE('',#61029,#8833);
#6337=LINE('',#61031,#8834);
#6338=LINE('',#61033,#8835);
#6339=LINE('',#61034,#8836);
#6340=LINE('',#61037,#8837);
#6341=LINE('',#61038,#8838);
#6342=LINE('',#61041,#8839);
#6343=LINE('',#61043,#8840);
#6344=LINE('',#61045,#8841);
#6345=LINE('',#61046,#8842);
#6346=LINE('',#61049,#8843);
#6347=LINE('',#61051,#8844);
#6348=LINE('',#61052,#8845);
#6349=LINE('',#61056,#8846);
#6350=LINE('',#61058,#8847);
#6351=LINE('',#61060,#8848);
#6352=LINE('',#61062,#8849);
#6353=LINE('',#61064,#8850);
#6354=LINE('',#61065,#8851);
#6355=LINE('',#61068,#8852);
#6356=LINE('',#61070,#8853);
#6357=LINE('',#61071,#8854);
#6358=LINE('',#61074,#8855);
#6359=LINE('',#61076,#8856);
#6360=LINE('',#61077,#8857);
#6361=LINE('',#61079,#8858);
#6362=LINE('',#61080,#8859);
#6363=LINE('',#61084,#8860);
#6364=LINE('',#61086,#8861);
#6365=LINE('',#61088,#8862);
#6366=LINE('',#61090,#8863);
#6367=LINE('',#61092,#8864);
#6368=LINE('',#61093,#8865);
#6369=LINE('',#61096,#8866);
#6370=LINE('',#61098,#8867);
#6371=LINE('',#61099,#8868);
#6372=LINE('',#61102,#8869);
#6373=LINE('',#61104,#8870);
#6374=LINE('',#61106,#8871);
#6375=LINE('',#61107,#8872);
#6376=LINE('',#61110,#8873);
#6377=LINE('',#61112,#8874);
#6378=LINE('',#61113,#8875);
#6379=LINE('',#61117,#8876);
#6380=LINE('',#61119,#8877);
#6381=LINE('',#61121,#8878);
#6382=LINE('',#61123,#8879);
#6383=LINE('',#61125,#8880);
#6384=LINE('',#61126,#8881);
#6385=LINE('',#61129,#8882);
#6386=LINE('',#61131,#8883);
#6387=LINE('',#61133,#8884);
#6388=LINE('',#61134,#8885);
#6389=LINE('',#61137,#8886);
#6390=LINE('',#61139,#8887);
#6391=LINE('',#61141,#8888);
#6392=LINE('',#61142,#8889);
#6393=LINE('',#61145,#8890);
#6394=LINE('',#61146,#8891);
#6395=LINE('',#61149,#8892);
#6396=LINE('',#61151,#8893);
#6397=LINE('',#61153,#8894);
#6398=LINE('',#61154,#8895);
#6399=LINE('',#61157,#8896);
#6400=LINE('',#61159,#8897);
#6401=LINE('',#61160,#8898);
#6402=LINE('',#61164,#8899);
#6403=LINE('',#61166,#8900);
#6404=LINE('',#61168,#8901);
#6405=LINE('',#61170,#8902);
#6406=LINE('',#61172,#8903);
#6407=LINE('',#61173,#8904);
#6408=LINE('',#61176,#8905);
#6409=LINE('',#61178,#8906);
#6410=LINE('',#61179,#8907);
#6411=LINE('',#61182,#8908);
#6412=LINE('',#61184,#8909);
#6413=LINE('',#61185,#8910);
#6414=LINE('',#61187,#8911);
#6415=LINE('',#61188,#8912);
#6416=LINE('',#61192,#8913);
#6417=LINE('',#61194,#8914);
#6418=LINE('',#61196,#8915);
#6419=LINE('',#61198,#8916);
#6420=LINE('',#61200,#8917);
#6421=LINE('',#61201,#8918);
#6422=LINE('',#61204,#8919);
#6423=LINE('',#61206,#8920);
#6424=LINE('',#61208,#8921);
#6425=LINE('',#61209,#8922);
#6426=LINE('',#61212,#8923);
#6427=LINE('',#61214,#8924);
#6428=LINE('',#61216,#8925);
#6429=LINE('',#61217,#8926);
#6430=LINE('',#61220,#8927);
#6431=LINE('',#61221,#8928);
#6432=LINE('',#61224,#8929);
#6433=LINE('',#61226,#8930);
#6434=LINE('',#61228,#8931);
#6435=LINE('',#61229,#8932);
#6436=LINE('',#61232,#8933);
#6437=LINE('',#61234,#8934);
#6438=LINE('',#61235,#8935);
#6439=LINE('',#61239,#8936);
#6440=LINE('',#61241,#8937);
#6441=LINE('',#61243,#8938);
#6442=LINE('',#61245,#8939);
#6443=LINE('',#61247,#8940);
#6444=LINE('',#61248,#8941);
#6445=LINE('',#61251,#8942);
#6446=LINE('',#61253,#8943);
#6447=LINE('',#61254,#8944);
#6448=LINE('',#61257,#8945);
#6449=LINE('',#61259,#8946);
#6450=LINE('',#61260,#8947);
#6451=LINE('',#61263,#8948);
#6452=LINE('',#61265,#8949);
#6453=LINE('',#61267,#8950);
#6454=LINE('',#61268,#8951);
#6455=LINE('',#61271,#8952);
#6456=LINE('',#61273,#8953);
#6457=LINE('',#61275,#8954);
#6458=LINE('',#61277,#8955);
#6459=LINE('',#61278,#8956);
#6460=LINE('',#61281,#8957);
#6461=LINE('',#61283,#8958);
#6462=LINE('',#61284,#8959);
#6463=LINE('',#61287,#8960);
#6464=LINE('',#61289,#8961);
#6465=LINE('',#61290,#8962);
#6466=LINE('',#61293,#8963);
#6467=LINE('',#61294,#8964);
#6468=LINE('',#61295,#8965);
#6469=LINE('',#61299,#8966);
#6470=LINE('',#61301,#8967);
#6471=LINE('',#61303,#8968);
#6472=LINE('',#61305,#8969);
#6473=LINE('',#61307,#8970);
#6474=LINE('',#61308,#8971);
#6475=LINE('',#61311,#8972);
#6476=LINE('',#61313,#8973);
#6477=LINE('',#61315,#8974);
#6478=LINE('',#61316,#8975);
#6479=LINE('',#61319,#8976);
#6480=LINE('',#61321,#8977);
#6481=LINE('',#61323,#8978);
#6482=LINE('',#61324,#8979);
#6483=LINE('',#61327,#8980);
#6484=LINE('',#61328,#8981);
#6485=LINE('',#61331,#8982);
#6486=LINE('',#61333,#8983);
#6487=LINE('',#61335,#8984);
#6488=LINE('',#61336,#8985);
#6489=LINE('',#61339,#8986);
#6490=LINE('',#61341,#8987);
#6491=LINE('',#61342,#8988);
#6492=LINE('',#61346,#8989);
#6493=LINE('',#61348,#8990);
#6494=LINE('',#61350,#8991);
#6495=LINE('',#61352,#8992);
#6496=LINE('',#61354,#8993);
#6497=LINE('',#61355,#8994);
#6498=LINE('',#61358,#8995);
#6499=LINE('',#61360,#8996);
#6500=LINE('',#61362,#8997);
#6501=LINE('',#61363,#8998);
#6502=LINE('',#61366,#8999);
#6503=LINE('',#61368,#9000);
#6504=LINE('',#61370,#9001);
#6505=LINE('',#61371,#9002);
#6506=LINE('',#61374,#9003);
#6507=LINE('',#61375,#9004);
#6508=LINE('',#61378,#9005);
#6509=LINE('',#61380,#9006);
#6510=LINE('',#61382,#9007);
#6511=LINE('',#61383,#9008);
#6512=LINE('',#61386,#9009);
#6513=LINE('',#61388,#9010);
#6514=LINE('',#61389,#9011);
#6515=LINE('',#61393,#9012);
#6516=LINE('',#61395,#9013);
#6517=LINE('',#61397,#9014);
#6518=LINE('',#61399,#9015);
#6519=LINE('',#61401,#9016);
#6520=LINE('',#61402,#9017);
#6521=LINE('',#61405,#9018);
#6522=LINE('',#61407,#9019);
#6523=LINE('',#61409,#9020);
#6524=LINE('',#61410,#9021);
#6525=LINE('',#61413,#9022);
#6526=LINE('',#61414,#9023);
#6527=LINE('',#61417,#9024);
#6528=LINE('',#61419,#9025);
#6529=LINE('',#61420,#9026);
#6530=LINE('',#61424,#9027);
#6531=LINE('',#61426,#9028);
#6532=LINE('',#61428,#9029);
#6533=LINE('',#61430,#9030);
#6534=LINE('',#61432,#9031);
#6535=LINE('',#61433,#9032);
#6536=LINE('',#61436,#9033);
#6537=LINE('',#61438,#9034);
#6538=LINE('',#61440,#9035);
#6539=LINE('',#61441,#9036);
#6540=LINE('',#61444,#9037);
#6541=LINE('',#61446,#9038);
#6542=LINE('',#61448,#9039);
#6543=LINE('',#61449,#9040);
#6544=LINE('',#61452,#9041);
#6545=LINE('',#61453,#9042);
#6546=LINE('',#61456,#9043);
#6547=LINE('',#61458,#9044);
#6548=LINE('',#61460,#9045);
#6549=LINE('',#61461,#9046);
#6550=LINE('',#61464,#9047);
#6551=LINE('',#61466,#9048);
#6552=LINE('',#61467,#9049);
#6553=LINE('',#61471,#9050);
#6554=LINE('',#61473,#9051);
#6555=LINE('',#61475,#9052);
#6556=LINE('',#61477,#9053);
#6557=LINE('',#61479,#9054);
#6558=LINE('',#61480,#9055);
#6559=LINE('',#61483,#9056);
#6560=LINE('',#61485,#9057);
#6561=LINE('',#61487,#9058);
#6562=LINE('',#61488,#9059);
#6563=LINE('',#61491,#9060);
#6564=LINE('',#61493,#9061);
#6565=LINE('',#61495,#9062);
#6566=LINE('',#61496,#9063);
#6567=LINE('',#61499,#9064);
#6568=LINE('',#61500,#9065);
#6569=LINE('',#61503,#9066);
#6570=LINE('',#61505,#9067);
#6571=LINE('',#61507,#9068);
#6572=LINE('',#61508,#9069);
#6573=LINE('',#61511,#9070);
#6574=LINE('',#61513,#9071);
#6575=LINE('',#61514,#9072);
#6576=LINE('',#61517,#9073);
#6577=LINE('',#61519,#9074);
#6578=LINE('',#61521,#9075);
#6579=LINE('',#61523,#9076);
#6580=LINE('',#61524,#9077);
#6581=LINE('',#61527,#9078);
#6582=LINE('',#61529,#9079);
#6583=LINE('',#61530,#9080);
#6584=LINE('',#61533,#9081);
#6585=LINE('',#61534,#9082);
#6586=LINE('',#61537,#9083);
#6587=LINE('',#61539,#9084);
#6588=LINE('',#61540,#9085);
#6589=LINE('',#61544,#9086);
#6590=LINE('',#61546,#9087);
#6591=LINE('',#61548,#9088);
#6592=LINE('',#61549,#9089);
#6593=LINE('',#61552,#9090);
#6594=LINE('',#61554,#9091);
#6595=LINE('',#61555,#9092);
#6596=LINE('',#61560,#9093);
#6597=LINE('',#61562,#9094);
#6598=LINE('',#61564,#9095);
#6599=LINE('',#61565,#9096);
#6600=LINE('',#61569,#9097);
#6601=LINE('',#61570,#9098);
#6602=LINE('',#61572,#9099);
#6603=LINE('',#61574,#9100);
#6604=LINE('',#61576,#9101);
#6605=LINE('',#61577,#9102);
#6606=LINE('',#61580,#9103);
#6607=LINE('',#61581,#9104);
#6608=LINE('',#61584,#9105);
#6609=LINE('',#61586,#9106);
#6610=LINE('',#61588,#9107);
#6611=LINE('',#61590,#9108);
#6612=LINE('',#61591,#9109);
#6613=LINE('',#61594,#9110);
#6614=LINE('',#61596,#9111);
#6615=LINE('',#61598,#9112);
#6616=LINE('',#61599,#9113);
#6617=LINE('',#61601,#9114);
#6618=LINE('',#61605,#9115);
#6619=LINE('',#61607,#9116);
#6620=LINE('',#61609,#9117);
#6621=LINE('',#61611,#9118);
#6622=LINE('',#61613,#9119);
#6623=LINE('',#61614,#9120);
#6624=LINE('',#61617,#9121);
#6625=LINE('',#61618,#9122);
#6626=LINE('',#61620,#9123);
#6627=LINE('',#61621,#9124);
#6628=LINE('',#61624,#9125);
#6629=LINE('',#61626,#9126);
#6630=LINE('',#61628,#9127);
#6631=LINE('',#61629,#9128);
#6632=LINE('',#61632,#9129);
#6633=LINE('',#61633,#9130);
#6634=LINE('',#61637,#9131);
#6635=LINE('',#61639,#9132);
#6636=LINE('',#61641,#9133);
#6637=LINE('',#61643,#9134);
#6638=LINE('',#61645,#9135);
#6639=LINE('',#61646,#9136);
#6640=LINE('',#61649,#9137);
#6641=LINE('',#61651,#9138);
#6642=LINE('',#61653,#9139);
#6643=LINE('',#61654,#9140);
#6644=LINE('',#61657,#9141);
#6645=LINE('',#61659,#9142);
#6646=LINE('',#61661,#9143);
#6647=LINE('',#61662,#9144);
#6648=LINE('',#61665,#9145);
#6649=LINE('',#61666,#9146);
#6650=LINE('',#61669,#9147);
#6651=LINE('',#61671,#9148);
#6652=LINE('',#61673,#9149);
#6653=LINE('',#61674,#9150);
#6654=LINE('',#61677,#9151);
#6655=LINE('',#61679,#9152);
#6656=LINE('',#61680,#9153);
#6657=LINE('',#61684,#9154);
#6658=LINE('',#61686,#9155);
#6659=LINE('',#61688,#9156);
#6660=LINE('',#61690,#9157);
#6661=LINE('',#61692,#9158);
#6662=LINE('',#61693,#9159);
#6663=LINE('',#61696,#9160);
#6664=LINE('',#61698,#9161);
#6665=LINE('',#61700,#9162);
#6666=LINE('',#61701,#9163);
#6667=LINE('',#61704,#9164);
#6668=LINE('',#61706,#9165);
#6669=LINE('',#61708,#9166);
#6670=LINE('',#61709,#9167);
#6671=LINE('',#61712,#9168);
#6672=LINE('',#61713,#9169);
#6673=LINE('',#61716,#9170);
#6674=LINE('',#61718,#9171);
#6675=LINE('',#61720,#9172);
#6676=LINE('',#61721,#9173);
#6677=LINE('',#61724,#9174);
#6678=LINE('',#61726,#9175);
#6679=LINE('',#61727,#9176);
#6680=LINE('',#61731,#9177);
#6681=LINE('',#61733,#9178);
#6682=LINE('',#61735,#9179);
#6683=LINE('',#61737,#9180);
#6684=LINE('',#61739,#9181);
#6685=LINE('',#61740,#9182);
#6686=LINE('',#61743,#9183);
#6687=LINE('',#61745,#9184);
#6688=LINE('',#61747,#9185);
#6689=LINE('',#61748,#9186);
#6690=LINE('',#61751,#9187);
#6691=LINE('',#61753,#9188);
#6692=LINE('',#61755,#9189);
#6693=LINE('',#61756,#9190);
#6694=LINE('',#61759,#9191);
#6695=LINE('',#61760,#9192);
#6696=LINE('',#61763,#9193);
#6697=LINE('',#61765,#9194);
#6698=LINE('',#61767,#9195);
#6699=LINE('',#61768,#9196);
#6700=LINE('',#61771,#9197);
#6701=LINE('',#61773,#9198);
#6702=LINE('',#61774,#9199);
#6703=LINE('',#61778,#9200);
#6704=LINE('',#61780,#9201);
#6705=LINE('',#61782,#9202);
#6706=LINE('',#61784,#9203);
#6707=LINE('',#61786,#9204);
#6708=LINE('',#61787,#9205);
#6709=LINE('',#61790,#9206);
#6710=LINE('',#61792,#9207);
#6711=LINE('',#61794,#9208);
#6712=LINE('',#61795,#9209);
#6713=LINE('',#61798,#9210);
#6714=LINE('',#61800,#9211);
#6715=LINE('',#61802,#9212);
#6716=LINE('',#61803,#9213);
#6717=LINE('',#61806,#9214);
#6718=LINE('',#61807,#9215);
#6719=LINE('',#61810,#9216);
#6720=LINE('',#61812,#9217);
#6721=LINE('',#61814,#9218);
#6722=LINE('',#61815,#9219);
#6723=LINE('',#61818,#9220);
#6724=LINE('',#61820,#9221);
#6725=LINE('',#61821,#9222);
#6726=LINE('',#61825,#9223);
#6727=LINE('',#61827,#9224);
#6728=LINE('',#61829,#9225);
#6729=LINE('',#61831,#9226);
#6730=LINE('',#61833,#9227);
#6731=LINE('',#61834,#9228);
#6732=LINE('',#61837,#9229);
#6733=LINE('',#61839,#9230);
#6734=LINE('',#61840,#9231);
#6735=LINE('',#61843,#9232);
#6736=LINE('',#61845,#9233);
#6737=LINE('',#61846,#9234);
#6738=LINE('',#61848,#9235);
#6739=LINE('',#61849,#9236);
#6740=LINE('',#61851,#9237);
#6741=LINE('',#61852,#9238);
#6742=LINE('',#61855,#9239);
#6743=LINE('',#61856,#9240);
#6744=LINE('',#61858,#9241);
#6745=LINE('',#61860,#9242);
#6746=LINE('',#61861,#9243);
#6747=LINE('',#61864,#9244);
#6748=LINE('',#61865,#9245);
#6749=LINE('',#61868,#9246);
#6750=LINE('',#61869,#9247);
#6751=LINE('',#61871,#9248);
#6752=LINE('',#61873,#9249);
#6753=LINE('',#61874,#9250);
#6754=LINE('',#61877,#9251);
#6755=LINE('',#61878,#9252);
#6756=LINE('',#61880,#9253);
#6757=LINE('',#61883,#9254);
#6758=LINE('',#61885,#9255);
#6759=LINE('',#61887,#9256);
#6760=LINE('',#61889,#9257);
#6761=LINE('',#61891,#9258);
#6762=LINE('',#61893,#9259);
#6763=LINE('',#61895,#9260);
#6764=LINE('',#61897,#9261);
#6765=LINE('',#61899,#9262);
#6766=LINE('',#61901,#9263);
#6767=LINE('',#61903,#9264);
#6768=LINE('',#61905,#9265);
#6769=LINE('',#61907,#9266);
#6770=LINE('',#61909,#9267);
#6771=LINE('',#61911,#9268);
#6772=LINE('',#61913,#9269);
#6773=LINE('',#61915,#9270);
#6774=LINE('',#61917,#9271);
#6775=LINE('',#61919,#9272);
#6776=LINE('',#61921,#9273);
#6777=LINE('',#61923,#9274);
#6778=LINE('',#61925,#9275);
#6779=LINE('',#61927,#9276);
#6780=LINE('',#61929,#9277);
#6781=LINE('',#61931,#9278);
#6782=LINE('',#61933,#9279);
#6783=LINE('',#61935,#9280);
#6784=LINE('',#61936,#9281);
#6785=LINE('',#61937,#9282);
#6786=LINE('',#61938,#9283);
#6787=LINE('',#61940,#9284);
#6788=LINE('',#61942,#9285);
#6789=LINE('',#61944,#9286);
#6790=LINE('',#61946,#9287);
#6791=LINE('',#61948,#9288);
#6792=LINE('',#61950,#9289);
#6793=LINE('',#61952,#9290);
#6794=LINE('',#61954,#9291);
#6795=LINE('',#61956,#9292);
#6796=LINE('',#61958,#9293);
#6797=LINE('',#61960,#9294);
#6798=LINE('',#61962,#9295);
#6799=LINE('',#61964,#9296);
#6800=LINE('',#61966,#9297);
#6801=LINE('',#61968,#9298);
#6802=LINE('',#61970,#9299);
#6803=LINE('',#61972,#9300);
#6804=LINE('',#61974,#9301);
#6805=LINE('',#61976,#9302);
#6806=LINE('',#61978,#9303);
#6807=LINE('',#61980,#9304);
#6808=LINE('',#61982,#9305);
#6809=LINE('',#61984,#9306);
#6810=LINE('',#61986,#9307);
#6811=LINE('',#61988,#9308);
#6812=LINE('',#61989,#9309);
#6813=LINE('',#61990,#9310);
#6814=LINE('',#61991,#9311);
#6815=LINE('',#61992,#9312);
#6816=LINE('',#61993,#9313);
#6817=LINE('',#61995,#9314);
#6818=LINE('',#61996,#9315);
#6819=LINE('',#61997,#9316);
#6820=LINE('',#61998,#9317);
#6821=LINE('',#61999,#9318);
#6822=LINE('',#62001,#9319);
#6823=LINE('',#62003,#9320);
#6824=LINE('',#62005,#9321);
#6825=LINE('',#62007,#9322);
#6826=LINE('',#62009,#9323);
#6827=LINE('',#62010,#9324);
#6828=LINE('',#62011,#9325);
#6829=LINE('',#62012,#9326);
#6830=LINE('',#62013,#9327);
#6831=LINE('',#62014,#9328);
#6832=LINE('',#62016,#9329);
#6833=LINE('',#62019,#9330);
#6834=LINE('',#62020,#9331);
#6835=LINE('',#62022,#9332);
#6836=LINE('',#62024,#9333);
#6837=LINE('',#62027,#9334);
#6838=LINE('',#62028,#9335);
#6839=LINE('',#62031,#9336);
#6840=LINE('',#62032,#9337);
#6841=LINE('',#62034,#9338);
#6842=LINE('',#62036,#9339);
#6843=LINE('',#62039,#9340);
#6844=LINE('',#62040,#9341);
#6845=LINE('',#62043,#9342);
#6846=LINE('',#62044,#9343);
#6847=LINE('',#62046,#9344);
#6848=LINE('',#62048,#9345);
#6849=LINE('',#62051,#9346);
#6850=LINE('',#62052,#9347);
#6851=LINE('',#62055,#9348);
#6852=LINE('',#62056,#9349);
#6853=LINE('',#62058,#9350);
#6854=LINE('',#62061,#9351);
#6855=LINE('',#62062,#9352);
#6856=LINE('',#62065,#9353);
#6857=LINE('',#62066,#9354);
#6858=LINE('',#62069,#9355);
#6859=LINE('',#62070,#9356);
#6860=LINE('',#62074,#9357);
#6861=LINE('',#62076,#9358);
#6862=LINE('',#62078,#9359);
#6863=LINE('',#62079,#9360);
#6864=LINE('',#62082,#9361);
#6865=LINE('',#62083,#9362);
#6866=LINE('',#62085,#9363);
#6867=LINE('',#62086,#9364);
#6868=LINE('',#62088,#9365);
#6869=LINE('',#62089,#9366);
#6870=LINE('',#62092,#9367);
#6871=LINE('',#62094,#9368);
#6872=LINE('',#62095,#9369);
#6873=LINE('',#62098,#9370);
#6874=LINE('',#62100,#9371);
#6875=LINE('',#62101,#9372);
#6876=LINE('',#62104,#9373);
#6877=LINE('',#62105,#9374);
#6878=LINE('',#62106,#9375);
#6879=LINE('',#62109,#9376);
#6880=LINE('',#62111,#9377);
#6881=LINE('',#62113,#9378);
#6882=LINE('',#62114,#9379);
#6883=LINE('',#62117,#9380);
#6884=LINE('',#62118,#9381);
#6885=LINE('',#62122,#9382);
#6886=LINE('',#62124,#9383);
#6887=LINE('',#62126,#9384);
#6888=LINE('',#62128,#9385);
#6889=LINE('',#62130,#9386);
#6890=LINE('',#62131,#9387);
#6891=LINE('',#62133,#9388);
#6892=LINE('',#62135,#9389);
#6893=LINE('',#62136,#9390);
#6894=LINE('',#62139,#9391);
#6895=LINE('',#62141,#9392);
#6896=LINE('',#62142,#9393);
#6897=LINE('',#62145,#9394);
#6898=LINE('',#62146,#9395);
#6899=LINE('',#62149,#9396);
#6900=LINE('',#62151,#9397);
#6901=LINE('',#62153,#9398);
#6902=LINE('',#62154,#9399);
#6903=LINE('',#62156,#9400);
#6904=LINE('',#62158,#9401);
#6905=LINE('',#62160,#9402);
#6906=LINE('',#62163,#9403);
#6907=LINE('',#62164,#9404);
#6908=LINE('',#62167,#9405);
#6909=LINE('',#62168,#9406);
#6910=LINE('',#62170,#9407);
#6911=LINE('',#62172,#9408);
#6912=LINE('',#62175,#9409);
#6913=LINE('',#62176,#9410);
#6914=LINE('',#62178,#9411);
#6915=LINE('',#62180,#9412);
#6916=LINE('',#62183,#9413);
#6917=LINE('',#62184,#9414);
#6918=LINE('',#62187,#9415);
#6919=LINE('',#62188,#9416);
#6920=LINE('',#62190,#9417);
#6921=LINE('',#62192,#9418);
#6922=LINE('',#62194,#9419);
#6923=LINE('',#62197,#9420);
#6924=LINE('',#62198,#9421);
#6925=LINE('',#62200,#9422);
#6926=LINE('',#62202,#9423);
#6927=LINE('',#62205,#9424);
#6928=LINE('',#62206,#9425);
#6929=LINE('',#62208,#9426);
#6930=LINE('',#62210,#9427);
#6931=LINE('',#62213,#9428);
#6932=LINE('',#62214,#9429);
#6933=LINE('',#62216,#9430);
#6934=LINE('',#62218,#9431);
#6935=LINE('',#62221,#9432);
#6936=LINE('',#62222,#9433);
#6937=LINE('',#62224,#9434);
#6938=LINE('',#62226,#9435);
#6939=LINE('',#62229,#9436);
#6940=LINE('',#62230,#9437);
#6941=LINE('',#62233,#9438);
#6942=LINE('',#62234,#9439);
#6943=LINE('',#62236,#9440);
#6944=LINE('',#62240,#9441);
#6945=LINE('',#62242,#9442);
#6946=LINE('',#62244,#9443);
#6947=LINE('',#62246,#9444);
#6948=LINE('',#62248,#9445);
#6949=LINE('',#62249,#9446);
#6950=LINE('',#62251,#9447);
#6951=LINE('',#62253,#9448);
#6952=LINE('',#62254,#9449);
#6953=LINE('',#62257,#9450);
#6954=LINE('',#62259,#9451);
#6955=LINE('',#62260,#9452);
#6956=LINE('',#62263,#9453);
#6957=LINE('',#62264,#9454);
#6958=LINE('',#62267,#9455);
#6959=LINE('',#62269,#9456);
#6960=LINE('',#62271,#9457);
#6961=LINE('',#62272,#9458);
#6962=LINE('',#62275,#9459);
#6963=LINE('',#62276,#9460);
#6964=LINE('',#62280,#9461);
#6965=LINE('',#62282,#9462);
#6966=LINE('',#62284,#9463);
#6967=LINE('',#62286,#9464);
#6968=LINE('',#62288,#9465);
#6969=LINE('',#62289,#9466);
#6970=LINE('',#62291,#9467);
#6971=LINE('',#62293,#9468);
#6972=LINE('',#62294,#9469);
#6973=LINE('',#62297,#9470);
#6974=LINE('',#62299,#9471);
#6975=LINE('',#62300,#9472);
#6976=LINE('',#62303,#9473);
#6977=LINE('',#62304,#9474);
#6978=LINE('',#62307,#9475);
#6979=LINE('',#62309,#9476);
#6980=LINE('',#62311,#9477);
#6981=LINE('',#62312,#9478);
#6982=LINE('',#62315,#9479);
#6983=LINE('',#62316,#9480);
#6984=LINE('',#62320,#9481);
#6985=LINE('',#62322,#9482);
#6986=LINE('',#62324,#9483);
#6987=LINE('',#62326,#9484);
#6988=LINE('',#62328,#9485);
#6989=LINE('',#62329,#9486);
#6990=LINE('',#62331,#9487);
#6991=LINE('',#62333,#9488);
#6992=LINE('',#62334,#9489);
#6993=LINE('',#62337,#9490);
#6994=LINE('',#62339,#9491);
#6995=LINE('',#62340,#9492);
#6996=LINE('',#62343,#9493);
#6997=LINE('',#62344,#9494);
#6998=LINE('',#62347,#9495);
#6999=LINE('',#62349,#9496);
#7000=LINE('',#62351,#9497);
#7001=LINE('',#62352,#9498);
#7002=LINE('',#62355,#9499);
#7003=LINE('',#62356,#9500);
#7004=LINE('',#62360,#9501);
#7005=LINE('',#62362,#9502);
#7006=LINE('',#62364,#9503);
#7007=LINE('',#62366,#9504);
#7008=LINE('',#62368,#9505);
#7009=LINE('',#62369,#9506);
#7010=LINE('',#62372,#9507);
#7011=LINE('',#62374,#9508);
#7012=LINE('',#62375,#9509);
#7013=LINE('',#62377,#9510);
#7014=LINE('',#62378,#9511);
#7015=LINE('',#62381,#9512);
#7016=LINE('',#62383,#9513);
#7017=LINE('',#62384,#9514);
#7018=LINE('',#62387,#9515);
#7019=LINE('',#62389,#9516);
#7020=LINE('',#62391,#9517);
#7021=LINE('',#62393,#9518);
#7022=LINE('',#62394,#9519);
#7023=LINE('',#62397,#9520);
#7024=LINE('',#62399,#9521);
#7025=LINE('',#62400,#9522);
#7026=LINE('',#62403,#9523);
#7027=LINE('',#62405,#9524);
#7028=LINE('',#62406,#9525);
#7029=LINE('',#62409,#9526);
#7030=LINE('',#62410,#9527);
#7031=LINE('',#62411,#9528);
#7032=LINE('',#62415,#9529);
#7033=LINE('',#62417,#9530);
#7034=LINE('',#62419,#9531);
#7035=LINE('',#62421,#9532);
#7036=LINE('',#62423,#9533);
#7037=LINE('',#62424,#9534);
#7038=LINE('',#62426,#9535);
#7039=LINE('',#62428,#9536);
#7040=LINE('',#62429,#9537);
#7041=LINE('',#62432,#9538);
#7042=LINE('',#62434,#9539);
#7043=LINE('',#62435,#9540);
#7044=LINE('',#62438,#9541);
#7045=LINE('',#62439,#9542);
#7046=LINE('',#62442,#9543);
#7047=LINE('',#62444,#9544);
#7048=LINE('',#62446,#9545);
#7049=LINE('',#62447,#9546);
#7050=LINE('',#62450,#9547);
#7051=LINE('',#62451,#9548);
#7052=LINE('',#62455,#9549);
#7053=LINE('',#62457,#9550);
#7054=LINE('',#62459,#9551);
#7055=LINE('',#62461,#9552);
#7056=LINE('',#62463,#9553);
#7057=LINE('',#62464,#9554);
#7058=LINE('',#62466,#9555);
#7059=LINE('',#62468,#9556);
#7060=LINE('',#62469,#9557);
#7061=LINE('',#62472,#9558);
#7062=LINE('',#62474,#9559);
#7063=LINE('',#62475,#9560);
#7064=LINE('',#62478,#9561);
#7065=LINE('',#62479,#9562);
#7066=LINE('',#62482,#9563);
#7067=LINE('',#62484,#9564);
#7068=LINE('',#62486,#9565);
#7069=LINE('',#62487,#9566);
#7070=LINE('',#62490,#9567);
#7071=LINE('',#62491,#9568);
#7072=LINE('',#62494,#9569);
#7073=LINE('',#62496,#9570);
#7074=LINE('',#62498,#9571);
#7075=LINE('',#62499,#9572);
#7076=LINE('',#62502,#9573);
#7077=LINE('',#62504,#9574);
#7078=LINE('',#62506,#9575);
#7079=LINE('',#62507,#9576);
#7080=LINE('',#62510,#9577);
#7081=LINE('',#62511,#9578);
#7082=LINE('',#62513,#9579);
#7083=LINE('',#62515,#9580);
#7084=LINE('',#62518,#9581);
#7085=LINE('',#62519,#9582);
#7086=LINE('',#62521,#9583);
#7087=LINE('',#62523,#9584);
#7088=LINE('',#62526,#9585);
#7089=LINE('',#62527,#9586);
#7090=LINE('',#62530,#9587);
#7091=LINE('',#62531,#9588);
#7092=LINE('',#62533,#9589);
#7093=LINE('',#62535,#9590);
#7094=LINE('',#62537,#9591);
#7095=LINE('',#62540,#9592);
#7096=LINE('',#62541,#9593);
#7097=LINE('',#62543,#9594);
#7098=LINE('',#62545,#9595);
#7099=LINE('',#62548,#9596);
#7100=LINE('',#62549,#9597);
#7101=LINE('',#62551,#9598);
#7102=LINE('',#62553,#9599);
#7103=LINE('',#62556,#9600);
#7104=LINE('',#62557,#9601);
#7105=LINE('',#62560,#9602);
#7106=LINE('',#62561,#9603);
#7107=LINE('',#62563,#9604);
#7108=LINE('',#62565,#9605);
#7109=LINE('',#62568,#9606);
#7110=LINE('',#62569,#9607);
#7111=LINE('',#62572,#9608);
#7112=LINE('',#62573,#9609);
#7113=LINE('',#62575,#9610);
#7114=LINE('',#62577,#9611);
#7115=LINE('',#62580,#9612);
#7116=LINE('',#62581,#9613);
#7117=LINE('',#62583,#9614);
#7118=LINE('',#62585,#9615);
#7119=LINE('',#62588,#9616);
#7120=LINE('',#62589,#9617);
#7121=LINE('',#62591,#9618);
#7122=LINE('',#62593,#9619);
#7123=LINE('',#62596,#9620);
#7124=LINE('',#62597,#9621);
#7125=LINE('',#62600,#9622);
#7126=LINE('',#62601,#9623);
#7127=LINE('',#62603,#9624);
#7128=LINE('',#62607,#9625);
#7129=LINE('',#62609,#9626);
#7130=LINE('',#62611,#9627);
#7131=LINE('',#62613,#9628);
#7132=LINE('',#62615,#9629);
#7133=LINE('',#62616,#9630);
#7134=LINE('',#62618,#9631);
#7135=LINE('',#62620,#9632);
#7136=LINE('',#62621,#9633);
#7137=LINE('',#62624,#9634);
#7138=LINE('',#62626,#9635);
#7139=LINE('',#62627,#9636);
#7140=LINE('',#62630,#9637);
#7141=LINE('',#62631,#9638);
#7142=LINE('',#62634,#9639);
#7143=LINE('',#62636,#9640);
#7144=LINE('',#62638,#9641);
#7145=LINE('',#62639,#9642);
#7146=LINE('',#62642,#9643);
#7147=LINE('',#62643,#9644);
#7148=LINE('',#62647,#9645);
#7149=LINE('',#62649,#9646);
#7150=LINE('',#62651,#9647);
#7151=LINE('',#62653,#9648);
#7152=LINE('',#62655,#9649);
#7153=LINE('',#62656,#9650);
#7154=LINE('',#62658,#9651);
#7155=LINE('',#62660,#9652);
#7156=LINE('',#62661,#9653);
#7157=LINE('',#62664,#9654);
#7158=LINE('',#62666,#9655);
#7159=LINE('',#62667,#9656);
#7160=LINE('',#62670,#9657);
#7161=LINE('',#62671,#9658);
#7162=LINE('',#62674,#9659);
#7163=LINE('',#62676,#9660);
#7164=LINE('',#62678,#9661);
#7165=LINE('',#62679,#9662);
#7166=LINE('',#62682,#9663);
#7167=LINE('',#62683,#9664);
#7168=LINE('',#62687,#9665);
#7169=LINE('',#62689,#9666);
#7170=LINE('',#62691,#9667);
#7171=LINE('',#62693,#9668);
#7172=LINE('',#62695,#9669);
#7173=LINE('',#62696,#9670);
#7174=LINE('',#62698,#9671);
#7175=LINE('',#62700,#9672);
#7176=LINE('',#62701,#9673);
#7177=LINE('',#62704,#9674);
#7178=LINE('',#62706,#9675);
#7179=LINE('',#62707,#9676);
#7180=LINE('',#62710,#9677);
#7181=LINE('',#62711,#9678);
#7182=LINE('',#62714,#9679);
#7183=LINE('',#62716,#9680);
#7184=LINE('',#62718,#9681);
#7185=LINE('',#62719,#9682);
#7186=LINE('',#62722,#9683);
#7187=LINE('',#62723,#9684);
#7188=LINE('',#62727,#9685);
#7189=LINE('',#62729,#9686);
#7190=LINE('',#62731,#9687);
#7191=LINE('',#62733,#9688);
#7192=LINE('',#62735,#9689);
#7193=LINE('',#62736,#9690);
#7194=LINE('',#62738,#9691);
#7195=LINE('',#62740,#9692);
#7196=LINE('',#62741,#9693);
#7197=LINE('',#62744,#9694);
#7198=LINE('',#62746,#9695);
#7199=LINE('',#62747,#9696);
#7200=LINE('',#62750,#9697);
#7201=LINE('',#62751,#9698);
#7202=LINE('',#62754,#9699);
#7203=LINE('',#62756,#9700);
#7204=LINE('',#62758,#9701);
#7205=LINE('',#62759,#9702);
#7206=LINE('',#62762,#9703);
#7207=LINE('',#62763,#9704);
#7208=LINE('',#62767,#9705);
#7209=LINE('',#62769,#9706);
#7210=LINE('',#62771,#9707);
#7211=LINE('',#62773,#9708);
#7212=LINE('',#62775,#9709);
#7213=LINE('',#62776,#9710);
#7214=LINE('',#62778,#9711);
#7215=LINE('',#62780,#9712);
#7216=LINE('',#62781,#9713);
#7217=LINE('',#62784,#9714);
#7218=LINE('',#62786,#9715);
#7219=LINE('',#62787,#9716);
#7220=LINE('',#62790,#9717);
#7221=LINE('',#62791,#9718);
#7222=LINE('',#62794,#9719);
#7223=LINE('',#62796,#9720);
#7224=LINE('',#62798,#9721);
#7225=LINE('',#62799,#9722);
#7226=LINE('',#62802,#9723);
#7227=LINE('',#62803,#9724);
#7228=LINE('',#62807,#9725);
#7229=LINE('',#62809,#9726);
#7230=LINE('',#62811,#9727);
#7231=LINE('',#62813,#9728);
#7232=LINE('',#62815,#9729);
#7233=LINE('',#62816,#9730);
#7234=LINE('',#62818,#9731);
#7235=LINE('',#62820,#9732);
#7236=LINE('',#62821,#9733);
#7237=LINE('',#62824,#9734);
#7238=LINE('',#62826,#9735);
#7239=LINE('',#62827,#9736);
#7240=LINE('',#62830,#9737);
#7241=LINE('',#62831,#9738);
#7242=LINE('',#62834,#9739);
#7243=LINE('',#62836,#9740);
#7244=LINE('',#62838,#9741);
#7245=LINE('',#62839,#9742);
#7246=LINE('',#62842,#9743);
#7247=LINE('',#62843,#9744);
#7248=LINE('',#62846,#9745);
#7249=LINE('',#62848,#9746);
#7250=LINE('',#62850,#9747);
#7251=LINE('',#62851,#9748);
#7252=LINE('',#62854,#9749);
#7253=LINE('',#62856,#9750);
#7254=LINE('',#62858,#9751);
#7255=LINE('',#62859,#9752);
#7256=LINE('',#62862,#9753);
#7257=LINE('',#62863,#9754);
#7258=LINE('',#62865,#9755);
#7259=LINE('',#62867,#9756);
#7260=LINE('',#62870,#9757);
#7261=LINE('',#62871,#9758);
#7262=LINE('',#62873,#9759);
#7263=LINE('',#62875,#9760);
#7264=LINE('',#62878,#9761);
#7265=LINE('',#62879,#9762);
#7266=LINE('',#62882,#9763);
#7267=LINE('',#62883,#9764);
#7268=LINE('',#62885,#9765);
#7269=LINE('',#62887,#9766);
#7270=LINE('',#62890,#9767);
#7271=LINE('',#62891,#9768);
#7272=LINE('',#62894,#9769);
#7273=LINE('',#62895,#9770);
#7274=LINE('',#62897,#9771);
#7275=LINE('',#62899,#9772);
#7276=LINE('',#62902,#9773);
#7277=LINE('',#62903,#9774);
#7278=LINE('',#62906,#9775);
#7279=LINE('',#62907,#9776);
#7280=LINE('',#62909,#9777);
#7281=LINE('',#62911,#9778);
#7282=LINE('',#62914,#9779);
#7283=LINE('',#62915,#9780);
#7284=LINE('',#62918,#9781);
#7285=LINE('',#62919,#9782);
#7286=LINE('',#62921,#9783);
#7287=LINE('',#62923,#9784);
#7288=LINE('',#62926,#9785);
#7289=LINE('',#62927,#9786);
#7290=LINE('',#62930,#9787);
#7291=LINE('',#62931,#9788);
#7292=LINE('',#62933,#9789);
#7293=LINE('',#62935,#9790);
#7294=LINE('',#62936,#9791);
#7295=LINE('',#62939,#9792);
#7296=LINE('',#62940,#9793);
#7297=LINE('',#62942,#9794);
#7298=LINE('',#62944,#9795);
#7299=LINE('',#62947,#9796);
#7300=LINE('',#62949,#9797);
#7301=LINE('',#62950,#9798);
#7302=LINE('',#62953,#9799);
#7303=LINE('',#62954,#9800);
#7304=LINE('',#62957,#9801);
#7305=LINE('',#62958,#9802);
#7306=LINE('',#62961,#9803);
#7307=LINE('',#62963,#9804);
#7308=LINE('',#62965,#9805);
#7309=LINE('',#62967,#9806);
#7310=LINE('',#62969,#9807);
#7311=LINE('',#62971,#9808);
#7312=LINE('',#62973,#9809);
#7313=LINE('',#62975,#9810);
#7314=LINE('',#62976,#9811);
#7315=LINE('',#62978,#9812);
#7316=LINE('',#62979,#9813);
#7317=LINE('',#62981,#9814);
#7318=LINE('',#62983,#9815);
#7319=LINE('',#62985,#9816);
#7320=LINE('',#62987,#9817);
#7321=LINE('',#62989,#9818);
#7322=LINE('',#62991,#9819);
#7323=LINE('',#62993,#9820);
#7324=LINE('',#62995,#9821);
#7325=LINE('',#62996,#9822);
#7326=LINE('',#62998,#9823);
#7327=LINE('',#63000,#9824);
#7328=LINE('',#63002,#9825);
#7329=LINE('',#63004,#9826);
#7330=LINE('',#63006,#9827);
#7331=LINE('',#63007,#9828);
#7332=LINE('',#63009,#9829);
#7333=LINE('',#63011,#9830);
#7334=LINE('',#63013,#9831);
#7335=LINE('',#63015,#9832);
#7336=LINE('',#63017,#9833);
#7337=LINE('',#63019,#9834);
#7338=LINE('',#63021,#9835);
#7339=LINE('',#63023,#9836);
#7340=LINE('',#63024,#9837);
#7341=LINE('',#63026,#9838);
#7342=LINE('',#63028,#9839);
#7343=LINE('',#63030,#9840);
#7344=LINE('',#63032,#9841);
#7345=LINE('',#63034,#9842);
#7346=LINE('',#63036,#9843);
#7347=LINE('',#63038,#9844);
#7348=LINE('',#63040,#9845);
#7349=LINE('',#63041,#9846);
#7350=LINE('',#63043,#9847);
#7351=LINE('',#63045,#9848);
#7352=LINE('',#63047,#9849);
#7353=LINE('',#63049,#9850);
#7354=LINE('',#63051,#9851);
#7355=LINE('',#63053,#9852);
#7356=LINE('',#63055,#9853);
#7357=LINE('',#63057,#9854);
#7358=LINE('',#63059,#9855);
#7359=LINE('',#63061,#9856);
#7360=LINE('',#63063,#9857);
#7361=LINE('',#63065,#9858);
#7362=LINE('',#63067,#9859);
#7363=LINE('',#63068,#9860);
#7364=LINE('',#63070,#9861);
#7365=LINE('',#63072,#9862);
#7366=LINE('',#63074,#9863);
#7367=LINE('',#63076,#9864);
#7368=LINE('',#63078,#9865);
#7369=LINE('',#63080,#9866);
#7370=LINE('',#63082,#9867);
#7371=LINE('',#63084,#9868);
#7372=LINE('',#63085,#9869);
#7373=LINE('',#63087,#9870);
#7374=LINE('',#63089,#9871);
#7375=LINE('',#63091,#9872);
#7376=LINE('',#63093,#9873);
#7377=LINE('',#63095,#9874);
#7378=LINE('',#63097,#9875);
#7379=LINE('',#63099,#9876);
#7380=LINE('',#63101,#9877);
#7381=LINE('',#63103,#9878);
#7382=LINE('',#63105,#9879);
#7383=LINE('',#63107,#9880);
#7384=LINE('',#63109,#9881);
#7385=LINE('',#63111,#9882);
#7386=LINE('',#63113,#9883);
#7387=LINE('',#63115,#9884);
#7388=LINE('',#63117,#9885);
#7389=LINE('',#63119,#9886);
#7390=LINE('',#63121,#9887);
#7391=LINE('',#63123,#9888);
#7392=LINE('',#63125,#9889);
#7393=LINE('',#63127,#9890);
#7394=LINE('',#63129,#9891);
#7395=LINE('',#63131,#9892);
#7396=LINE('',#63133,#9893);
#7397=LINE('',#63134,#9894);
#7398=LINE('',#63136,#9895);
#7399=LINE('',#63138,#9896);
#7400=LINE('',#63140,#9897);
#7401=LINE('',#63142,#9898);
#7402=LINE('',#63144,#9899);
#7403=LINE('',#63146,#9900);
#7404=LINE('',#63148,#9901);
#7405=LINE('',#63150,#9902);
#7406=LINE('',#63151,#9903);
#7407=LINE('',#63153,#9904);
#7408=LINE('',#63155,#9905);
#7409=LINE('',#63157,#9906);
#7410=LINE('',#63159,#9907);
#7411=LINE('',#63161,#9908);
#7412=LINE('',#63163,#9909);
#7413=LINE('',#63165,#9910);
#7414=LINE('',#63167,#9911);
#7415=LINE('',#63169,#9912);
#7416=LINE('',#63171,#9913);
#7417=LINE('',#63173,#9914);
#7418=LINE('',#63175,#9915);
#7419=LINE('',#63176,#9916);
#7420=LINE('',#63180,#9917);
#7421=LINE('',#63182,#9918);
#7422=LINE('',#63183,#9919);
#7423=LINE('',#63185,#9920);
#7424=LINE('',#63187,#9921);
#7425=LINE('',#63190,#9922);
#7426=LINE('',#63191,#9923);
#7427=LINE('',#63193,#9924);
#7428=LINE('',#63195,#9925);
#7429=LINE('',#63198,#9926);
#7430=LINE('',#63199,#9927);
#7431=LINE('',#63201,#9928);
#7432=LINE('',#63203,#9929);
#7433=LINE('',#63206,#9930);
#7434=LINE('',#63208,#9931);
#7435=LINE('',#63210,#9932);
#7436=LINE('',#63212,#9933);
#7437=LINE('',#63213,#9934);
#7438=LINE('',#63215,#9935);
#7439=LINE('',#63217,#9936);
#7440=LINE('',#63220,#9937);
#7441=LINE('',#63221,#9938);
#7442=LINE('',#63224,#9939);
#7443=LINE('',#63226,#9940);
#7444=LINE('',#63228,#9941);
#7445=LINE('',#63229,#9942);
#7446=LINE('',#63231,#9943);
#7447=LINE('',#63233,#9944);
#7448=LINE('',#63236,#9945);
#7449=LINE('',#63237,#9946);
#7450=LINE('',#63239,#9947);
#7451=LINE('',#63241,#9948);
#7452=LINE('',#63244,#9949);
#7453=LINE('',#63245,#9950);
#7454=LINE('',#63247,#9951);
#7455=LINE('',#63249,#9952);
#7456=LINE('',#63252,#9953);
#7457=LINE('',#63253,#9954);
#7458=LINE('',#63255,#9955);
#7459=LINE('',#63257,#9956);
#7460=LINE('',#63260,#9957);
#7461=LINE('',#63261,#9958);
#7462=LINE('',#63263,#9959);
#7463=LINE('',#63265,#9960);
#7464=LINE('',#63268,#9961);
#7465=LINE('',#63269,#9962);
#7466=LINE('',#63273,#9963);
#7467=LINE('',#63274,#9964);
#7468=LINE('',#63276,#9965);
#7469=LINE('',#63278,#9966);
#7470=LINE('',#63281,#9967);
#7471=LINE('',#63282,#9968);
#7472=LINE('',#63284,#9969);
#7473=LINE('',#63286,#9970);
#7474=LINE('',#63289,#9971);
#7475=LINE('',#63291,#9972);
#7476=LINE('',#63293,#9973);
#7477=LINE('',#63295,#9974);
#7478=LINE('',#63296,#9975);
#7479=LINE('',#63298,#9976);
#7480=LINE('',#63300,#9977);
#7481=LINE('',#63303,#9978);
#7482=LINE('',#63304,#9979);
#7483=LINE('',#63306,#9980);
#7484=LINE('',#63308,#9981);
#7485=LINE('',#63311,#9982);
#7486=LINE('',#63312,#9983);
#7487=LINE('',#63314,#9984);
#7488=LINE('',#63317,#9985);
#7489=LINE('',#63319,#9986);
#7490=LINE('',#63321,#9987);
#7491=LINE('',#63322,#9988);
#7492=LINE('',#63324,#9989);
#7493=LINE('',#63326,#9990);
#7494=LINE('',#63329,#9991);
#7495=LINE('',#63330,#9992);
#7496=LINE('',#63334,#9993);
#7497=LINE('',#63335,#9994);
#7498=LINE('',#63337,#9995);
#7499=LINE('',#63339,#9996);
#7500=LINE('',#63342,#9997);
#7501=LINE('',#63343,#9998);
#7502=LINE('',#63345,#9999);
#7503=LINE('',#63347,#10000);
#7504=LINE('',#63350,#10001);
#7505=LINE('',#63352,#10002);
#7506=LINE('',#63354,#10003);
#7507=LINE('',#63356,#10004);
#7508=LINE('',#63357,#10005);
#7509=LINE('',#63359,#10006);
#7510=LINE('',#63362,#10007);
#7511=LINE('',#63364,#10008);
#7512=LINE('',#63366,#10009);
#7513=LINE('',#63367,#10010);
#7514=LINE('',#63369,#10011);
#7515=LINE('',#63371,#10012);
#7516=LINE('',#63374,#10013);
#7517=LINE('',#63375,#10014);
#7518=LINE('',#63380,#10015);
#7519=LINE('',#63381,#10016);
#7520=LINE('',#63383,#10017);
#7521=LINE('',#63384,#10018);
#7522=LINE('',#63386,#10019);
#7523=LINE('',#63388,#10020);
#7524=LINE('',#63391,#10021);
#7525=LINE('',#63392,#10022);
#7526=LINE('',#63394,#10023);
#7527=LINE('',#63559,#10024);
#7528=LINE('',#63648,#10025);
#7529=LINE('',#63653,#10026);
#7530=LINE('',#63656,#10027);
#7531=LINE('',#63658,#10028);
#7532=LINE('',#63661,#10029);
#7533=LINE('',#63664,#10030);
#7534=LINE('',#63665,#10031);
#7535=LINE('',#63667,#10032);
#7536=LINE('',#63670,#10033);
#7537=LINE('',#63671,#10034);
#7538=LINE('',#63679,#10035);
#7539=LINE('',#63685,#10036);
#7540=LINE('',#63686,#10037);
#7541=LINE('',#63688,#10038);
#7542=LINE('',#63690,#10039);
#7543=LINE('',#63698,#10040);
#7544=LINE('',#63700,#10041);
#7545=LINE('',#63702,#10042);
#7546=LINE('',#63703,#10043);
#7547=LINE('',#63708,#10044);
#7548=LINE('',#63712,#10045);
#7549=LINE('',#63714,#10046);
#7550=LINE('',#63715,#10047);
#7551=LINE('',#63719,#10048);
#7552=LINE('',#63721,#10049);
#7553=LINE('',#63723,#10050);
#7554=LINE('',#63724,#10051);
#7555=LINE('',#63729,#10052);
#7556=LINE('',#63733,#10053);
#7557=LINE('',#63735,#10054);
#7558=LINE('',#63736,#10055);
#7559=LINE('',#63740,#10056);
#7560=LINE('',#63742,#10057);
#7561=LINE('',#63744,#10058);
#7562=LINE('',#63745,#10059);
#7563=LINE('',#63750,#10060);
#7564=LINE('',#63754,#10061);
#7565=LINE('',#63756,#10062);
#7566=LINE('',#63757,#10063);
#7567=LINE('',#63761,#10064);
#7568=LINE('',#63763,#10065);
#7569=LINE('',#63765,#10066);
#7570=LINE('',#63766,#10067);
#7571=LINE('',#63771,#10068);
#7572=LINE('',#63775,#10069);
#7573=LINE('',#63777,#10070);
#7574=LINE('',#63778,#10071);
#7575=LINE('',#63782,#10072);
#7576=LINE('',#63784,#10073);
#7577=LINE('',#63786,#10074);
#7578=LINE('',#63787,#10075);
#7579=LINE('',#63792,#10076);
#7580=LINE('',#63796,#10077);
#7581=LINE('',#63798,#10078);
#7582=LINE('',#63799,#10079);
#7583=LINE('',#63803,#10080);
#7584=LINE('',#63805,#10081);
#7585=LINE('',#63807,#10082);
#7586=LINE('',#63808,#10083);
#7587=LINE('',#63813,#10084);
#7588=LINE('',#63817,#10085);
#7589=LINE('',#63819,#10086);
#7590=LINE('',#63820,#10087);
#7591=LINE('',#63824,#10088);
#7592=LINE('',#63826,#10089);
#7593=LINE('',#63828,#10090);
#7594=LINE('',#63829,#10091);
#7595=LINE('',#63834,#10092);
#7596=LINE('',#63838,#10093);
#7597=LINE('',#63840,#10094);
#7598=LINE('',#63841,#10095);
#7599=LINE('',#63845,#10096);
#7600=LINE('',#63847,#10097);
#7601=LINE('',#63849,#10098);
#7602=LINE('',#63850,#10099);
#7603=LINE('',#63855,#10100);
#7604=LINE('',#63859,#10101);
#7605=LINE('',#63861,#10102);
#7606=LINE('',#63862,#10103);
#7607=LINE('',#63903,#10104);
#7608=LINE('',#63910,#10105);
#7609=LINE('',#63914,#10106);
#7610=LINE('',#63921,#10107);
#7611=LINE('',#63925,#10108);
#7612=LINE('',#63926,#10109);
#7613=LINE('',#63969,#10110);
#7614=LINE('',#63972,#10111);
#7615=LINE('',#63989,#10112);
#7616=LINE('',#63993,#10113);
#7617=LINE('',#64017,#10114);
#7618=LINE('',#64019,#10115);
#7619=LINE('',#64020,#10116);
#7620=LINE('',#64023,#10117);
#7621=LINE('',#64025,#10118);
#7622=LINE('',#64027,#10119);
#7623=LINE('',#64030,#10120);
#7624=LINE('',#64034,#10121);
#7625=LINE('',#64036,#10122);
#7626=LINE('',#64043,#10123);
#7627=LINE('',#64047,#10124);
#7628=LINE('',#64051,#10125);
#7629=LINE('',#64053,#10126);
#7630=LINE('',#64055,#10127);
#7631=LINE('',#64057,#10128);
#7632=LINE('',#64058,#10129);
#7633=LINE('',#64061,#10130);
#7634=LINE('',#64063,#10131);
#7635=LINE('',#64064,#10132);
#7636=LINE('',#64067,#10133);
#7637=LINE('',#64068,#10134);
#7638=LINE('',#64074,#10135);
#7639=LINE('',#64079,#10136);
#7640=LINE('',#64082,#10137);
#7641=LINE('',#64084,#10138);
#7642=LINE('',#64085,#10139);
#7643=LINE('',#64088,#10140);
#7644=LINE('',#64090,#10141);
#7645=LINE('',#64092,#10142);
#7646=LINE('',#64094,#10143);
#7647=LINE('',#64095,#10144);
#7648=LINE('',#64100,#10145);
#7649=LINE('',#64110,#10146);
#7650=LINE('',#64119,#10147);
#7651=LINE('',#64123,#10148);
#7652=LINE('',#64126,#10149);
#7653=LINE('',#64127,#10150);
#7654=LINE('',#64130,#10151);
#7655=LINE('',#64134,#10152);
#7656=LINE('',#64136,#10153);
#7657=LINE('',#64140,#10154);
#7658=LINE('',#64148,#10155);
#7659=LINE('',#64151,#10156);
#7660=LINE('',#64153,#10157);
#7661=LINE('',#64156,#10158);
#7662=LINE('',#64157,#10159);
#7663=LINE('',#64160,#10160);
#7664=LINE('',#64164,#10161);
#7665=LINE('',#64165,#10162);
#7666=LINE('',#64168,#10163);
#7667=LINE('',#64172,#10164);
#7668=LINE('',#64176,#10165);
#7669=LINE('',#64180,#10166);
#7670=LINE('',#64192,#10167);
#7671=LINE('',#64194,#10168);
#7672=LINE('',#64196,#10169);
#7673=LINE('',#64198,#10170);
#7674=LINE('',#64199,#10171);
#7675=LINE('',#64203,#10172);
#7676=LINE('',#64205,#10173);
#7677=LINE('',#64215,#10174);
#7678=LINE('',#64230,#10175);
#7679=LINE('',#64242,#10176);
#7680=LINE('',#64250,#10177);
#7681=LINE('',#64267,#10178);
#7682=LINE('',#64268,#10179);
#7683=LINE('',#64282,#10180);
#7684=LINE('',#64283,#10181);
#7685=LINE('',#64335,#10182);
#7686=LINE('',#64336,#10183);
#7687=LINE('',#64341,#10184);
#7688=LINE('',#64344,#10185);
#7689=LINE('',#64347,#10186);
#7690=LINE('',#64349,#10187);
#7691=LINE('',#64351,#10188);
#7692=LINE('',#64353,#10189);
#7693=LINE('',#64354,#10190);
#7694=LINE('',#64369,#10191);
#7695=LINE('',#64372,#10192);
#7696=LINE('',#64383,#10193);
#7697=LINE('',#64387,#10194);
#7698=LINE('',#64389,#10195);
#7699=LINE('',#64396,#10196);
#7700=LINE('',#64407,#10197);
#7701=LINE('',#64411,#10198);
#7702=LINE('',#64421,#10199);
#7703=LINE('',#64426,#10200);
#7704=LINE('',#64428,#10201);
#7705=LINE('',#64429,#10202);
#7706=LINE('',#64438,#10203);
#7707=LINE('',#64442,#10204);
#7708=LINE('',#64445,#10205);
#7709=LINE('',#64450,#10206);
#7710=LINE('',#64453,#10207);
#7711=LINE('',#64464,#10208);
#7712=LINE('',#64468,#10209);
#7713=LINE('',#64483,#10210);
#7714=LINE('',#64485,#10211);
#7715=LINE('',#64496,#10212);
#7716=LINE('',#64498,#10213);
#7717=LINE('',#64499,#10214);
#7718=LINE('',#64502,#10215);
#7719=LINE('',#64513,#10216);
#7720=LINE('',#64517,#10217);
#7721=LINE('',#64527,#10218);
#7722=LINE('',#64541,#10219);
#7723=LINE('',#64561,#10220);
#7724=LINE('',#64563,#10221);
#7725=LINE('',#64565,#10222);
#7726=LINE('',#64585,#10223);
#7727=LINE('',#64587,#10224);
#7728=LINE('',#64589,#10225);
#7729=LINE('',#64590,#10226);
#7730=LINE('',#64592,#10227);
#7731=LINE('',#64594,#10228);
#7732=LINE('',#64596,#10229);
#7733=LINE('',#64598,#10230);
#7734=LINE('',#64607,#10231);
#7735=LINE('',#64617,#10232);
#7736=LINE('',#64627,#10233);
#7737=LINE('',#64665,#10234);
#7738=LINE('',#64669,#10235);
#7739=LINE('',#64673,#10236);
#7740=LINE('',#64695,#10237);
#7741=LINE('',#64730,#10238);
#7742=LINE('',#64734,#10239);
#7743=LINE('',#64736,#10240);
#7744=LINE('',#64738,#10241);
#7745=LINE('',#64740,#10242);
#7746=LINE('',#64741,#10243);
#7747=LINE('',#64743,#10244);
#7748=LINE('',#64745,#10245);
#7749=LINE('',#64746,#10246);
#7750=LINE('',#64761,#10247);
#7751=LINE('',#64802,#10248);
#7752=LINE('',#64805,#10249);
#7753=LINE('',#64808,#10250);
#7754=LINE('',#64810,#10251);
#7755=LINE('',#64811,#10252);
#7756=LINE('',#64846,#10253);
#7757=LINE('',#64849,#10254);
#7758=LINE('',#64852,#10255);
#7759=LINE('',#64853,#10256);
#7760=LINE('',#64863,#10257);
#7761=LINE('',#64867,#10258);
#7762=LINE('',#64871,#10259);
#7763=LINE('',#64883,#10260);
#7764=LINE('',#64885,#10261);
#7765=LINE('',#64887,#10262);
#7766=LINE('',#64888,#10263);
#7767=LINE('',#64889,#10264);
#7768=LINE('',#64891,#10265);
#7769=LINE('',#64893,#10266);
#7770=LINE('',#64895,#10267);
#7771=LINE('',#64897,#10268);
#7772=LINE('',#64898,#10269);
#7773=LINE('',#64899,#10270);
#7774=LINE('',#64918,#10271);
#7775=LINE('',#64922,#10272);
#7776=LINE('',#64931,#10273);
#7777=LINE('',#64939,#10274);
#7778=LINE('',#64942,#10275);
#7779=LINE('',#64945,#10276);
#7780=LINE('',#64947,#10277);
#7781=LINE('',#64948,#10278);
#7782=LINE('',#64961,#10279);
#7783=LINE('',#64963,#10280);
#7784=LINE('',#64964,#10281);
#7785=LINE('',#64966,#10282);
#7786=LINE('',#64968,#10283);
#7787=LINE('',#64969,#10284);
#7788=LINE('',#64971,#10285);
#7789=LINE('',#64976,#10286);
#7790=LINE('',#64983,#10287);
#7791=LINE('',#64988,#10288);
#7792=LINE('',#64990,#10289);
#7793=LINE('',#64991,#10290);
#7794=LINE('',#64993,#10291);
#7795=LINE('',#64999,#10292);
#7796=LINE('',#65013,#10293);
#7797=LINE('',#65019,#10294);
#7798=LINE('',#65032,#10295);
#7799=LINE('',#65036,#10296);
#7800=LINE('',#65040,#10297);
#7801=LINE('',#65043,#10298);
#7802=LINE('',#65048,#10299);
#7803=LINE('',#65051,#10300);
#7804=LINE('',#65094,#10301);
#7805=LINE('',#65096,#10302);
#7806=LINE('',#65098,#10303);
#7807=LINE('',#65099,#10304);
#7808=LINE('',#65104,#10305);
#7809=LINE('',#65106,#10306);
#7810=LINE('',#65108,#10307);
#7811=LINE('',#65110,#10308);
#7812=LINE('',#65112,#10309);
#7813=LINE('',#65114,#10310);
#7814=LINE('',#65116,#10311);
#7815=LINE('',#65118,#10312);
#7816=LINE('',#65120,#10313);
#7817=LINE('',#65121,#10314);
#7818=LINE('',#65124,#10315);
#7819=LINE('',#65126,#10316);
#7820=LINE('',#65128,#10317);
#7821=LINE('',#65138,#10318);
#7822=LINE('',#65147,#10319);
#7823=LINE('',#65153,#10320);
#7824=LINE('',#65158,#10321);
#7825=LINE('',#65163,#10322);
#7826=LINE('',#65168,#10323);
#7827=LINE('',#65171,#10324);
#7828=LINE('',#65175,#10325);
#7829=LINE('',#65179,#10326);
#7830=LINE('',#65183,#10327);
#7831=LINE('',#65188,#10328);
#7832=LINE('',#65191,#10329);
#7833=LINE('',#65195,#10330);
#7834=LINE('',#65212,#10331);
#7835=LINE('',#65217,#10332);
#7836=LINE('',#65220,#10333);
#7837=LINE('',#65224,#10334);
#7838=LINE('',#65228,#10335);
#7839=LINE('',#65232,#10336);
#7840=LINE('',#65246,#10337);
#7841=LINE('',#65247,#10338);
#7842=LINE('',#65249,#10339);
#7843=LINE('',#65250,#10340);
#7844=LINE('',#65262,#10341);
#7845=LINE('',#65272,#10342);
#7846=LINE('',#65273,#10343);
#7847=LINE('',#65276,#10344);
#7848=LINE('',#65278,#10345);
#7849=LINE('',#65279,#10346);
#7850=LINE('',#65323,#10347);
#7851=LINE('',#65325,#10348);
#7852=LINE('',#65326,#10349);
#7853=LINE('',#65327,#10350);
#7854=LINE('',#65329,#10351);
#7855=LINE('',#65330,#10352);
#7856=LINE('',#65335,#10353);
#7857=LINE('',#65339,#10354);
#7858=LINE('',#65341,#10355);
#7859=LINE('',#65342,#10356);
#7860=LINE('',#65345,#10357);
#7861=LINE('',#65347,#10358);
#7862=LINE('',#65348,#10359);
#7863=LINE('',#65351,#10360);
#7864=LINE('',#65353,#10361);
#7865=LINE('',#65354,#10362);
#7866=LINE('',#65357,#10363);
#7867=LINE('',#65359,#10364);
#7868=LINE('',#65361,#10365);
#7869=LINE('',#65362,#10366);
#7870=LINE('',#65366,#10367);
#7871=LINE('',#65368,#10368);
#7872=LINE('',#65370,#10369);
#7873=LINE('',#65371,#10370);
#7874=LINE('',#65389,#10371);
#7875=LINE('',#65391,#10372);
#7876=LINE('',#65394,#10373);
#7877=LINE('',#65396,#10374);
#7878=LINE('',#65399,#10375);
#7879=LINE('',#65400,#10376);
#7880=LINE('',#65403,#10377);
#7881=LINE('',#65405,#10378);
#7882=LINE('',#65406,#10379);
#7883=LINE('',#65448,#10380);
#7884=LINE('',#65450,#10381);
#7885=LINE('',#65460,#10382);
#7886=LINE('',#65462,#10383);
#7887=LINE('',#65463,#10384);
#7888=LINE('',#65466,#10385);
#7889=LINE('',#65468,#10386);
#7890=LINE('',#65469,#10387);
#7891=LINE('',#65472,#10388);
#7892=LINE('',#65473,#10389);
#7893=LINE('',#65476,#10390);
#7894=LINE('',#65477,#10391);
#7895=LINE('',#65488,#10392);
#7896=LINE('',#65499,#10393);
#7897=LINE('',#65502,#10394);
#7898=LINE('',#65503,#10395);
#7899=LINE('',#65514,#10396);
#7900=LINE('',#65525,#10397);
#7901=LINE('',#65527,#10398);
#7902=LINE('',#65531,#10399);
#7903=LINE('',#65533,#10400);
#7904=LINE('',#65534,#10401);
#7905=LINE('',#65537,#10402);
#7906=LINE('',#65538,#10403);
#7907=LINE('',#65541,#10404);
#7908=LINE('',#65542,#10405);
#7909=LINE('',#65545,#10406);
#7910=LINE('',#65546,#10407);
#7911=LINE('',#65549,#10408);
#7912=LINE('',#65550,#10409);
#7913=LINE('',#65553,#10410);
#7914=LINE('',#65554,#10411);
#7915=LINE('',#65557,#10412);
#7916=LINE('',#65558,#10413);
#7917=LINE('',#65561,#10414);
#7918=LINE('',#65562,#10415);
#7919=LINE('',#65565,#10416);
#7920=LINE('',#65566,#10417);
#7921=LINE('',#65568,#10418);
#7922=LINE('',#65582,#10419);
#7923=LINE('',#65587,#10420);
#7924=LINE('',#65602,#10421);
#7925=LINE('',#65617,#10422);
#7926=LINE('',#65632,#10423);
#7927=LINE('',#65647,#10424);
#7928=LINE('',#65662,#10425);
#7929=LINE('',#65677,#10426);
#7930=LINE('',#65697,#10427);
#7931=LINE('',#65702,#10428);
#7932=LINE('',#65713,#10429);
#7933=LINE('',#65724,#10430);
#7934=LINE('',#65735,#10431);
#7935=LINE('',#65746,#10432);
#7936=LINE('',#65757,#10433);
#7937=LINE('',#65768,#10434);
#7938=LINE('',#65779,#10435);
#7939=LINE('',#65790,#10436);
#7940=LINE('',#65803,#10437);
#7941=LINE('',#65805,#10438);
#7942=LINE('',#65806,#10439);
#7943=LINE('',#65809,#10440);
#7944=LINE('',#65810,#10441);
#7945=LINE('',#65813,#10442);
#7946=LINE('',#65814,#10443);
#7947=LINE('',#65816,#10444);
#7948=LINE('',#65822,#10445);
#7949=LINE('',#65827,#10446);
#7950=LINE('',#65829,#10447);
#7951=LINE('',#65831,#10448);
#7952=LINE('',#65833,#10449);
#7953=LINE('',#65835,#10450);
#7954=LINE('',#65840,#10451);
#7955=LINE('',#65841,#10452);
#7956=LINE('',#65843,#10453);
#7957=LINE('',#65845,#10454);
#7958=LINE('',#65847,#10455);
#7959=LINE('',#65850,#10456);
#7960=LINE('',#65851,#10457);
#7961=LINE('',#65853,#10458);
#7962=LINE('',#65854,#10459);
#7963=LINE('',#65860,#10460);
#7964=LINE('',#65867,#10461);
#7965=LINE('',#65873,#10462);
#7966=LINE('',#65877,#10463);
#7967=LINE('',#65881,#10464);
#7968=LINE('',#65884,#10465);
#7969=LINE('',#65889,#10466);
#7970=LINE('',#65891,#10467);
#7971=LINE('',#65895,#10468);
#7972=LINE('',#65897,#10469);
#7973=LINE('',#65899,#10470);
#7974=LINE('',#65901,#10471);
#7975=LINE('',#65905,#10472);
#7976=LINE('',#65907,#10473);
#7977=LINE('',#65910,#10474);
#7978=LINE('',#65924,#10475);
#7979=LINE('',#65926,#10476);
#7980=LINE('',#65930,#10477);
#7981=LINE('',#65932,#10478);
#7982=LINE('',#65936,#10479);
#7983=LINE('',#65938,#10480);
#7984=LINE('',#65939,#10481);
#7985=LINE('',#65942,#10482);
#7986=LINE('',#65946,#10483);
#7987=LINE('',#65947,#10484);
#7988=LINE('',#65952,#10485);
#7989=LINE('',#65956,#10486);
#7990=LINE('',#65957,#10487);
#7991=LINE('',#65962,#10488);
#7992=LINE('',#65966,#10489);
#7993=LINE('',#65967,#10490);
#7994=LINE('',#65970,#10491);
#7995=LINE('',#65974,#10492);
#7996=LINE('',#65975,#10493);
#7997=LINE('',#65978,#10494);
#7998=LINE('',#65981,#10495);
#7999=LINE('',#65985,#10496);
#8000=LINE('',#65986,#10497);
#8001=LINE('',#65988,#10498);
#8002=LINE('',#65991,#10499);
#8003=LINE('',#65993,#10500);
#8004=LINE('',#65996,#10501);
#8005=LINE('',#65998,#10502);
#8006=LINE('',#66004,#10503);
#8007=LINE('',#66037,#10504);
#8008=LINE('',#66121,#10505);
#8009=LINE('',#66211,#10506);
#8010=LINE('',#66301,#10507);
#8011=LINE('',#66385,#10508);
#8012=LINE('',#66475,#10509);
#8013=LINE('',#66562,#10510);
#8014=LINE('',#66649,#10511);
#8015=LINE('',#66739,#10512);
#8016=LINE('',#66823,#10513);
#8017=LINE('',#66913,#10514);
#8018=LINE('',#67003,#10515);
#8019=LINE('',#67087,#10516);
#8020=LINE('',#67177,#10517);
#8021=LINE('',#67260,#10518);
#8022=LINE('',#67286,#10519);
#8023=LINE('',#67324,#10520);
#8024=LINE('',#67361,#10521);
#8025=LINE('',#67398,#10522);
#8026=LINE('',#67436,#10523);
#8027=LINE('',#67473,#10524);
#8028=LINE('',#67510,#10525);
#8029=LINE('',#67548,#10526);
#8030=LINE('',#67584,#10527);
#8031=LINE('',#67622,#10528);
#8032=LINE('',#67659,#10529);
#8033=LINE('',#67696,#10530);
#8034=LINE('',#67734,#10531);
#8035=LINE('',#67780,#10532);
#8036=LINE('',#67785,#10533);
#8037=LINE('',#67797,#10534);
#8038=LINE('',#67812,#10535);
#8039=LINE('',#67827,#10536);
#8040=LINE('',#67842,#10537);
#8041=LINE('',#67857,#10538);
#8042=LINE('',#67872,#10539);
#8043=LINE('',#67900,#10540);
#8044=LINE('',#67905,#10541);
#8045=LINE('',#67917,#10542);
#8046=LINE('',#67932,#10543);
#8047=LINE('',#67947,#10544);
#8048=LINE('',#67962,#10545);
#8049=LINE('',#67977,#10546);
#8050=LINE('',#67992,#10547);
#8051=LINE('',#68007,#10548);
#8052=LINE('',#68035,#10549);
#8053=LINE('',#68040,#10550);
#8054=LINE('',#68052,#10551);
#8055=LINE('',#68067,#10552);
#8056=LINE('',#68082,#10553);
#8057=LINE('',#68097,#10554);
#8058=LINE('',#68112,#10555);
#8059=LINE('',#68127,#10556);
#8060=LINE('',#68142,#10557);
#8061=LINE('',#68157,#10558);
#8062=LINE('',#68172,#10559);
#8063=LINE('',#68187,#10560);
#8064=LINE('',#68202,#10561);
#8065=LINE('',#68217,#10562);
#8066=LINE('',#68232,#10563);
#8067=LINE('',#68247,#10564);
#8068=LINE('',#68267,#10565);
#8069=LINE('',#68269,#10566);
#8070=LINE('',#68271,#10567);
#8071=LINE('',#68272,#10568);
#8072=LINE('',#68275,#10569);
#8073=LINE('',#68277,#10570);
#8074=LINE('',#68278,#10571);
#8075=LINE('',#68281,#10572);
#8076=LINE('',#68283,#10573);
#8077=LINE('',#68284,#10574);
#8078=LINE('',#68286,#10575);
#8079=LINE('',#68287,#10576);
#8080=LINE('',#68301,#10577);
#8081=LINE('',#68306,#10578);
#8082=LINE('',#68318,#10579);
#8083=LINE('',#68333,#10580);
#8084=LINE('',#68348,#10581);
#8085=LINE('',#68363,#10582);
#8086=LINE('',#68378,#10583);
#8087=LINE('',#68393,#10584);
#8088=LINE('',#68421,#10585);
#8089=LINE('',#68426,#10586);
#8090=LINE('',#68438,#10587);
#8091=LINE('',#68453,#10588);
#8092=LINE('',#68468,#10589);
#8093=LINE('',#68483,#10590);
#8094=LINE('',#68498,#10591);
#8095=LINE('',#68513,#10592);
#8096=LINE('',#68528,#10593);
#8097=LINE('',#68556,#10594);
#8098=LINE('',#68561,#10595);
#8099=LINE('',#68573,#10596);
#8100=LINE('',#68588,#10597);
#8101=LINE('',#68603,#10598);
#8102=LINE('',#68618,#10599);
#8103=LINE('',#68633,#10600);
#8104=LINE('',#68648,#10601);
#8105=LINE('',#68663,#10602);
#8106=LINE('',#68678,#10603);
#8107=LINE('',#68693,#10604);
#8108=LINE('',#68708,#10605);
#8109=LINE('',#68723,#10606);
#8110=LINE('',#68738,#10607);
#8111=LINE('',#68753,#10608);
#8112=LINE('',#68768,#10609);
#8113=LINE('',#70640,#10610);
#8114=LINE('',#70642,#10611);
#8115=LINE('',#70644,#10612);
#8116=LINE('',#70646,#10613);
#8117=LINE('',#70648,#10614);
#8118=LINE('',#70649,#10615);
#8119=LINE('',#70674,#10616);
#8120=LINE('',#70684,#10617);
#8121=LINE('',#70685,#10618);
#8122=LINE('',#70687,#10619);
#8123=LINE('',#70689,#10620);
#8124=LINE('',#70691,#10621);
#8125=LINE('',#70693,#10622);
#8126=LINE('',#70700,#10623);
#8127=VECTOR('',#28995,6.175);
#8128=VECTOR('',#29002,1.);
#8129=VECTOR('',#29005,1.);
#8130=VECTOR('',#29008,1.);
#8131=VECTOR('',#29011,1.);
#8132=VECTOR('',#29014,1.);
#8133=VECTOR('',#29017,1.);
#8134=VECTOR('',#29020,1.);
#8135=VECTOR('',#29023,1.);
#8136=VECTOR('',#29026,1.);
#8137=VECTOR('',#29029,1.);
#8138=VECTOR('',#29032,1.);
#8139=VECTOR('',#29035,1.);
#8140=VECTOR('',#29038,1.);
#8141=VECTOR('',#29041,1.);
#8142=VECTOR('',#29044,1.);
#8143=VECTOR('',#29047,1.);
#8144=VECTOR('',#29050,1.);
#8145=VECTOR('',#29053,1.);
#8146=VECTOR('',#29056,1.);
#8147=VECTOR('',#29059,1.);
#8148=VECTOR('',#29062,1.);
#8149=VECTOR('',#29065,1.);
#8150=VECTOR('',#29068,1.);
#8151=VECTOR('',#29071,1.);
#8152=VECTOR('',#29074,1.);
#8153=VECTOR('',#29077,1.);
#8154=VECTOR('',#29080,1.);
#8155=VECTOR('',#29083,1.);
#8156=VECTOR('',#29086,1.);
#8157=VECTOR('',#29089,1.);
#8158=VECTOR('',#29092,1.);
#8159=VECTOR('',#29095,1.);
#8160=VECTOR('',#29098,1.);
#8161=VECTOR('',#29101,1.);
#8162=VECTOR('',#29104,1.);
#8163=VECTOR('',#29107,1.);
#8164=VECTOR('',#29112,6.25);
#8165=VECTOR('',#29117,6.175);
#8166=VECTOR('',#29124,1.);
#8167=VECTOR('',#29127,1.);
#8168=VECTOR('',#29130,1.);
#8169=VECTOR('',#29133,1.);
#8170=VECTOR('',#29136,1.);
#8171=VECTOR('',#29139,1.);
#8172=VECTOR('',#29142,1.);
#8173=VECTOR('',#29145,1.);
#8174=VECTOR('',#29148,1.);
#8175=VECTOR('',#29151,1.);
#8176=VECTOR('',#29154,1.);
#8177=VECTOR('',#29157,1.);
#8178=VECTOR('',#29160,1.);
#8179=VECTOR('',#29163,1.);
#8180=VECTOR('',#29166,1.);
#8181=VECTOR('',#29169,1.);
#8182=VECTOR('',#29172,1.);
#8183=VECTOR('',#29175,1.);
#8184=VECTOR('',#29178,1.);
#8185=VECTOR('',#29181,1.);
#8186=VECTOR('',#29184,1.);
#8187=VECTOR('',#29187,1.);
#8188=VECTOR('',#29190,1.);
#8189=VECTOR('',#29193,1.);
#8190=VECTOR('',#29196,1.);
#8191=VECTOR('',#29199,1.);
#8192=VECTOR('',#29202,1.);
#8193=VECTOR('',#29205,1.);
#8194=VECTOR('',#29208,1.);
#8195=VECTOR('',#29211,1.);
#8196=VECTOR('',#29214,1.);
#8197=VECTOR('',#29217,1.);
#8198=VECTOR('',#29220,1.);
#8199=VECTOR('',#29223,1.);
#8200=VECTOR('',#29226,1.);
#8201=VECTOR('',#29229,1.);
#8202=VECTOR('',#29234,6.25);
#8203=VECTOR('',#29245,2.95);
#8204=VECTOR('',#29250,3.);
#8205=VECTOR('',#29257,6.175);
#8206=VECTOR('',#29262,6.175);
#8207=VECTOR('',#29271,3.);
#8208=VECTOR('',#29276,2.95);
#8209=VECTOR('',#29279,1.);
#8210=VECTOR('',#29282,1.);
#8211=VECTOR('',#29283,1.);
#8212=VECTOR('',#29286,1.);
#8213=VECTOR('',#29289,1.);
#8214=VECTOR('',#29292,1.);
#8215=VECTOR('',#29293,1.);
#8216=VECTOR('',#29296,1.);
#8217=VECTOR('',#29299,1.);
#8218=VECTOR('',#29302,1.);
#8219=VECTOR('',#29303,1.);
#8220=VECTOR('',#29306,1.);
#8221=VECTOR('',#29309,1.);
#8222=VECTOR('',#29312,1.);
#8223=VECTOR('',#29313,1.);
#8224=VECTOR('',#29316,1.);
#8225=VECTOR('',#29319,1.);
#8226=VECTOR('',#29322,1.);
#8227=VECTOR('',#29323,1.);
#8228=VECTOR('',#29326,1.);
#8229=VECTOR('',#29329,1.);
#8230=VECTOR('',#29332,1.);
#8231=VECTOR('',#29333,1.);
#8232=VECTOR('',#29336,1.);
#8233=VECTOR('',#29339,1.);
#8234=VECTOR('',#29342,1.);
#8235=VECTOR('',#29343,1.);
#8236=VECTOR('',#29346,1.);
#8237=VECTOR('',#29349,1.);
#8238=VECTOR('',#29352,1.);
#8239=VECTOR('',#29353,1.);
#8240=VECTOR('',#29356,1.);
#8241=VECTOR('',#29359,1.);
#8242=VECTOR('',#29362,1.);
#8243=VECTOR('',#29363,1.);
#8244=VECTOR('',#29366,1.);
#8245=VECTOR('',#29369,1.);
#8246=VECTOR('',#29372,1.);
#8247=VECTOR('',#29373,1.);
#8248=VECTOR('',#29376,1.);
#8249=VECTOR('',#29379,1.);
#8250=VECTOR('',#29382,1.);
#8251=VECTOR('',#29383,1.);
#8252=VECTOR('',#29386,1.);
#8253=VECTOR('',#29389,1.);
#8254=VECTOR('',#29392,1.);
#8255=VECTOR('',#29393,1.);
#8256=VECTOR('',#29396,1.);
#8257=VECTOR('',#29399,1.);
#8258=VECTOR('',#29402,1.);
#8259=VECTOR('',#29403,1.);
#8260=VECTOR('',#29406,1.);
#8261=VECTOR('',#29409,1.);
#8262=VECTOR('',#29412,1.);
#8263=VECTOR('',#29413,1.);
#8264=VECTOR('',#29416,1.);
#8265=VECTOR('',#29419,1.);
#8266=VECTOR('',#29422,1.);
#8267=VECTOR('',#29423,1.);
#8268=VECTOR('',#29426,1.);
#8269=VECTOR('',#29429,1.);
#8270=VECTOR('',#29432,1.);
#8271=VECTOR('',#29433,1.);
#8272=VECTOR('',#29436,1.);
#8273=VECTOR('',#29439,1.);
#8274=VECTOR('',#29442,1.);
#8275=VECTOR('',#29443,1.);
#8276=VECTOR('',#29446,1.);
#8277=VECTOR('',#29449,1.);
#8278=VECTOR('',#29452,1.);
#8279=VECTOR('',#29453,1.);
#8280=VECTOR('',#29456,1.);
#8281=VECTOR('',#29499,1.2);
#8282=VECTOR('',#29504,1.2);
#8283=VECTOR('',#29507,1.2);
#8284=VECTOR('',#29510,1.2);
#8285=VECTOR('',#29513,1.2);
#8286=VECTOR('',#29516,1.2);
#8287=VECTOR('',#29519,1.2);
#8288=VECTOR('',#29522,1.2);
#8289=VECTOR('',#29525,1.2);
#8290=VECTOR('',#29528,1.2);
#8291=VECTOR('',#29531,1.2);
#8292=VECTOR('',#29534,1.2);
#8293=VECTOR('',#29537,1.2);
#8294=VECTOR('',#29540,1.016475);
#8295=VECTOR('',#29545,1.016475);
#8296=VECTOR('',#29550,1.016475);
#8297=VECTOR('',#29553,1.016475);
#8298=VECTOR('',#29556,1.016475);
#8299=VECTOR('',#29559,1.016475);
#8300=VECTOR('',#29562,1.016475);
#8301=VECTOR('',#29565,1.016475);
#8302=VECTOR('',#29568,1.016475);
#8303=VECTOR('',#29571,1.016475);
#8304=VECTOR('',#29574,1.016475);
#8305=VECTOR('',#29577,1.016475);
#8306=VECTOR('',#29580,1.016475);
#8307=VECTOR('',#29609,1.85);
#8308=VECTOR('',#29614,2.);
#8309=VECTOR('',#29621,1.225);
#8310=VECTOR('',#29626,1.125);
#8311=VECTOR('',#29633,1.);
#8312=VECTOR('',#29634,1.);
#8313=VECTOR('',#29635,1.);
#8314=VECTOR('',#29636,1.);
#8315=VECTOR('',#29641,1.);
#8316=VECTOR('',#29650,1.);
#8317=VECTOR('',#29651,1.);
#8318=VECTOR('',#29652,1.);
#8319=VECTOR('',#29655,1.);
#8320=VECTOR('',#29656,1.);
#8321=VECTOR('',#29657,1.);
#8322=VECTOR('',#29658,1.);
#8323=VECTOR('',#29661,1.);
#8324=VECTOR('',#29662,1.);
#8325=VECTOR('',#29663,1.);
#8326=VECTOR('',#29666,1.);
#8327=VECTOR('',#29667,1.);
#8328=VECTOR('',#29670,1.);
#8329=VECTOR('',#29671,1.);
#8330=VECTOR('',#29674,1.);
#8331=VECTOR('',#29681,1.);
#8332=VECTOR('',#29682,1.);
#8333=VECTOR('',#29687,1.);
#8334=VECTOR('',#29690,1.);
#8335=VECTOR('',#29693,1.);
#8336=VECTOR('',#29696,1.);
#8337=VECTOR('',#29699,1.);
#8338=VECTOR('',#29702,1.);
#8339=VECTOR('',#29711,1.);
#8340=VECTOR('',#29712,1.);
#8341=VECTOR('',#29713,1.);
#8342=VECTOR('',#29714,1.);
#8343=VECTOR('',#29717,1.);
#8344=VECTOR('',#29718,1.);
#8345=VECTOR('',#29719,1.);
#8346=VECTOR('',#29722,1.);
#8347=VECTOR('',#29723,1.);
#8348=VECTOR('',#29726,1.);
#8349=VECTOR('',#29729,1.);
#8350=VECTOR('',#29730,1.);
#8351=VECTOR('',#29731,1.);
#8352=VECTOR('',#29734,1.);
#8353=VECTOR('',#29735,1.);
#8354=VECTOR('',#29746,1.);
#8355=VECTOR('',#29751,1.);
#8356=VECTOR('',#29754,2.08);
#8357=VECTOR('',#29761,2.005);
#8358=VECTOR('',#29764,1.);
#8359=VECTOR('',#29765,1.);
#8360=VECTOR('',#29766,1.);
#8361=VECTOR('',#29767,1.);
#8362=VECTOR('',#29770,1.);
#8363=VECTOR('',#29771,1.);
#8364=VECTOR('',#29772,1.);
#8365=VECTOR('',#29775,1.);
#8366=VECTOR('',#29776,1.);
#8367=VECTOR('',#29779,1.);
#8368=VECTOR('',#29782,1.);
#8369=VECTOR('',#29783,1.);
#8370=VECTOR('',#29784,1.);
#8371=VECTOR('',#29785,1.);
#8372=VECTOR('',#29790,1.);
#8373=VECTOR('',#29797,1.);
#8374=VECTOR('',#29798,1.);
#8375=VECTOR('',#29805,1.);
#8376=VECTOR('',#29810,1.);
#8377=VECTOR('',#29813,1.);
#8378=VECTOR('',#29814,1.);
#8379=VECTOR('',#29815,1.);
#8380=VECTOR('',#29818,1.);
#8381=VECTOR('',#29819,1.);
#8382=VECTOR('',#29820,1.);
#8383=VECTOR('',#29823,1.);
#8384=VECTOR('',#29824,1.);
#8385=VECTOR('',#29827,1.);
#8386=VECTOR('',#29830,1.);
#8387=VECTOR('',#29831,1.);
#8388=VECTOR('',#29832,1.);
#8389=VECTOR('',#29833,1.);
#8390=VECTOR('',#29840,1.);
#8391=VECTOR('',#29841,1.);
#8392=VECTOR('',#29848,1.);
#8393=VECTOR('',#29853,1.);
#8394=VECTOR('',#29878,1.);
#8395=VECTOR('',#29883,1.);
#8396=VECTOR('',#29886,1.);
#8397=VECTOR('',#29891,1.);
#8398=VECTOR('',#29900,1.);
#8399=VECTOR('',#29905,1.);
#8400=VECTOR('',#29916,2.055);
#8401=VECTOR('',#29919,1.);
#8402=VECTOR('',#29942,1.925);
#8403=VECTOR('',#29947,2.);
#8404=VECTOR('',#29952,1.925);
#8405=VECTOR('',#29957,1.);
#8406=VECTOR('',#29960,0.805);
#8407=VECTOR('',#29965,7.5);
#8408=VECTOR('',#29966,7.5);
#8409=VECTOR('',#29969,1.);
#8410=VECTOR('',#29974,3.0025);
#8411=VECTOR('',#29997,1.49999999999999);
#8412=VECTOR('',#30000,1.5);
#8413=VECTOR('',#30003,1.5);
#8414=VECTOR('',#30006,1.5);
#8415=VECTOR('',#30009,1.5);
#8416=VECTOR('',#30012,1.5);
#8417=VECTOR('',#30015,3.0525);
#8418=VECTOR('',#30024,7.4);
#8419=VECTOR('',#30029,7.4);
#8420=VECTOR('',#30036,3.0525);
#8421=VECTOR('',#30041,1.);
#8422=VECTOR('',#30046,1.);
#8423=VECTOR('',#30049,1.);
#8424=VECTOR('',#30052,1.);
#8425=VECTOR('',#30055,1.);
#8426=VECTOR('',#30058,1.);
#8427=VECTOR('',#30061,1.);
#8428=VECTOR('',#30064,0.8469);
#8429=VECTOR('',#30069,0.8469);
#8430=VECTOR('',#30074,0.8469);
#8431=VECTOR('',#30077,0.8469);
#8432=VECTOR('',#30080,0.8469);
#8433=VECTOR('',#30083,0.8469);
#8434=VECTOR('',#30086,0.8469);
#8435=VECTOR('',#30105,1.);
#8436=VECTOR('',#30110,1.);
#8437=VECTOR('',#30115,1.);
#8438=VECTOR('',#30120,1.);
#8439=VECTOR('',#30125,1.);
#8440=VECTOR('',#30130,1.);
#8441=VECTOR('',#30135,0.288675134594813);
#8442=VECTOR('',#30152,1.);
#8443=VECTOR('',#30153,1.);
#8444=VECTOR('',#30154,1.);
#8445=VECTOR('',#30157,1.);
#8446=VECTOR('',#30158,1.);
#8447=VECTOR('',#30161,1.);
#8448=VECTOR('',#30162,1.);
#8449=VECTOR('',#30165,1.);
#8450=VECTOR('',#30166,1.);
#8451=VECTOR('',#30169,1.);
#8452=VECTOR('',#30170,1.);
#8453=VECTOR('',#30173,1.);
#8454=VECTOR('',#30174,1.);
#8455=VECTOR('',#30177,1.);
#8456=VECTOR('',#30178,1.);
#8457=VECTOR('',#30181,1.);
#8458=VECTOR('',#30182,1.);
#8459=VECTOR('',#30185,1.);
#8460=VECTOR('',#30186,1.);
#8461=VECTOR('',#30189,1.);
#8462=VECTOR('',#30192,1.);
#8463=VECTOR('',#30197,1.);
#8464=VECTOR('',#30200,1.);
#8465=VECTOR('',#30201,1.);
#8466=VECTOR('',#30204,1.);
#8467=VECTOR('',#30207,1.);
#8468=VECTOR('',#30210,1.);
#8469=VECTOR('',#30211,1.);
#8470=VECTOR('',#30214,1.);
#8471=VECTOR('',#30221,1.);
#8472=VECTOR('',#30234,0.875);
#8473=VECTOR('',#30243,0.96);
#8474=VECTOR('',#30250,1.);
#8475=VECTOR('',#30251,1.);
#8476=VECTOR('',#30252,1.);
#8477=VECTOR('',#30253,1.);
#8478=VECTOR('',#30256,1.);
#8479=VECTOR('',#30257,1.);
#8480=VECTOR('',#30258,1.);
#8481=VECTOR('',#30261,1.);
#8482=VECTOR('',#30262,1.);
#8483=VECTOR('',#30263,1.);
#8484=VECTOR('',#30266,1.);
#8485=VECTOR('',#30267,1.);
#8486=VECTOR('',#30272,1.);
#8487=VECTOR('',#30273,1.);
#8488=VECTOR('',#30274,1.);
#8489=VECTOR('',#30275,1.);
#8490=VECTOR('',#30278,1.);
#8491=VECTOR('',#30279,1.);
#8492=VECTOR('',#30280,1.);
#8493=VECTOR('',#30283,1.);
#8494=VECTOR('',#30284,1.);
#8495=VECTOR('',#30285,1.);
#8496=VECTOR('',#30288,1.);
#8497=VECTOR('',#30289,1.);
#8498=VECTOR('',#30294,1.);
#8499=VECTOR('',#30295,1.);
#8500=VECTOR('',#30296,1.);
#8501=VECTOR('',#30299,1.);
#8502=VECTOR('',#30300,1.);
#8503=VECTOR('',#30301,1.);
#8504=VECTOR('',#30304,1.);
#8505=VECTOR('',#30305,1.);
#8506=VECTOR('',#30306,1.);
#8507=VECTOR('',#30309,1.);
#8508=VECTOR('',#30310,1.);
#8509=VECTOR('',#30311,1.);
#8510=VECTOR('',#30314,1.);
#8511=VECTOR('',#30315,1.);
#8512=VECTOR('',#30316,1.);
#8513=VECTOR('',#30319,1.);
#8514=VECTOR('',#30320,1.);
#8515=VECTOR('',#30323,1.);
#8516=VECTOR('',#30324,1.);
#8517=VECTOR('',#30325,1.);
#8518=VECTOR('',#30328,1.);
#8519=VECTOR('',#30329,1.);
#8520=VECTOR('',#30330,1.);
#8521=VECTOR('',#30333,1.);
#8522=VECTOR('',#30334,1.);
#8523=VECTOR('',#30337,1.);
#8524=VECTOR('',#30338,1.);
#8525=VECTOR('',#30341,1.);
#8526=VECTOR('',#30342,1.);
#8527=VECTOR('',#30343,1.);
#8528=VECTOR('',#30346,1.);
#8529=VECTOR('',#30347,1.);
#8530=VECTOR('',#30350,1.);
#8531=VECTOR('',#30351,1.);
#8532=VECTOR('',#30354,1.);
#8533=VECTOR('',#30355,1.);
#8534=VECTOR('',#30358,1.);
#8535=VECTOR('',#30359,1.);
#8536=VECTOR('',#30362,1.);
#8537=VECTOR('',#30363,1.);
#8538=VECTOR('',#30366,1.);
#8539=VECTOR('',#30367,1.);
#8540=VECTOR('',#30370,1.);
#8541=VECTOR('',#30371,1.);
#8542=VECTOR('',#30374,1.);
#8543=VECTOR('',#30375,1.);
#8544=VECTOR('',#30378,1.);
#8545=VECTOR('',#30379,1.);
#8546=VECTOR('',#30396,0.8);
#8547=VECTOR('',#30401,0.8);
#8548=VECTOR('',#30404,0.8);
#8549=VECTOR('',#30407,0.8);
#8550=VECTOR('',#30410,0.8);
#8551=VECTOR('',#30413,0.8);
#8552=VECTOR('',#30416,0.8);
#8553=VECTOR('',#30419,0.8);
#8554=VECTOR('',#30422,0.8);
#8555=VECTOR('',#30425,0.8);
#8556=VECTOR('',#30428,0.8);
#8557=VECTOR('',#30431,0.8);
#8558=VECTOR('',#30434,0.8);
#8559=VECTOR('',#30437,0.8);
#8560=VECTOR('',#30440,0.8);
#8561=VECTOR('',#30443,0.8);
#8562=VECTOR('',#30446,0.8);
#8563=VECTOR('',#30449,0.8);
#8564=VECTOR('',#30452,0.8);
#8565=VECTOR('',#30455,0.8);
#8566=VECTOR('',#30458,0.8);
#8567=VECTOR('',#30461,0.8);
#8568=VECTOR('',#30464,0.8);
#8569=VECTOR('',#30467,0.8);
#8570=VECTOR('',#30470,0.8);
#8571=VECTOR('',#30473,0.8);
#8572=VECTOR('',#30476,0.8);
#8573=VECTOR('',#30479,0.8);
#8574=VECTOR('',#30482,0.8);
#8575=VECTOR('',#30485,0.6767);
#8576=VECTOR('',#30490,0.6767);
#8577=VECTOR('',#30495,0.6767);
#8578=VECTOR('',#30498,0.6767);
#8579=VECTOR('',#30501,0.6767);
#8580=VECTOR('',#30504,0.6767);
#8581=VECTOR('',#30507,0.6767);
#8582=VECTOR('',#30510,0.6767);
#8583=VECTOR('',#30513,0.6767);
#8584=VECTOR('',#30516,0.6767);
#8585=VECTOR('',#30519,0.6767);
#8586=VECTOR('',#30522,0.6767);
#8587=VECTOR('',#30525,0.6767);
#8588=VECTOR('',#30528,0.6767);
#8589=VECTOR('',#30531,0.6767);
#8590=VECTOR('',#30534,0.6767);
#8591=VECTOR('',#30537,0.6767);
#8592=VECTOR('',#30540,0.6767);
#8593=VECTOR('',#30543,0.6767);
#8594=VECTOR('',#30546,0.6767);
#8595=VECTOR('',#30549,0.6767);
#8596=VECTOR('',#30552,0.6767);
#8597=VECTOR('',#30555,0.6767);
#8598=VECTOR('',#30558,0.6767);
#8599=VECTOR('',#30561,0.6767);
#8600=VECTOR('',#30564,0.6767);
#8601=VECTOR('',#30567,0.6767);
#8602=VECTOR('',#30570,0.6767);
#8603=VECTOR('',#30573,0.6767);
#8604=VECTOR('',#30592,1.);
#8605=VECTOR('',#30597,1.);
#8606=VECTOR('',#30602,1.);
#8607=VECTOR('',#30607,1.);
#8608=VECTOR('',#30612,1.);
#8609=VECTOR('',#30617,1.);
#8610=VECTOR('',#30622,0.23094010767585);
#8611=VECTOR('',#30639,1.);
#8612=VECTOR('',#30640,1.);
#8613=VECTOR('',#30641,1.);
#8614=VECTOR('',#30644,1.);
#8615=VECTOR('',#30645,1.);
#8616=VECTOR('',#30648,1.);
#8617=VECTOR('',#30649,1.);
#8618=VECTOR('',#30652,1.);
#8619=VECTOR('',#30653,1.);
#8620=VECTOR('',#30656,1.);
#8621=VECTOR('',#30657,1.);
#8622=VECTOR('',#30660,1.);
#8623=VECTOR('',#30661,1.);
#8624=VECTOR('',#30664,1.);
#8625=VECTOR('',#30665,1.);
#8626=VECTOR('',#30668,1.);
#8627=VECTOR('',#30669,1.);
#8628=VECTOR('',#30672,1.);
#8629=VECTOR('',#30673,1.);
#8630=VECTOR('',#30676,1.);
#8631=VECTOR('',#30679,1.);
#8632=VECTOR('',#30684,1.);
#8633=VECTOR('',#30687,1.);
#8634=VECTOR('',#30688,1.);
#8635=VECTOR('',#30691,1.);
#8636=VECTOR('',#30694,1.);
#8637=VECTOR('',#30697,1.);
#8638=VECTOR('',#30698,1.);
#8639=VECTOR('',#30701,1.);
#8640=VECTOR('',#30708,1.);
#8641=VECTOR('',#30721,0.7);
#8642=VECTOR('',#30730,0.76);
#8643=VECTOR('',#30739,0.845);
#8644=VECTOR('',#30746,0.805);
#8645=VECTOR('',#30755,0.845);
#8646=VECTOR('',#30762,1.28782032302755);
#8647=VECTOR('',#30765,1.);
#8648=VECTOR('',#30766,1.);
#8649=VECTOR('',#30769,1.);
#8650=VECTOR('',#30772,1.);
#8651=VECTOR('',#30775,1.28782032302755);
#8652=VECTOR('',#30778,1.);
#8653=VECTOR('',#30781,1.);
#8654=VECTOR('',#30788,0.8);
#8655=VECTOR('',#30793,0.8);
#8656=VECTOR('',#30796,0.8);
#8657=VECTOR('',#30799,0.8);
#8658=VECTOR('',#30802,0.8);
#8659=VECTOR('',#30805,0.8);
#8660=VECTOR('',#30808,0.8);
#8661=VECTOR('',#30811,0.8);
#8662=VECTOR('',#30814,0.8);
#8663=VECTOR('',#30817,0.8);
#8664=VECTOR('',#30820,0.8);
#8665=VECTOR('',#30823,0.8);
#8666=VECTOR('',#30826,0.8);
#8667=VECTOR('',#30829,0.8);
#8668=VECTOR('',#30832,0.8);
#8669=VECTOR('',#30835,0.8);
#8670=VECTOR('',#30838,0.8);
#8671=VECTOR('',#30841,0.8);
#8672=VECTOR('',#30844,0.8);
#8673=VECTOR('',#30847,0.6767);
#8674=VECTOR('',#30852,0.6767);
#8675=VECTOR('',#30857,0.6767);
#8676=VECTOR('',#30860,0.6767);
#8677=VECTOR('',#30863,0.6767);
#8678=VECTOR('',#30866,0.6767);
#8679=VECTOR('',#30869,0.6767);
#8680=VECTOR('',#30872,0.6767);
#8681=VECTOR('',#30875,0.6767);
#8682=VECTOR('',#30878,0.6767);
#8683=VECTOR('',#30881,0.6767);
#8684=VECTOR('',#30884,0.6767);
#8685=VECTOR('',#30887,0.6767);
#8686=VECTOR('',#30890,0.6767);
#8687=VECTOR('',#30893,0.6767);
#8688=VECTOR('',#30896,0.6767);
#8689=VECTOR('',#30899,0.6767);
#8690=VECTOR('',#30902,0.6767);
#8691=VECTOR('',#30905,0.6767);
#8692=VECTOR('',#30924,1.);
#8693=VECTOR('',#30929,1.);
#8694=VECTOR('',#30934,1.);
#8695=VECTOR('',#30939,1.);
#8696=VECTOR('',#30944,1.);
#8697=VECTOR('',#30949,1.);
#8698=VECTOR('',#30954,0.23094010767585);
#8699=VECTOR('',#30971,1.);
#8700=VECTOR('',#30972,1.);
#8701=VECTOR('',#30973,1.);
#8702=VECTOR('',#30976,1.);
#8703=VECTOR('',#30977,1.);
#8704=VECTOR('',#30980,1.);
#8705=VECTOR('',#30981,1.);
#8706=VECTOR('',#30984,1.);
#8707=VECTOR('',#30985,1.);
#8708=VECTOR('',#30988,1.);
#8709=VECTOR('',#30989,1.);
#8710=VECTOR('',#30992,1.);
#8711=VECTOR('',#30993,1.);
#8712=VECTOR('',#30996,1.);
#8713=VECTOR('',#30997,1.);
#8714=VECTOR('',#31000,1.);
#8715=VECTOR('',#31001,1.);
#8716=VECTOR('',#31004,1.);
#8717=VECTOR('',#31005,1.);
#8718=VECTOR('',#31008,1.);
#8719=VECTOR('',#31011,1.);
#8720=VECTOR('',#31016,1.);
#8721=VECTOR('',#31019,1.);
#8722=VECTOR('',#31020,1.);
#8723=VECTOR('',#31023,1.);
#8724=VECTOR('',#31026,1.);
#8725=VECTOR('',#31029,1.);
#8726=VECTOR('',#31030,1.);
#8727=VECTOR('',#31033,1.);
#8728=VECTOR('',#31040,1.);
#8729=VECTOR('',#31053,0.7);
#8730=VECTOR('',#31062,0.76);
#8731=VECTOR('',#31067,1.);
#8732=VECTOR('',#31072,7.5);
#8733=VECTOR('',#31077,2.01);
#8734=VECTOR('',#31078,1.);
#8735=VECTOR('',#31079,1.);
#8736=VECTOR('',#31080,1.);
#8737=VECTOR('',#31085,1.08);
#8738=VECTOR('',#31094,1.005);
#8739=VECTOR('',#31101,1.);
#8740=VECTOR('',#31104,0.805000000000009);
#8741=VECTOR('',#31109,3.0025);
#8742=VECTOR('',#31112,1.);
#8743=VECTOR('',#31121,3.0525);
#8744=VECTOR('',#31130,7.4);
#8745=VECTOR('',#31133,7.4);
#8746=VECTOR('',#31138,1.);
#8747=VECTOR('',#31139,1.);
#8748=VECTOR('',#31140,1.);
#8749=VECTOR('',#31141,1.);
#8750=VECTOR('',#31142,1.);
#8751=VECTOR('',#31143,1.);
#8752=VECTOR('',#31146,1.);
#8753=VECTOR('',#31147,1.);
#8754=VECTOR('',#31148,1.);
#8755=VECTOR('',#31149,1.);
#8756=VECTOR('',#31152,1.);
#8757=VECTOR('',#31153,1.);
#8758=VECTOR('',#31156,1.);
#8759=VECTOR('',#31157,1.);
#8760=VECTOR('',#31158,1.);
#8761=VECTOR('',#31161,1.);
#8762=VECTOR('',#31162,1.);
#8763=VECTOR('',#31163,1.);
#8764=VECTOR('',#31164,1.);
#8765=VECTOR('',#31165,1.);
#8766=VECTOR('',#31166,1.);
#8767=VECTOR('',#31169,1.);
#8768=VECTOR('',#31170,1.);
#8769=VECTOR('',#31171,1.);
#8770=VECTOR('',#31172,1.);
#8771=VECTOR('',#31175,1.);
#8772=VECTOR('',#31176,1.);
#8773=VECTOR('',#31179,1.);
#8774=VECTOR('',#31180,1.);
#8775=VECTOR('',#31181,1.);
#8776=VECTOR('',#31184,1.);
#8777=VECTOR('',#31185,1.);
#8778=VECTOR('',#31186,1.);
#8779=VECTOR('',#31187,1.);
#8780=VECTOR('',#31188,1.);
#8781=VECTOR('',#31189,1.);
#8782=VECTOR('',#31192,1.);
#8783=VECTOR('',#31193,1.);
#8784=VECTOR('',#31194,1.);
#8785=VECTOR('',#31197,1.);
#8786=VECTOR('',#31198,1.);
#8787=VECTOR('',#31199,1.);
#8788=VECTOR('',#31202,1.);
#8789=VECTOR('',#31203,1.);
#8790=VECTOR('',#31204,1.);
#8791=VECTOR('',#31205,1.);
#8792=VECTOR('',#31208,1.);
#8793=VECTOR('',#31209,1.);
#8794=VECTOR('',#31210,1.);
#8795=VECTOR('',#31211,1.);
#8796=VECTOR('',#31212,1.);
#8797=VECTOR('',#31213,1.);
#8798=VECTOR('',#31216,1.);
#8799=VECTOR('',#31217,1.);
#8800=VECTOR('',#31218,1.);
#8801=VECTOR('',#31219,1.);
#8802=VECTOR('',#31222,1.);
#8803=VECTOR('',#31223,1.);
#8804=VECTOR('',#31226,1.);
#8805=VECTOR('',#31227,1.);
#8806=VECTOR('',#31228,1.);
#8807=VECTOR('',#31231,1.);
#8808=VECTOR('',#31232,1.);
#8809=VECTOR('',#31233,1.);
#8810=VECTOR('',#31234,1.);
#8811=VECTOR('',#31235,1.);
#8812=VECTOR('',#31236,1.);
#8813=VECTOR('',#31239,1.);
#8814=VECTOR('',#31240,1.);
#8815=VECTOR('',#31241,1.);
#8816=VECTOR('',#31244,1.);
#8817=VECTOR('',#31245,1.);
#8818=VECTOR('',#31246,1.);
#8819=VECTOR('',#31247,1.);
#8820=VECTOR('',#31250,1.);
#8821=VECTOR('',#31251,1.);
#8822=VECTOR('',#31252,1.);
#8823=VECTOR('',#31255,1.);
#8824=VECTOR('',#31256,1.);
#8825=VECTOR('',#31257,1.);
#8826=VECTOR('',#31258,1.);
#8827=VECTOR('',#31259,1.);
#8828=VECTOR('',#31260,1.);
#8829=VECTOR('',#31263,1.);
#8830=VECTOR('',#31264,1.);
#8831=VECTOR('',#31265,1.);
#8832=VECTOR('',#31266,1.);
#8833=VECTOR('',#31269,1.);
#8834=VECTOR('',#31270,1.);
#8835=VECTOR('',#31271,1.);
#8836=VECTOR('',#31272,1.);
#8837=VECTOR('',#31275,1.);
#8838=VECTOR('',#31276,1.);
#8839=VECTOR('',#31279,1.);
#8840=VECTOR('',#31280,1.);
#8841=VECTOR('',#31281,1.);
#8842=VECTOR('',#31282,1.);
#8843=VECTOR('',#31285,1.);
#8844=VECTOR('',#31286,1.);
#8845=VECTOR('',#31287,1.);
#8846=VECTOR('',#31290,1.);
#8847=VECTOR('',#31291,1.);
#8848=VECTOR('',#31292,1.);
#8849=VECTOR('',#31293,1.);
#8850=VECTOR('',#31294,1.);
#8851=VECTOR('',#31295,1.);
#8852=VECTOR('',#31298,1.);
#8853=VECTOR('',#31299,1.);
#8854=VECTOR('',#31300,1.);
#8855=VECTOR('',#31303,1.);
#8856=VECTOR('',#31304,1.);
#8857=VECTOR('',#31305,1.);
#8858=VECTOR('',#31308,1.);
#8859=VECTOR('',#31309,1.);
#8860=VECTOR('',#31312,1.);
#8861=VECTOR('',#31313,1.);
#8862=VECTOR('',#31314,1.);
#8863=VECTOR('',#31315,1.);
#8864=VECTOR('',#31316,1.);
#8865=VECTOR('',#31317,1.);
#8866=VECTOR('',#31320,1.);
#8867=VECTOR('',#31321,1.);
#8868=VECTOR('',#31322,1.);
#8869=VECTOR('',#31325,1.);
#8870=VECTOR('',#31326,1.);
#8871=VECTOR('',#31327,1.);
#8872=VECTOR('',#31328,1.);
#8873=VECTOR('',#31331,1.);
#8874=VECTOR('',#31332,1.);
#8875=VECTOR('',#31333,1.);
#8876=VECTOR('',#31336,1.);
#8877=VECTOR('',#31337,1.);
#8878=VECTOR('',#31338,1.);
#8879=VECTOR('',#31339,1.);
#8880=VECTOR('',#31340,1.);
#8881=VECTOR('',#31341,1.);
#8882=VECTOR('',#31344,1.);
#8883=VECTOR('',#31345,1.);
#8884=VECTOR('',#31346,1.);
#8885=VECTOR('',#31347,1.);
#8886=VECTOR('',#31350,1.);
#8887=VECTOR('',#31351,1.);
#8888=VECTOR('',#31352,1.);
#8889=VECTOR('',#31353,1.);
#8890=VECTOR('',#31356,1.);
#8891=VECTOR('',#31357,1.);
#8892=VECTOR('',#31360,1.);
#8893=VECTOR('',#31361,1.);
#8894=VECTOR('',#31362,1.);
#8895=VECTOR('',#31363,1.);
#8896=VECTOR('',#31366,1.);
#8897=VECTOR('',#31367,1.);
#8898=VECTOR('',#31368,1.);
#8899=VECTOR('',#31371,1.);
#8900=VECTOR('',#31372,1.);
#8901=VECTOR('',#31373,1.);
#8902=VECTOR('',#31374,1.);
#8903=VECTOR('',#31375,1.);
#8904=VECTOR('',#31376,1.);
#8905=VECTOR('',#31379,1.);
#8906=VECTOR('',#31380,1.);
#8907=VECTOR('',#31381,1.);
#8908=VECTOR('',#31384,1.);
#8909=VECTOR('',#31385,1.);
#8910=VECTOR('',#31386,1.);
#8911=VECTOR('',#31389,1.);
#8912=VECTOR('',#31390,1.);
#8913=VECTOR('',#31393,1.);
#8914=VECTOR('',#31394,1.);
#8915=VECTOR('',#31395,1.);
#8916=VECTOR('',#31396,1.);
#8917=VECTOR('',#31397,1.);
#8918=VECTOR('',#31398,1.);
#8919=VECTOR('',#31401,1.);
#8920=VECTOR('',#31402,1.);
#8921=VECTOR('',#31403,1.);
#8922=VECTOR('',#31404,1.);
#8923=VECTOR('',#31407,1.);
#8924=VECTOR('',#31408,1.);
#8925=VECTOR('',#31409,1.);
#8926=VECTOR('',#31410,1.);
#8927=VECTOR('',#31413,1.);
#8928=VECTOR('',#31414,1.);
#8929=VECTOR('',#31417,1.);
#8930=VECTOR('',#31418,1.);
#8931=VECTOR('',#31419,1.);
#8932=VECTOR('',#31420,1.);
#8933=VECTOR('',#31423,1.);
#8934=VECTOR('',#31424,1.);
#8935=VECTOR('',#31425,1.);
#8936=VECTOR('',#31428,1.);
#8937=VECTOR('',#31429,1.);
#8938=VECTOR('',#31430,1.);
#8939=VECTOR('',#31431,1.);
#8940=VECTOR('',#31432,1.);
#8941=VECTOR('',#31433,1.);
#8942=VECTOR('',#31436,1.);
#8943=VECTOR('',#31437,1.);
#8944=VECTOR('',#31438,1.);
#8945=VECTOR('',#31441,1.);
#8946=VECTOR('',#31442,1.);
#8947=VECTOR('',#31443,1.);
#8948=VECTOR('',#31446,1.);
#8949=VECTOR('',#31447,1.);
#8950=VECTOR('',#31448,1.);
#8951=VECTOR('',#31449,1.);
#8952=VECTOR('',#31452,1.);
#8953=VECTOR('',#31453,1.);
#8954=VECTOR('',#31454,1.);
#8955=VECTOR('',#31455,1.);
#8956=VECTOR('',#31456,1.);
#8957=VECTOR('',#31459,1.);
#8958=VECTOR('',#31460,1.);
#8959=VECTOR('',#31461,1.);
#8960=VECTOR('',#31464,1.);
#8961=VECTOR('',#31465,1.);
#8962=VECTOR('',#31466,1.);
#8963=VECTOR('',#31469,1.);
#8964=VECTOR('',#31470,1.);
#8965=VECTOR('',#31471,1.);
#8966=VECTOR('',#31474,1.);
#8967=VECTOR('',#31475,1.);
#8968=VECTOR('',#31476,1.);
#8969=VECTOR('',#31477,1.);
#8970=VECTOR('',#31478,1.);
#8971=VECTOR('',#31479,1.);
#8972=VECTOR('',#31482,1.);
#8973=VECTOR('',#31483,1.);
#8974=VECTOR('',#31484,1.);
#8975=VECTOR('',#31485,1.);
#8976=VECTOR('',#31488,1.);
#8977=VECTOR('',#31489,1.);
#8978=VECTOR('',#31490,1.);
#8979=VECTOR('',#31491,1.);
#8980=VECTOR('',#31494,1.);
#8981=VECTOR('',#31495,1.);
#8982=VECTOR('',#31498,1.);
#8983=VECTOR('',#31499,1.);
#8984=VECTOR('',#31500,1.);
#8985=VECTOR('',#31501,1.);
#8986=VECTOR('',#31504,1.);
#8987=VECTOR('',#31505,1.);
#8988=VECTOR('',#31506,1.);
#8989=VECTOR('',#31509,1.);
#8990=VECTOR('',#31510,1.);
#8991=VECTOR('',#31511,1.);
#8992=VECTOR('',#31512,1.);
#8993=VECTOR('',#31513,1.);
#8994=VECTOR('',#31514,1.);
#8995=VECTOR('',#31517,1.);
#8996=VECTOR('',#31518,1.);
#8997=VECTOR('',#31519,1.);
#8998=VECTOR('',#31520,1.);
#8999=VECTOR('',#31523,1.);
#9000=VECTOR('',#31524,1.);
#9001=VECTOR('',#31525,1.);
#9002=VECTOR('',#31526,1.);
#9003=VECTOR('',#31529,1.);
#9004=VECTOR('',#31530,1.);
#9005=VECTOR('',#31533,1.);
#9006=VECTOR('',#31534,1.);
#9007=VECTOR('',#31535,1.);
#9008=VECTOR('',#31536,1.);
#9009=VECTOR('',#31539,1.);
#9010=VECTOR('',#31540,1.);
#9011=VECTOR('',#31541,1.);
#9012=VECTOR('',#31544,1.);
#9013=VECTOR('',#31545,1.);
#9014=VECTOR('',#31546,1.);
#9015=VECTOR('',#31547,1.);
#9016=VECTOR('',#31548,1.);
#9017=VECTOR('',#31549,1.);
#9018=VECTOR('',#31552,1.);
#9019=VECTOR('',#31553,1.);
#9020=VECTOR('',#31554,1.);
#9021=VECTOR('',#31555,1.);
#9022=VECTOR('',#31558,1.);
#9023=VECTOR('',#31559,1.);
#9024=VECTOR('',#31562,1.);
#9025=VECTOR('',#31563,1.);
#9026=VECTOR('',#31564,1.);
#9027=VECTOR('',#31567,1.);
#9028=VECTOR('',#31568,1.);
#9029=VECTOR('',#31569,1.);
#9030=VECTOR('',#31570,1.);
#9031=VECTOR('',#31571,1.);
#9032=VECTOR('',#31572,1.);
#9033=VECTOR('',#31575,1.);
#9034=VECTOR('',#31576,1.);
#9035=VECTOR('',#31577,1.);
#9036=VECTOR('',#31578,1.);
#9037=VECTOR('',#31581,1.);
#9038=VECTOR('',#31582,1.);
#9039=VECTOR('',#31583,1.);
#9040=VECTOR('',#31584,1.);
#9041=VECTOR('',#31587,1.);
#9042=VECTOR('',#31588,1.);
#9043=VECTOR('',#31591,1.);
#9044=VECTOR('',#31592,1.);
#9045=VECTOR('',#31593,1.);
#9046=VECTOR('',#31594,1.);
#9047=VECTOR('',#31597,1.);
#9048=VECTOR('',#31598,1.);
#9049=VECTOR('',#31599,1.);
#9050=VECTOR('',#31602,1.);
#9051=VECTOR('',#31603,1.);
#9052=VECTOR('',#31604,1.);
#9053=VECTOR('',#31605,1.);
#9054=VECTOR('',#31606,1.);
#9055=VECTOR('',#31607,1.);
#9056=VECTOR('',#31610,1.);
#9057=VECTOR('',#31611,1.);
#9058=VECTOR('',#31612,1.);
#9059=VECTOR('',#31613,1.);
#9060=VECTOR('',#31616,1.);
#9061=VECTOR('',#31617,1.);
#9062=VECTOR('',#31618,1.);
#9063=VECTOR('',#31619,1.);
#9064=VECTOR('',#31622,1.);
#9065=VECTOR('',#31623,1.);
#9066=VECTOR('',#31626,1.);
#9067=VECTOR('',#31627,1.);
#9068=VECTOR('',#31628,1.);
#9069=VECTOR('',#31629,1.);
#9070=VECTOR('',#31632,1.);
#9071=VECTOR('',#31633,1.);
#9072=VECTOR('',#31634,1.);
#9073=VECTOR('',#31637,1.);
#9074=VECTOR('',#31638,1.);
#9075=VECTOR('',#31639,1.);
#9076=VECTOR('',#31640,1.);
#9077=VECTOR('',#31641,1.);
#9078=VECTOR('',#31644,1.);
#9079=VECTOR('',#31645,1.);
#9080=VECTOR('',#31646,1.);
#9081=VECTOR('',#31649,1.);
#9082=VECTOR('',#31650,1.);
#9083=VECTOR('',#31653,1.);
#9084=VECTOR('',#31654,1.);
#9085=VECTOR('',#31655,1.);
#9086=VECTOR('',#31658,1.);
#9087=VECTOR('',#31659,1.);
#9088=VECTOR('',#31660,1.);
#9089=VECTOR('',#31661,1.);
#9090=VECTOR('',#31664,1.);
#9091=VECTOR('',#31665,1.);
#9092=VECTOR('',#31666,1.);
#9093=VECTOR('',#31671,1.);
#9094=VECTOR('',#31672,1.);
#9095=VECTOR('',#31673,1.);
#9096=VECTOR('',#31674,1.);
#9097=VECTOR('',#31677,1.);
#9098=VECTOR('',#31678,1.);
#9099=VECTOR('',#31679,1.);
#9100=VECTOR('',#31680,1.);
#9101=VECTOR('',#31681,1.);
#9102=VECTOR('',#31682,1.);
#9103=VECTOR('',#31685,1.);
#9104=VECTOR('',#31686,1.);
#9105=VECTOR('',#31689,1.);
#9106=VECTOR('',#31690,1.);
#9107=VECTOR('',#31691,1.);
#9108=VECTOR('',#31692,1.);
#9109=VECTOR('',#31693,1.);
#9110=VECTOR('',#31696,1.);
#9111=VECTOR('',#31697,1.);
#9112=VECTOR('',#31698,1.);
#9113=VECTOR('',#31699,1.);
#9114=VECTOR('',#31702,1.);
#9115=VECTOR('',#31705,1.);
#9116=VECTOR('',#31706,1.);
#9117=VECTOR('',#31707,1.);
#9118=VECTOR('',#31708,1.);
#9119=VECTOR('',#31709,1.);
#9120=VECTOR('',#31710,1.);
#9121=VECTOR('',#31713,1.);
#9122=VECTOR('',#31714,1.);
#9123=VECTOR('',#31715,1.);
#9124=VECTOR('',#31716,1.);
#9125=VECTOR('',#31719,1.);
#9126=VECTOR('',#31720,1.);
#9127=VECTOR('',#31721,1.);
#9128=VECTOR('',#31722,1.);
#9129=VECTOR('',#31725,1.);
#9130=VECTOR('',#31726,1.);
#9131=VECTOR('',#31729,1.);
#9132=VECTOR('',#31730,1.);
#9133=VECTOR('',#31731,1.);
#9134=VECTOR('',#31732,1.);
#9135=VECTOR('',#31733,1.);
#9136=VECTOR('',#31734,1.);
#9137=VECTOR('',#31737,1.);
#9138=VECTOR('',#31738,1.);
#9139=VECTOR('',#31739,1.);
#9140=VECTOR('',#31740,1.);
#9141=VECTOR('',#31743,1.);
#9142=VECTOR('',#31744,1.);
#9143=VECTOR('',#31745,1.);
#9144=VECTOR('',#31746,1.);
#9145=VECTOR('',#31749,1.);
#9146=VECTOR('',#31750,1.);
#9147=VECTOR('',#31753,1.);
#9148=VECTOR('',#31754,1.);
#9149=VECTOR('',#31755,1.);
#9150=VECTOR('',#31756,1.);
#9151=VECTOR('',#31759,1.);
#9152=VECTOR('',#31760,1.);
#9153=VECTOR('',#31761,1.);
#9154=VECTOR('',#31764,1.);
#9155=VECTOR('',#31765,1.);
#9156=VECTOR('',#31766,1.);
#9157=VECTOR('',#31767,1.);
#9158=VECTOR('',#31768,1.);
#9159=VECTOR('',#31769,1.);
#9160=VECTOR('',#31772,1.);
#9161=VECTOR('',#31773,1.);
#9162=VECTOR('',#31774,1.);
#9163=VECTOR('',#31775,1.);
#9164=VECTOR('',#31778,1.);
#9165=VECTOR('',#31779,1.);
#9166=VECTOR('',#31780,1.);
#9167=VECTOR('',#31781,1.);
#9168=VECTOR('',#31784,1.);
#9169=VECTOR('',#31785,1.);
#9170=VECTOR('',#31788,1.);
#9171=VECTOR('',#31789,1.);
#9172=VECTOR('',#31790,1.);
#9173=VECTOR('',#31791,1.);
#9174=VECTOR('',#31794,1.);
#9175=VECTOR('',#31795,1.);
#9176=VECTOR('',#31796,1.);
#9177=VECTOR('',#31799,1.);
#9178=VECTOR('',#31800,1.);
#9179=VECTOR('',#31801,1.);
#9180=VECTOR('',#31802,1.);
#9181=VECTOR('',#31803,1.);
#9182=VECTOR('',#31804,1.);
#9183=VECTOR('',#31807,1.);
#9184=VECTOR('',#31808,1.);
#9185=VECTOR('',#31809,1.);
#9186=VECTOR('',#31810,1.);
#9187=VECTOR('',#31813,1.);
#9188=VECTOR('',#31814,1.);
#9189=VECTOR('',#31815,1.);
#9190=VECTOR('',#31816,1.);
#9191=VECTOR('',#31819,1.);
#9192=VECTOR('',#31820,1.);
#9193=VECTOR('',#31823,1.);
#9194=VECTOR('',#31824,1.);
#9195=VECTOR('',#31825,1.);
#9196=VECTOR('',#31826,1.);
#9197=VECTOR('',#31829,1.);
#9198=VECTOR('',#31830,1.);
#9199=VECTOR('',#31831,1.);
#9200=VECTOR('',#31834,1.);
#9201=VECTOR('',#31835,1.);
#9202=VECTOR('',#31836,1.);
#9203=VECTOR('',#31837,1.);
#9204=VECTOR('',#31838,1.);
#9205=VECTOR('',#31839,1.);
#9206=VECTOR('',#31842,1.);
#9207=VECTOR('',#31843,1.);
#9208=VECTOR('',#31844,1.);
#9209=VECTOR('',#31845,1.);
#9210=VECTOR('',#31848,1.);
#9211=VECTOR('',#31849,1.);
#9212=VECTOR('',#31850,1.);
#9213=VECTOR('',#31851,1.);
#9214=VECTOR('',#31854,1.);
#9215=VECTOR('',#31855,1.);
#9216=VECTOR('',#31858,1.);
#9217=VECTOR('',#31859,1.);
#9218=VECTOR('',#31860,1.);
#9219=VECTOR('',#31861,1.);
#9220=VECTOR('',#31864,1.);
#9221=VECTOR('',#31865,1.);
#9222=VECTOR('',#31866,1.);
#9223=VECTOR('',#31869,1.);
#9224=VECTOR('',#31870,1.);
#9225=VECTOR('',#31871,1.);
#9226=VECTOR('',#31872,1.);
#9227=VECTOR('',#31873,1.);
#9228=VECTOR('',#31874,1.);
#9229=VECTOR('',#31877,1.);
#9230=VECTOR('',#31878,1.);
#9231=VECTOR('',#31879,1.);
#9232=VECTOR('',#31882,1.);
#9233=VECTOR('',#31883,1.);
#9234=VECTOR('',#31884,1.);
#9235=VECTOR('',#31887,1.);
#9236=VECTOR('',#31888,1.);
#9237=VECTOR('',#31891,1.);
#9238=VECTOR('',#31892,1.);
#9239=VECTOR('',#31895,1.);
#9240=VECTOR('',#31896,1.);
#9241=VECTOR('',#31899,1.);
#9242=VECTOR('',#31902,1.);
#9243=VECTOR('',#31903,1.);
#9244=VECTOR('',#31906,1.);
#9245=VECTOR('',#31907,1.);
#9246=VECTOR('',#31910,1.);
#9247=VECTOR('',#31911,1.);
#9248=VECTOR('',#31914,1.);
#9249=VECTOR('',#31917,1.);
#9250=VECTOR('',#31918,1.);
#9251=VECTOR('',#31921,1.);
#9252=VECTOR('',#31922,1.);
#9253=VECTOR('',#31925,1.);
#9254=VECTOR('',#31928,1.);
#9255=VECTOR('',#31929,1.);
#9256=VECTOR('',#31930,1.);
#9257=VECTOR('',#31931,1.);
#9258=VECTOR('',#31932,1.);
#9259=VECTOR('',#31933,1.);
#9260=VECTOR('',#31934,1.);
#9261=VECTOR('',#31935,1.);
#9262=VECTOR('',#31936,1.);
#9263=VECTOR('',#31937,1.);
#9264=VECTOR('',#31938,1.);
#9265=VECTOR('',#31939,1.);
#9266=VECTOR('',#31940,1.);
#9267=VECTOR('',#31941,1.);
#9268=VECTOR('',#31942,1.);
#9269=VECTOR('',#31943,1.);
#9270=VECTOR('',#31944,1.);
#9271=VECTOR('',#31945,1.);
#9272=VECTOR('',#31946,1.);
#9273=VECTOR('',#31947,1.);
#9274=VECTOR('',#31948,1.);
#9275=VECTOR('',#31949,1.);
#9276=VECTOR('',#31950,1.);
#9277=VECTOR('',#31951,1.);
#9278=VECTOR('',#31952,1.);
#9279=VECTOR('',#31953,1.);
#9280=VECTOR('',#31954,1.);
#9281=VECTOR('',#31955,1.);
#9282=VECTOR('',#31956,1.);
#9283=VECTOR('',#31957,1.);
#9284=VECTOR('',#31958,1.);
#9285=VECTOR('',#31959,1.);
#9286=VECTOR('',#31960,1.);
#9287=VECTOR('',#31961,1.);
#9288=VECTOR('',#31962,1.);
#9289=VECTOR('',#31963,1.);
#9290=VECTOR('',#31964,1.);
#9291=VECTOR('',#31965,1.);
#9292=VECTOR('',#31966,1.);
#9293=VECTOR('',#31967,1.);
#9294=VECTOR('',#31968,1.);
#9295=VECTOR('',#31969,1.);
#9296=VECTOR('',#31970,1.);
#9297=VECTOR('',#31971,1.);
#9298=VECTOR('',#31972,1.);
#9299=VECTOR('',#31973,1.);
#9300=VECTOR('',#31974,1.);
#9301=VECTOR('',#31975,1.);
#9302=VECTOR('',#31976,1.);
#9303=VECTOR('',#31977,1.);
#9304=VECTOR('',#31978,1.);
#9305=VECTOR('',#31979,1.);
#9306=VECTOR('',#31980,1.);
#9307=VECTOR('',#31981,1.);
#9308=VECTOR('',#31982,1.);
#9309=VECTOR('',#31983,1.);
#9310=VECTOR('',#31984,1.);
#9311=VECTOR('',#31985,1.);
#9312=VECTOR('',#31986,1.);
#9313=VECTOR('',#31987,1.);
#9314=VECTOR('',#31988,1.);
#9315=VECTOR('',#31989,1.);
#9316=VECTOR('',#31990,1.);
#9317=VECTOR('',#31991,1.);
#9318=VECTOR('',#31992,1.);
#9319=VECTOR('',#31993,1.);
#9320=VECTOR('',#31994,1.);
#9321=VECTOR('',#31995,1.);
#9322=VECTOR('',#31996,1.);
#9323=VECTOR('',#31997,1.);
#9324=VECTOR('',#31998,1.);
#9325=VECTOR('',#31999,1.);
#9326=VECTOR('',#32000,1.);
#9327=VECTOR('',#32001,1.);
#9328=VECTOR('',#32002,1.);
#9329=VECTOR('',#32005,1.);
#9330=VECTOR('',#32008,1.);
#9331=VECTOR('',#32009,1.);
#9332=VECTOR('',#32012,1.);
#9333=VECTOR('',#32015,1.);
#9334=VECTOR('',#32018,1.);
#9335=VECTOR('',#32019,1.);
#9336=VECTOR('',#32022,1.);
#9337=VECTOR('',#32023,1.);
#9338=VECTOR('',#32026,1.);
#9339=VECTOR('',#32029,1.);
#9340=VECTOR('',#32032,1.);
#9341=VECTOR('',#32033,1.);
#9342=VECTOR('',#32036,1.);
#9343=VECTOR('',#32037,1.);
#9344=VECTOR('',#32040,1.);
#9345=VECTOR('',#32043,1.);
#9346=VECTOR('',#32046,1.);
#9347=VECTOR('',#32047,1.);
#9348=VECTOR('',#32050,1.);
#9349=VECTOR('',#32051,1.);
#9350=VECTOR('',#32054,1.);
#9351=VECTOR('',#32057,1.);
#9352=VECTOR('',#32058,1.);
#9353=VECTOR('',#32061,1.);
#9354=VECTOR('',#32062,1.);
#9355=VECTOR('',#32065,1.);
#9356=VECTOR('',#32066,1.);
#9357=VECTOR('',#32069,1.);
#9358=VECTOR('',#32070,1.);
#9359=VECTOR('',#32071,1.);
#9360=VECTOR('',#32072,1.);
#9361=VECTOR('',#32075,1.);
#9362=VECTOR('',#32076,1.);
#9363=VECTOR('',#32077,1.);
#9364=VECTOR('',#32078,1.);
#9365=VECTOR('',#32081,1.);
#9366=VECTOR('',#32082,1.);
#9367=VECTOR('',#32085,1.);
#9368=VECTOR('',#32086,1.);
#9369=VECTOR('',#32087,1.);
#9370=VECTOR('',#32090,1.);
#9371=VECTOR('',#32091,1.);
#9372=VECTOR('',#32092,1.);
#9373=VECTOR('',#32095,1.);
#9374=VECTOR('',#32096,1.);
#9375=VECTOR('',#32097,1.);
#9376=VECTOR('',#32100,1.);
#9377=VECTOR('',#32101,1.);
#9378=VECTOR('',#32102,1.);
#9379=VECTOR('',#32103,1.);
#9380=VECTOR('',#32106,1.);
#9381=VECTOR('',#32107,1.);
#9382=VECTOR('',#32110,1.);
#9383=VECTOR('',#32111,1.);
#9384=VECTOR('',#32112,1.);
#9385=VECTOR('',#32113,1.);
#9386=VECTOR('',#32114,1.);
#9387=VECTOR('',#32115,1.);
#9388=VECTOR('',#32118,1.);
#9389=VECTOR('',#32119,1.);
#9390=VECTOR('',#32120,1.);
#9391=VECTOR('',#32123,1.);
#9392=VECTOR('',#32124,1.);
#9393=VECTOR('',#32125,1.);
#9394=VECTOR('',#32128,1.);
#9395=VECTOR('',#32129,1.);
#9396=VECTOR('',#32132,1.);
#9397=VECTOR('',#32133,1.);
#9398=VECTOR('',#32134,1.);
#9399=VECTOR('',#32135,1.);
#9400=VECTOR('',#32138,1.);
#9401=VECTOR('',#32141,1.);
#9402=VECTOR('',#32144,1.);
#9403=VECTOR('',#32147,1.);
#9404=VECTOR('',#32148,1.);
#9405=VECTOR('',#32151,1.);
#9406=VECTOR('',#32152,1.);
#9407=VECTOR('',#32155,1.);
#9408=VECTOR('',#32158,1.);
#9409=VECTOR('',#32161,1.);
#9410=VECTOR('',#32162,1.);
#9411=VECTOR('',#32165,1.);
#9412=VECTOR('',#32168,1.);
#9413=VECTOR('',#32171,1.);
#9414=VECTOR('',#32172,1.);
#9415=VECTOR('',#32175,1.);
#9416=VECTOR('',#32176,1.);
#9417=VECTOR('',#32179,1.);
#9418=VECTOR('',#32182,1.);
#9419=VECTOR('',#32185,1.);
#9420=VECTOR('',#32188,1.);
#9421=VECTOR('',#32189,1.);
#9422=VECTOR('',#32192,1.);
#9423=VECTOR('',#32195,1.);
#9424=VECTOR('',#32198,1.);
#9425=VECTOR('',#32199,1.);
#9426=VECTOR('',#32202,1.);
#9427=VECTOR('',#32205,1.);
#9428=VECTOR('',#32208,1.);
#9429=VECTOR('',#32209,1.);
#9430=VECTOR('',#32212,1.);
#9431=VECTOR('',#32215,1.);
#9432=VECTOR('',#32218,1.);
#9433=VECTOR('',#32219,1.);
#9434=VECTOR('',#32222,1.);
#9435=VECTOR('',#32225,1.);
#9436=VECTOR('',#32228,1.);
#9437=VECTOR('',#32229,1.);
#9438=VECTOR('',#32232,1.);
#9439=VECTOR('',#32233,1.);
#9440=VECTOR('',#32236,1.);
#9441=VECTOR('',#32239,1.);
#9442=VECTOR('',#32240,1.);
#9443=VECTOR('',#32241,1.);
#9444=VECTOR('',#32242,1.);
#9445=VECTOR('',#32243,1.);
#9446=VECTOR('',#32244,1.);
#9447=VECTOR('',#32247,1.);
#9448=VECTOR('',#32248,1.);
#9449=VECTOR('',#32249,1.);
#9450=VECTOR('',#32252,1.);
#9451=VECTOR('',#32253,1.);
#9452=VECTOR('',#32254,1.);
#9453=VECTOR('',#32257,1.);
#9454=VECTOR('',#32258,1.);
#9455=VECTOR('',#32261,1.);
#9456=VECTOR('',#32262,1.);
#9457=VECTOR('',#32263,1.);
#9458=VECTOR('',#32264,1.);
#9459=VECTOR('',#32267,1.);
#9460=VECTOR('',#32268,1.);
#9461=VECTOR('',#32271,1.);
#9462=VECTOR('',#32272,1.);
#9463=VECTOR('',#32273,1.);
#9464=VECTOR('',#32274,1.);
#9465=VECTOR('',#32275,1.);
#9466=VECTOR('',#32276,1.);
#9467=VECTOR('',#32279,1.);
#9468=VECTOR('',#32280,1.);
#9469=VECTOR('',#32281,1.);
#9470=VECTOR('',#32284,1.);
#9471=VECTOR('',#32285,1.);
#9472=VECTOR('',#32286,1.);
#9473=VECTOR('',#32289,1.);
#9474=VECTOR('',#32290,1.);
#9475=VECTOR('',#32293,1.);
#9476=VECTOR('',#32294,1.);
#9477=VECTOR('',#32295,1.);
#9478=VECTOR('',#32296,1.);
#9479=VECTOR('',#32299,1.);
#9480=VECTOR('',#32300,1.);
#9481=VECTOR('',#32303,1.);
#9482=VECTOR('',#32304,1.);
#9483=VECTOR('',#32305,1.);
#9484=VECTOR('',#32306,1.);
#9485=VECTOR('',#32307,1.);
#9486=VECTOR('',#32308,1.);
#9487=VECTOR('',#32311,1.);
#9488=VECTOR('',#32312,1.);
#9489=VECTOR('',#32313,1.);
#9490=VECTOR('',#32316,1.);
#9491=VECTOR('',#32317,1.);
#9492=VECTOR('',#32318,1.);
#9493=VECTOR('',#32321,1.);
#9494=VECTOR('',#32322,1.);
#9495=VECTOR('',#32325,1.);
#9496=VECTOR('',#32326,1.);
#9497=VECTOR('',#32327,1.);
#9498=VECTOR('',#32328,1.);
#9499=VECTOR('',#32331,1.);
#9500=VECTOR('',#32332,1.);
#9501=VECTOR('',#32335,1.);
#9502=VECTOR('',#32336,1.);
#9503=VECTOR('',#32337,1.);
#9504=VECTOR('',#32338,1.);
#9505=VECTOR('',#32339,1.);
#9506=VECTOR('',#32340,1.);
#9507=VECTOR('',#32343,1.);
#9508=VECTOR('',#32344,1.);
#9509=VECTOR('',#32345,1.);
#9510=VECTOR('',#32348,1.);
#9511=VECTOR('',#32349,1.);
#9512=VECTOR('',#32352,1.);
#9513=VECTOR('',#32353,1.);
#9514=VECTOR('',#32354,1.);
#9515=VECTOR('',#32357,1.);
#9516=VECTOR('',#32358,1.);
#9517=VECTOR('',#32359,1.);
#9518=VECTOR('',#32360,1.);
#9519=VECTOR('',#32361,1.);
#9520=VECTOR('',#32364,1.);
#9521=VECTOR('',#32365,1.);
#9522=VECTOR('',#32366,1.);
#9523=VECTOR('',#32369,1.);
#9524=VECTOR('',#32370,1.);
#9525=VECTOR('',#32371,1.);
#9526=VECTOR('',#32374,1.);
#9527=VECTOR('',#32375,1.);
#9528=VECTOR('',#32376,1.);
#9529=VECTOR('',#32379,1.);
#9530=VECTOR('',#32380,1.);
#9531=VECTOR('',#32381,1.);
#9532=VECTOR('',#32382,1.);
#9533=VECTOR('',#32383,1.);
#9534=VECTOR('',#32384,1.);
#9535=VECTOR('',#32387,1.);
#9536=VECTOR('',#32388,1.);
#9537=VECTOR('',#32389,1.);
#9538=VECTOR('',#32392,1.);
#9539=VECTOR('',#32393,1.);
#9540=VECTOR('',#32394,1.);
#9541=VECTOR('',#32397,1.);
#9542=VECTOR('',#32398,1.);
#9543=VECTOR('',#32401,1.);
#9544=VECTOR('',#32402,1.);
#9545=VECTOR('',#32403,1.);
#9546=VECTOR('',#32404,1.);
#9547=VECTOR('',#32407,1.);
#9548=VECTOR('',#32408,1.);
#9549=VECTOR('',#32411,1.);
#9550=VECTOR('',#32412,1.);
#9551=VECTOR('',#32413,1.);
#9552=VECTOR('',#32414,1.);
#9553=VECTOR('',#32415,1.);
#9554=VECTOR('',#32416,1.);
#9555=VECTOR('',#32419,1.);
#9556=VECTOR('',#32420,1.);
#9557=VECTOR('',#32421,1.);
#9558=VECTOR('',#32424,1.);
#9559=VECTOR('',#32425,1.);
#9560=VECTOR('',#32426,1.);
#9561=VECTOR('',#32429,1.);
#9562=VECTOR('',#32430,1.);
#9563=VECTOR('',#32433,1.);
#9564=VECTOR('',#32434,1.);
#9565=VECTOR('',#32435,1.);
#9566=VECTOR('',#32436,1.);
#9567=VECTOR('',#32439,1.);
#9568=VECTOR('',#32440,1.);
#9569=VECTOR('',#32443,1.);
#9570=VECTOR('',#32444,1.);
#9571=VECTOR('',#32445,1.);
#9572=VECTOR('',#32446,1.);
#9573=VECTOR('',#32449,1.);
#9574=VECTOR('',#32450,1.);
#9575=VECTOR('',#32451,1.);
#9576=VECTOR('',#32452,1.);
#9577=VECTOR('',#32455,1.);
#9578=VECTOR('',#32456,1.);
#9579=VECTOR('',#32459,1.);
#9580=VECTOR('',#32462,1.);
#9581=VECTOR('',#32465,1.);
#9582=VECTOR('',#32466,1.);
#9583=VECTOR('',#32469,1.);
#9584=VECTOR('',#32472,1.);
#9585=VECTOR('',#32475,1.);
#9586=VECTOR('',#32476,1.);
#9587=VECTOR('',#32479,1.);
#9588=VECTOR('',#32480,1.);
#9589=VECTOR('',#32483,1.);
#9590=VECTOR('',#32486,1.);
#9591=VECTOR('',#32489,1.);
#9592=VECTOR('',#32492,1.);
#9593=VECTOR('',#32493,1.);
#9594=VECTOR('',#32496,1.);
#9595=VECTOR('',#32499,1.);
#9596=VECTOR('',#32502,1.);
#9597=VECTOR('',#32503,1.);
#9598=VECTOR('',#32506,1.);
#9599=VECTOR('',#32509,1.);
#9600=VECTOR('',#32512,1.);
#9601=VECTOR('',#32513,1.);
#9602=VECTOR('',#32516,1.);
#9603=VECTOR('',#32517,1.);
#9604=VECTOR('',#32520,1.);
#9605=VECTOR('',#32523,1.);
#9606=VECTOR('',#32526,1.);
#9607=VECTOR('',#32527,1.);
#9608=VECTOR('',#32530,1.);
#9609=VECTOR('',#32531,1.);
#9610=VECTOR('',#32534,1.);
#9611=VECTOR('',#32537,1.);
#9612=VECTOR('',#32540,1.);
#9613=VECTOR('',#32541,1.);
#9614=VECTOR('',#32544,1.);
#9615=VECTOR('',#32547,1.);
#9616=VECTOR('',#32550,1.);
#9617=VECTOR('',#32551,1.);
#9618=VECTOR('',#32554,1.);
#9619=VECTOR('',#32557,1.);
#9620=VECTOR('',#32560,1.);
#9621=VECTOR('',#32561,1.);
#9622=VECTOR('',#32564,1.);
#9623=VECTOR('',#32565,1.);
#9624=VECTOR('',#32568,1.);
#9625=VECTOR('',#32571,1.);
#9626=VECTOR('',#32572,1.);
#9627=VECTOR('',#32573,1.);
#9628=VECTOR('',#32574,1.);
#9629=VECTOR('',#32575,1.);
#9630=VECTOR('',#32576,1.);
#9631=VECTOR('',#32579,1.);
#9632=VECTOR('',#32580,1.);
#9633=VECTOR('',#32581,1.);
#9634=VECTOR('',#32584,1.);
#9635=VECTOR('',#32585,1.);
#9636=VECTOR('',#32586,1.);
#9637=VECTOR('',#32589,1.);
#9638=VECTOR('',#32590,1.);
#9639=VECTOR('',#32593,1.);
#9640=VECTOR('',#32594,1.);
#9641=VECTOR('',#32595,1.);
#9642=VECTOR('',#32596,1.);
#9643=VECTOR('',#32599,1.);
#9644=VECTOR('',#32600,1.);
#9645=VECTOR('',#32603,1.);
#9646=VECTOR('',#32604,1.);
#9647=VECTOR('',#32605,1.);
#9648=VECTOR('',#32606,1.);
#9649=VECTOR('',#32607,1.);
#9650=VECTOR('',#32608,1.);
#9651=VECTOR('',#32611,1.);
#9652=VECTOR('',#32612,1.);
#9653=VECTOR('',#32613,1.);
#9654=VECTOR('',#32616,1.);
#9655=VECTOR('',#32617,1.);
#9656=VECTOR('',#32618,1.);
#9657=VECTOR('',#32621,1.);
#9658=VECTOR('',#32622,1.);
#9659=VECTOR('',#32625,1.);
#9660=VECTOR('',#32626,1.);
#9661=VECTOR('',#32627,1.);
#9662=VECTOR('',#32628,1.);
#9663=VECTOR('',#32631,1.);
#9664=VECTOR('',#32632,1.);
#9665=VECTOR('',#32635,1.);
#9666=VECTOR('',#32636,1.);
#9667=VECTOR('',#32637,1.);
#9668=VECTOR('',#32638,1.);
#9669=VECTOR('',#32639,1.);
#9670=VECTOR('',#32640,1.);
#9671=VECTOR('',#32643,1.);
#9672=VECTOR('',#32644,1.);
#9673=VECTOR('',#32645,1.);
#9674=VECTOR('',#32648,1.);
#9675=VECTOR('',#32649,1.);
#9676=VECTOR('',#32650,1.);
#9677=VECTOR('',#32653,1.);
#9678=VECTOR('',#32654,1.);
#9679=VECTOR('',#32657,1.);
#9680=VECTOR('',#32658,1.);
#9681=VECTOR('',#32659,1.);
#9682=VECTOR('',#32660,1.);
#9683=VECTOR('',#32663,1.);
#9684=VECTOR('',#32664,1.);
#9685=VECTOR('',#32667,1.);
#9686=VECTOR('',#32668,1.);
#9687=VECTOR('',#32669,1.);
#9688=VECTOR('',#32670,1.);
#9689=VECTOR('',#32671,1.);
#9690=VECTOR('',#32672,1.);
#9691=VECTOR('',#32675,1.);
#9692=VECTOR('',#32676,1.);
#9693=VECTOR('',#32677,1.);
#9694=VECTOR('',#32680,1.);
#9695=VECTOR('',#32681,1.);
#9696=VECTOR('',#32682,1.);
#9697=VECTOR('',#32685,1.);
#9698=VECTOR('',#32686,1.);
#9699=VECTOR('',#32689,1.);
#9700=VECTOR('',#32690,1.);
#9701=VECTOR('',#32691,1.);
#9702=VECTOR('',#32692,1.);
#9703=VECTOR('',#32695,1.);
#9704=VECTOR('',#32696,1.);
#9705=VECTOR('',#32699,1.);
#9706=VECTOR('',#32700,1.);
#9707=VECTOR('',#32701,1.);
#9708=VECTOR('',#32702,1.);
#9709=VECTOR('',#32703,1.);
#9710=VECTOR('',#32704,1.);
#9711=VECTOR('',#32707,1.);
#9712=VECTOR('',#32708,1.);
#9713=VECTOR('',#32709,1.);
#9714=VECTOR('',#32712,1.);
#9715=VECTOR('',#32713,1.);
#9716=VECTOR('',#32714,1.);
#9717=VECTOR('',#32717,1.);
#9718=VECTOR('',#32718,1.);
#9719=VECTOR('',#32721,1.);
#9720=VECTOR('',#32722,1.);
#9721=VECTOR('',#32723,1.);
#9722=VECTOR('',#32724,1.);
#9723=VECTOR('',#32727,1.);
#9724=VECTOR('',#32728,1.);
#9725=VECTOR('',#32731,1.);
#9726=VECTOR('',#32732,1.);
#9727=VECTOR('',#32733,1.);
#9728=VECTOR('',#32734,1.);
#9729=VECTOR('',#32735,1.);
#9730=VECTOR('',#32736,1.);
#9731=VECTOR('',#32739,1.);
#9732=VECTOR('',#32740,1.);
#9733=VECTOR('',#32741,1.);
#9734=VECTOR('',#32744,1.);
#9735=VECTOR('',#32745,1.);
#9736=VECTOR('',#32746,1.);
#9737=VECTOR('',#32749,1.);
#9738=VECTOR('',#32750,1.);
#9739=VECTOR('',#32753,1.);
#9740=VECTOR('',#32754,1.);
#9741=VECTOR('',#32755,1.);
#9742=VECTOR('',#32756,1.);
#9743=VECTOR('',#32759,1.);
#9744=VECTOR('',#32760,1.);
#9745=VECTOR('',#32763,1.);
#9746=VECTOR('',#32764,1.);
#9747=VECTOR('',#32765,1.);
#9748=VECTOR('',#32766,1.);
#9749=VECTOR('',#32769,1.);
#9750=VECTOR('',#32770,1.);
#9751=VECTOR('',#32771,1.);
#9752=VECTOR('',#32772,1.);
#9753=VECTOR('',#32775,1.);
#9754=VECTOR('',#32776,1.);
#9755=VECTOR('',#32779,1.);
#9756=VECTOR('',#32782,1.);
#9757=VECTOR('',#32785,1.);
#9758=VECTOR('',#32786,1.);
#9759=VECTOR('',#32789,1.);
#9760=VECTOR('',#32792,1.);
#9761=VECTOR('',#32795,1.);
#9762=VECTOR('',#32796,1.);
#9763=VECTOR('',#32799,1.);
#9764=VECTOR('',#32800,1.);
#9765=VECTOR('',#32803,1.);
#9766=VECTOR('',#32806,1.);
#9767=VECTOR('',#32809,1.);
#9768=VECTOR('',#32810,1.);
#9769=VECTOR('',#32813,1.);
#9770=VECTOR('',#32814,1.);
#9771=VECTOR('',#32817,1.);
#9772=VECTOR('',#32820,1.);
#9773=VECTOR('',#32823,1.);
#9774=VECTOR('',#32824,1.);
#9775=VECTOR('',#32827,1.);
#9776=VECTOR('',#32828,1.);
#9777=VECTOR('',#32831,1.);
#9778=VECTOR('',#32834,1.);
#9779=VECTOR('',#32837,1.);
#9780=VECTOR('',#32838,1.);
#9781=VECTOR('',#32841,1.);
#9782=VECTOR('',#32842,1.);
#9783=VECTOR('',#32845,1.);
#9784=VECTOR('',#32848,1.);
#9785=VECTOR('',#32851,1.);
#9786=VECTOR('',#32852,1.);
#9787=VECTOR('',#32855,1.);
#9788=VECTOR('',#32856,1.);
#9789=VECTOR('',#32859,1.);
#9790=VECTOR('',#32862,1.);
#9791=VECTOR('',#32863,1.);
#9792=VECTOR('',#32866,1.);
#9793=VECTOR('',#32867,1.);
#9794=VECTOR('',#32870,1.);
#9795=VECTOR('',#32873,1.);
#9796=VECTOR('',#32876,1.);
#9797=VECTOR('',#32877,1.);
#9798=VECTOR('',#32878,1.);
#9799=VECTOR('',#32881,1.);
#9800=VECTOR('',#32882,1.);
#9801=VECTOR('',#32885,1.);
#9802=VECTOR('',#32886,1.);
#9803=VECTOR('',#32889,1.);
#9804=VECTOR('',#32890,1.);
#9805=VECTOR('',#32891,1.);
#9806=VECTOR('',#32892,1.);
#9807=VECTOR('',#32893,1.);
#9808=VECTOR('',#32894,1.);
#9809=VECTOR('',#32895,1.);
#9810=VECTOR('',#32896,1.);
#9811=VECTOR('',#32897,1.);
#9812=VECTOR('',#32898,1.);
#9813=VECTOR('',#32899,1.);
#9814=VECTOR('',#32900,1.);
#9815=VECTOR('',#32901,1.);
#9816=VECTOR('',#32902,1.);
#9817=VECTOR('',#32903,1.);
#9818=VECTOR('',#32904,1.);
#9819=VECTOR('',#32905,1.);
#9820=VECTOR('',#32906,1.);
#9821=VECTOR('',#32907,1.);
#9822=VECTOR('',#32908,1.);
#9823=VECTOR('',#32909,1.);
#9824=VECTOR('',#32910,1.);
#9825=VECTOR('',#32911,1.);
#9826=VECTOR('',#32912,1.);
#9827=VECTOR('',#32913,1.);
#9828=VECTOR('',#32914,1.);
#9829=VECTOR('',#32915,1.);
#9830=VECTOR('',#32916,1.);
#9831=VECTOR('',#32917,1.);
#9832=VECTOR('',#32918,1.);
#9833=VECTOR('',#32919,1.);
#9834=VECTOR('',#32920,1.);
#9835=VECTOR('',#32921,1.);
#9836=VECTOR('',#32922,1.);
#9837=VECTOR('',#32923,1.);
#9838=VECTOR('',#32924,1.);
#9839=VECTOR('',#32925,1.);
#9840=VECTOR('',#32926,1.);
#9841=VECTOR('',#32927,1.);
#9842=VECTOR('',#32928,1.);
#9843=VECTOR('',#32929,1.);
#9844=VECTOR('',#32930,1.);
#9845=VECTOR('',#32931,1.);
#9846=VECTOR('',#32932,1.);
#9847=VECTOR('',#32933,1.);
#9848=VECTOR('',#32934,1.);
#9849=VECTOR('',#32935,1.);
#9850=VECTOR('',#32936,1.);
#9851=VECTOR('',#32937,1.);
#9852=VECTOR('',#32938,1.);
#9853=VECTOR('',#32939,1.);
#9854=VECTOR('',#32940,1.);
#9855=VECTOR('',#32941,1.);
#9856=VECTOR('',#32942,1.);
#9857=VECTOR('',#32943,1.);
#9858=VECTOR('',#32944,1.);
#9859=VECTOR('',#32945,1.);
#9860=VECTOR('',#32946,1.);
#9861=VECTOR('',#32947,1.);
#9862=VECTOR('',#32948,1.);
#9863=VECTOR('',#32949,1.);
#9864=VECTOR('',#32950,1.);
#9865=VECTOR('',#32951,1.);
#9866=VECTOR('',#32952,1.);
#9867=VECTOR('',#32953,1.);
#9868=VECTOR('',#32954,1.);
#9869=VECTOR('',#32955,1.);
#9870=VECTOR('',#32956,1.);
#9871=VECTOR('',#32957,1.);
#9872=VECTOR('',#32958,1.);
#9873=VECTOR('',#32959,1.);
#9874=VECTOR('',#32960,1.);
#9875=VECTOR('',#32961,1.);
#9876=VECTOR('',#32962,1.);
#9877=VECTOR('',#32963,1.);
#9878=VECTOR('',#32964,1.);
#9879=VECTOR('',#32965,1.);
#9880=VECTOR('',#32966,1.);
#9881=VECTOR('',#32967,1.);
#9882=VECTOR('',#32968,1.);
#9883=VECTOR('',#32969,1.);
#9884=VECTOR('',#32970,1.);
#9885=VECTOR('',#32971,1.);
#9886=VECTOR('',#32972,1.);
#9887=VECTOR('',#32973,1.);
#9888=VECTOR('',#32974,1.);
#9889=VECTOR('',#32975,1.);
#9890=VECTOR('',#32976,1.);
#9891=VECTOR('',#32977,1.);
#9892=VECTOR('',#32978,1.);
#9893=VECTOR('',#32979,1.);
#9894=VECTOR('',#32980,1.);
#9895=VECTOR('',#32981,1.);
#9896=VECTOR('',#32982,1.);
#9897=VECTOR('',#32983,1.);
#9898=VECTOR('',#32984,1.);
#9899=VECTOR('',#32985,1.);
#9900=VECTOR('',#32986,1.);
#9901=VECTOR('',#32987,1.);
#9902=VECTOR('',#32988,1.);
#9903=VECTOR('',#32989,1.);
#9904=VECTOR('',#32990,1.);
#9905=VECTOR('',#32991,1.);
#9906=VECTOR('',#32992,1.);
#9907=VECTOR('',#32993,1.);
#9908=VECTOR('',#32994,1.);
#9909=VECTOR('',#32995,1.);
#9910=VECTOR('',#32996,1.);
#9911=VECTOR('',#32997,1.);
#9912=VECTOR('',#32998,1.);
#9913=VECTOR('',#32999,1.);
#9914=VECTOR('',#33000,1.);
#9915=VECTOR('',#33001,1.);
#9916=VECTOR('',#33002,1.);
#9917=VECTOR('',#33007,1.);
#9918=VECTOR('',#33010,1.);
#9919=VECTOR('',#33011,1.);
#9920=VECTOR('',#33014,1.);
#9921=VECTOR('',#33017,1.);
#9922=VECTOR('',#33022,1.);
#9923=VECTOR('',#33023,1.);
#9924=VECTOR('',#33026,1.);
#9925=VECTOR('',#33029,1.);
#9926=VECTOR('',#33034,1.);
#9927=VECTOR('',#33035,1.);
#9928=VECTOR('',#33038,1.);
#9929=VECTOR('',#33041,1.);
#9930=VECTOR('',#33046,1.);
#9931=VECTOR('',#33049,1.);
#9932=VECTOR('',#33052,1.);
#9933=VECTOR('',#33055,1.);
#9934=VECTOR('',#33056,1.);
#9935=VECTOR('',#33059,1.);
#9936=VECTOR('',#33062,1.);
#9937=VECTOR('',#33067,1.);
#9938=VECTOR('',#33068,1.);
#9939=VECTOR('',#33073,1.);
#9940=VECTOR('',#33076,1.);
#9941=VECTOR('',#33079,1.);
#9942=VECTOR('',#33080,1.);
#9943=VECTOR('',#33083,1.);
#9944=VECTOR('',#33086,1.);
#9945=VECTOR('',#33091,1.);
#9946=VECTOR('',#33092,1.);
#9947=VECTOR('',#33095,1.);
#9948=VECTOR('',#33098,1.);
#9949=VECTOR('',#33103,1.);
#9950=VECTOR('',#33104,1.);
#9951=VECTOR('',#33107,1.);
#9952=VECTOR('',#33110,1.);
#9953=VECTOR('',#33115,1.);
#9954=VECTOR('',#33116,1.);
#9955=VECTOR('',#33119,1.);
#9956=VECTOR('',#33122,1.);
#9957=VECTOR('',#33127,1.);
#9958=VECTOR('',#33128,1.);
#9959=VECTOR('',#33131,1.);
#9960=VECTOR('',#33134,1.);
#9961=VECTOR('',#33139,1.);
#9962=VECTOR('',#33140,1.);
#9963=VECTOR('',#33147,1.);
#9964=VECTOR('',#33148,1.);
#9965=VECTOR('',#33151,1.);
#9966=VECTOR('',#33154,1.);
#9967=VECTOR('',#33159,1.);
#9968=VECTOR('',#33160,1.);
#9969=VECTOR('',#33163,1.);
#9970=VECTOR('',#33166,1.);
#9971=VECTOR('',#33171,1.);
#9972=VECTOR('',#33174,1.);
#9973=VECTOR('',#33177,1.);
#9974=VECTOR('',#33180,1.);
#9975=VECTOR('',#33181,1.);
#9976=VECTOR('',#33184,1.);
#9977=VECTOR('',#33187,1.);
#9978=VECTOR('',#33192,1.);
#9979=VECTOR('',#33193,1.);
#9980=VECTOR('',#33196,1.);
#9981=VECTOR('',#33199,1.);
#9982=VECTOR('',#33204,1.);
#9983=VECTOR('',#33205,1.);
#9984=VECTOR('',#33208,1.);
#9985=VECTOR('',#33213,1.);
#9986=VECTOR('',#33216,1.);
#9987=VECTOR('',#33219,1.);
#9988=VECTOR('',#33220,1.);
#9989=VECTOR('',#33223,1.);
#9990=VECTOR('',#33226,1.);
#9991=VECTOR('',#33231,1.);
#9992=VECTOR('',#33232,1.);
#9993=VECTOR('',#33239,1.);
#9994=VECTOR('',#33240,1.);
#9995=VECTOR('',#33243,1.);
#9996=VECTOR('',#33246,1.);
#9997=VECTOR('',#33251,1.);
#9998=VECTOR('',#33252,1.);
#9999=VECTOR('',#33255,1.);
#10000=VECTOR('',#33258,1.);
#10001=VECTOR('',#33263,1.);
#10002=VECTOR('',#33266,1.);
#10003=VECTOR('',#33269,1.);
#10004=VECTOR('',#33272,1.);
#10005=VECTOR('',#33273,1.);
#10006=VECTOR('',#33276,1.);
#10007=VECTOR('',#33281,1.);
#10008=VECTOR('',#33284,1.);
#10009=VECTOR('',#33287,1.);
#10010=VECTOR('',#33288,1.);
#10011=VECTOR('',#33291,1.);
#10012=VECTOR('',#33294,1.);
#10013=VECTOR('',#33299,1.);
#10014=VECTOR('',#33300,1.);
#10015=VECTOR('',#33307,1.);
#10016=VECTOR('',#33308,1.);
#10017=VECTOR('',#33311,1.);
#10018=VECTOR('',#33312,1.);
#10019=VECTOR('',#33315,1.);
#10020=VECTOR('',#33318,1.);
#10021=VECTOR('',#33323,1.);
#10022=VECTOR('',#33324,1.);
#10023=VECTOR('',#33327,1.);
#10024=VECTOR('',#33332,1.);
#10025=VECTOR('',#33337,0.805);
#10026=VECTOR('',#33342,1.755);
#10027=VECTOR('',#33347,0.855000000000001);
#10028=VECTOR('',#33350,1.83);
#10029=VECTOR('',#33353,1.755);
#10030=VECTOR('',#33356,1.);
#10031=VECTOR('',#33357,1.);
#10032=VECTOR('',#33360,1.);
#10033=VECTOR('',#33363,1.);
#10034=VECTOR('',#33364,1.);
#10035=VECTOR('',#33379,1.);
#10036=VECTOR('',#33388,1.);
#10037=VECTOR('',#33389,1.);
#10038=VECTOR('',#33392,1.);
#10039=VECTOR('',#33395,1.);
#10040=VECTOR('',#33406,1.);
#10041=VECTOR('',#33407,1.);
#10042=VECTOR('',#33408,1.);
#10043=VECTOR('',#33409,1.);
#10044=VECTOR('',#33414,1.);
#10045=VECTOR('',#33419,1.);
#10046=VECTOR('',#33420,1.);
#10047=VECTOR('',#33421,1.);
#10048=VECTOR('',#33424,1.);
#10049=VECTOR('',#33425,1.);
#10050=VECTOR('',#33426,1.);
#10051=VECTOR('',#33427,1.);
#10052=VECTOR('',#33432,1.);
#10053=VECTOR('',#33437,1.);
#10054=VECTOR('',#33438,1.);
#10055=VECTOR('',#33439,1.);
#10056=VECTOR('',#33442,1.);
#10057=VECTOR('',#33443,1.);
#10058=VECTOR('',#33444,1.);
#10059=VECTOR('',#33445,1.);
#10060=VECTOR('',#33450,1.);
#10061=VECTOR('',#33455,1.);
#10062=VECTOR('',#33456,1.);
#10063=VECTOR('',#33457,1.);
#10064=VECTOR('',#33460,1.);
#10065=VECTOR('',#33461,1.);
#10066=VECTOR('',#33462,1.);
#10067=VECTOR('',#33463,1.);
#10068=VECTOR('',#33468,1.);
#10069=VECTOR('',#33473,1.);
#10070=VECTOR('',#33474,1.);
#10071=VECTOR('',#33475,1.);
#10072=VECTOR('',#33478,1.);
#10073=VECTOR('',#33479,1.);
#10074=VECTOR('',#33480,1.);
#10075=VECTOR('',#33481,1.);
#10076=VECTOR('',#33486,1.);
#10077=VECTOR('',#33491,1.);
#10078=VECTOR('',#33492,1.);
#10079=VECTOR('',#33493,1.);
#10080=VECTOR('',#33496,1.);
#10081=VECTOR('',#33497,1.);
#10082=VECTOR('',#33498,1.);
#10083=VECTOR('',#33499,1.);
#10084=VECTOR('',#33504,1.);
#10085=VECTOR('',#33509,1.);
#10086=VECTOR('',#33510,1.);
#10087=VECTOR('',#33511,1.);
#10088=VECTOR('',#33514,1.);
#10089=VECTOR('',#33515,1.);
#10090=VECTOR('',#33516,1.);
#10091=VECTOR('',#33517,1.);
#10092=VECTOR('',#33522,1.);
#10093=VECTOR('',#33527,1.);
#10094=VECTOR('',#33528,1.);
#10095=VECTOR('',#33529,1.);
#10096=VECTOR('',#33532,1.);
#10097=VECTOR('',#33533,1.);
#10098=VECTOR('',#33534,1.);
#10099=VECTOR('',#33535,1.);
#10100=VECTOR('',#33540,1.);
#10101=VECTOR('',#33545,1.);
#10102=VECTOR('',#33546,1.);
#10103=VECTOR('',#33547,1.);
#10104=VECTOR('',#33620,1.3);
#10105=VECTOR('',#33629,1.205);
#10106=VECTOR('',#33634,1.205);
#10107=VECTOR('',#33643,2.4);
#10108=VECTOR('',#33648,2.5);
#10109=VECTOR('',#33649,2.5);
#10110=VECTOR('',#33666,1.);
#10111=VECTOR('',#33669,1.);
#10112=VECTOR('',#33674,1.);
#10113=VECTOR('',#33677,1.);
#10114=VECTOR('',#33690,1.);
#10115=VECTOR('',#33691,1.);
#10116=VECTOR('',#33692,1.);
#10117=VECTOR('',#33695,1.);
#10118=VECTOR('',#33696,1.);
#10119=VECTOR('',#33697,1.);
#10120=VECTOR('',#33700,1.);
#10121=VECTOR('',#33705,6.255);
#10122=VECTOR('',#33706,6.255);
#10123=VECTOR('',#33713,1.);
#10124=VECTOR('',#33716,1.);
#10125=VECTOR('',#33721,1.);
#10126=VECTOR('',#33722,1.);
#10127=VECTOR('',#33723,1.);
#10128=VECTOR('',#33724,1.);
#10129=VECTOR('',#33725,1.);
#10130=VECTOR('',#33728,1.);
#10131=VECTOR('',#33729,1.);
#10132=VECTOR('',#33730,1.);
#10133=VECTOR('',#33733,1.);
#10134=VECTOR('',#33734,1.);
#10135=VECTOR('',#33739,1.);
#10136=VECTOR('',#33744,1.);
#10137=VECTOR('',#33747,1.);
#10138=VECTOR('',#33748,1.);
#10139=VECTOR('',#33749,1.);
#10140=VECTOR('',#33752,1.);
#10141=VECTOR('',#33753,1.);
#10142=VECTOR('',#33754,1.);
#10143=VECTOR('',#33755,1.);
#10144=VECTOR('',#33756,1.);
#10145=VECTOR('',#33761,1.);
#10146=VECTOR('',#33774,1.);
#10147=VECTOR('',#33785,1.);
#10148=VECTOR('',#33788,1.);
#10149=VECTOR('',#33793,1.);
#10150=VECTOR('',#33794,1.);
#10151=VECTOR('',#33797,1.);
#10152=VECTOR('',#33802,1.);
#10153=VECTOR('',#33803,1.);
#10154=VECTOR('',#33808,1.);
#10155=VECTOR('',#33821,1.);
#10156=VECTOR('',#33824,1.);
#10157=VECTOR('',#33825,1.);
#10158=VECTOR('',#33830,1.);
#10159=VECTOR('',#33831,1.);
#10160=VECTOR('',#33834,1.);
#10161=VECTOR('',#33839,1.);
#10162=VECTOR('',#33840,1.);
#10163=VECTOR('',#33843,1.);
#10164=VECTOR('',#33846,1.);
#10165=VECTOR('',#33849,1.);
#10166=VECTOR('',#33852,1.);
#10167=VECTOR('',#33865,1.);
#10168=VECTOR('',#33866,1.);
#10169=VECTOR('',#33867,1.);
#10170=VECTOR('',#33868,1.);
#10171=VECTOR('',#33869,1.);
#10172=VECTOR('',#33874,1.);
#10173=VECTOR('',#33877,1.);
#10174=VECTOR('',#33890,1.1);
#10175=VECTOR('',#33911,1.1);
#10176=VECTOR('',#33928,1.1);
#10177=VECTOR('',#33939,1.1);
#10178=VECTOR('',#33960,1.);
#10179=VECTOR('',#33961,1.);
#10180=VECTOR('',#33964,1.);
#10181=VECTOR('',#33965,1.);
#10182=VECTOR('',#33980,1.);
#10183=VECTOR('',#33981,1.);
#10184=VECTOR('',#33986,1.);
#10185=VECTOR('',#33989,1.);
#10186=VECTOR('',#33992,1.);
#10187=VECTOR('',#33993,1.);
#10188=VECTOR('',#33994,1.);
#10189=VECTOR('',#33995,1.);
#10190=VECTOR('',#33996,1.);
#10191=VECTOR('',#33999,1.);
#10192=VECTOR('',#34002,1.);
#10193=VECTOR('',#34005,1.);
#10194=VECTOR('',#34008,1.);
#10195=VECTOR('',#34011,1.);
#10196=VECTOR('',#34020,1.);
#10197=VECTOR('',#34023,1.);
#10198=VECTOR('',#34026,1.);
#10199=VECTOR('',#34029,1.);
#10200=VECTOR('',#34034,1.);
#10201=VECTOR('',#34035,1.);
#10202=VECTOR('',#34036,1.);
#10203=VECTOR('',#34047,1.);
#10204=VECTOR('',#34050,1.);
#10205=VECTOR('',#34053,1.);
#10206=VECTOR('',#34056,1.);
#10207=VECTOR('',#34059,1.);
#10208=VECTOR('',#34062,1.);
#10209=VECTOR('',#34067,1.);
#10210=VECTOR('',#34070,1.);
#10211=VECTOR('',#34073,1.);
#10212=VECTOR('',#34088,1.);
#10213=VECTOR('',#34089,1.);
#10214=VECTOR('',#34090,1.);
#10215=VECTOR('',#34093,1.);
#10216=VECTOR('',#34096,1.);
#10217=VECTOR('',#34099,1.);
#10218=VECTOR('',#34102,1.);
#10219=VECTOR('',#34105,1.);
#10220=VECTOR('',#34108,1.);
#10221=VECTOR('',#34109,1.);
#10222=VECTOR('',#34110,1.);
#10223=VECTOR('',#34125,1.);
#10224=VECTOR('',#34126,1.);
#10225=VECTOR('',#34127,1.);
#10226=VECTOR('',#34128,1.);
#10227=VECTOR('',#34129,1.);
#10228=VECTOR('',#34130,1.);
#10229=VECTOR('',#34131,1.);
#10230=VECTOR('',#34132,1.);
#10231=VECTOR('',#34143,0.804999999999993);
#10232=VECTOR('',#34156,0.804999999999993);
#10233=VECTOR('',#34169,0.804999999999993);
#10234=VECTOR('',#34180,1.);
#10235=VECTOR('',#34183,1.);
#10236=VECTOR('',#34186,1.);
#10237=VECTOR('',#34191,0.804999999999993);
#10238=VECTOR('',#34196,1.);
#10239=VECTOR('',#34201,1.);
#10240=VECTOR('',#34202,1.);
#10241=VECTOR('',#34203,1.);
#10242=VECTOR('',#34204,1.);
#10243=VECTOR('',#34205,1.);
#10244=VECTOR('',#34206,1.);
#10245=VECTOR('',#34207,1.);
#10246=VECTOR('',#34208,1.);
#10247=VECTOR('',#34225,2.);
#10248=VECTOR('',#34238,1.);
#10249=VECTOR('',#34241,1.);
#10250=VECTOR('',#34244,1.);
#10251=VECTOR('',#34245,1.);
#10252=VECTOR('',#34246,1.);
#10253=VECTOR('',#34253,1.);
#10254=VECTOR('',#34256,1.);
#10255=VECTOR('',#34259,1.);
#10256=VECTOR('',#34260,1.);
#10257=VECTOR('',#34273,1.);
#10258=VECTOR('',#34276,1.);
#10259=VECTOR('',#34279,1.);
#10260=VECTOR('',#34290,1.);
#10261=VECTOR('',#34291,1.);
#10262=VECTOR('',#34292,1.);
#10263=VECTOR('',#34293,1.);
#10264=VECTOR('',#34294,1.);
#10265=VECTOR('',#34295,1.);
#10266=VECTOR('',#34296,1.);
#10267=VECTOR('',#34297,1.);
#10268=VECTOR('',#34298,1.);
#10269=VECTOR('',#34299,1.);
#10270=VECTOR('',#34300,1.);
#10271=VECTOR('',#34329,1.);
#10272=VECTOR('',#34332,1.);
#10273=VECTOR('',#34333,1.);
#10274=VECTOR('',#34334,1.);
#10275=VECTOR('',#34339,1.);
#10276=VECTOR('',#34342,1.);
#10277=VECTOR('',#34343,1.);
#10278=VECTOR('',#34344,1.);
#10279=VECTOR('',#34351,1.);
#10280=VECTOR('',#34352,1.);
#10281=VECTOR('',#34353,1.);
#10282=VECTOR('',#34354,1.);
#10283=VECTOR('',#34355,1.);
#10284=VECTOR('',#34356,1.);
#10285=VECTOR('',#34359,1.);
#10286=VECTOR('',#34366,1.);
#10287=VECTOR('',#34377,1.);
#10288=VECTOR('',#34384,1.);
#10289=VECTOR('',#34385,1.);
#10290=VECTOR('',#34386,1.);
#10291=VECTOR('',#34389,1.);
#10292=VECTOR('',#34392,1.);
#10293=VECTOR('',#34395,1.);
#10294=VECTOR('',#34402,1.);
#10295=VECTOR('',#34405,1.);
#10296=VECTOR('',#34408,1.);
#10297=VECTOR('',#34411,1.);
#10298=VECTOR('',#34414,1.);
#10299=VECTOR('',#34419,1.);
#10300=VECTOR('',#34422,1.);
#10301=VECTOR('',#34423,1.);
#10302=VECTOR('',#34424,1.);
#10303=VECTOR('',#34425,1.);
#10304=VECTOR('',#34426,1.);
#10305=VECTOR('',#34429,1.);
#10306=VECTOR('',#34430,1.);
#10307=VECTOR('',#34431,1.);
#10308=VECTOR('',#34432,1.);
#10309=VECTOR('',#34433,1.);
#10310=VECTOR('',#34434,1.);
#10311=VECTOR('',#34435,1.);
#10312=VECTOR('',#34436,1.);
#10313=VECTOR('',#34437,1.);
#10314=VECTOR('',#34438,1.);
#10315=VECTOR('',#34439,1.);
#10316=VECTOR('',#34440,1.);
#10317=VECTOR('',#34441,1.);
#10318=VECTOR('',#34442,1.);
#10319=VECTOR('',#34443,1.);
#10320=VECTOR('',#34452,1.);
#10321=VECTOR('',#34455,1.);
#10322=VECTOR('',#34460,1.);
#10323=VECTOR('',#34467,1.);
#10324=VECTOR('',#34470,1.);
#10325=VECTOR('',#34473,1.);
#10326=VECTOR('',#34476,1.);
#10327=VECTOR('',#34479,1.);
#10328=VECTOR('',#34484,1.);
#10329=VECTOR('',#34487,1.);
#10330=VECTOR('',#34492,1.);
#10331=VECTOR('',#34501,1.);
#10332=VECTOR('',#34508,1.);
#10333=VECTOR('',#34511,1.);
#10334=VECTOR('',#34514,1.);
#10335=VECTOR('',#34519,1.);
#10336=VECTOR('',#34522,1.);
#10337=VECTOR('',#34545,1.);
#10338=VECTOR('',#34546,1.);
#10339=VECTOR('',#34549,1.);
#10340=VECTOR('',#34550,1.);
#10341=VECTOR('',#34561,1.);
#10342=VECTOR('',#34572,1.);
#10343=VECTOR('',#34573,1.);
#10344=VECTOR('',#34576,1.);
#10345=VECTOR('',#34577,1.);
#10346=VECTOR('',#34578,1.);
#10347=VECTOR('',#34589,1.);
#10348=VECTOR('',#34590,1.);
#10349=VECTOR('',#34591,1.);
#10350=VECTOR('',#34592,1.);
#10351=VECTOR('',#34595,1.);
#10352=VECTOR('',#34596,1.);
#10353=VECTOR('',#34601,1.);
#10354=VECTOR('',#34606,1.);
#10355=VECTOR('',#34607,1.);
#10356=VECTOR('',#34608,1.);
#10357=VECTOR('',#34611,1.);
#10358=VECTOR('',#34612,1.);
#10359=VECTOR('',#34613,1.);
#10360=VECTOR('',#34616,1.);
#10361=VECTOR('',#34617,1.);
#10362=VECTOR('',#34618,1.);
#10363=VECTOR('',#34621,1.);
#10364=VECTOR('',#34622,1.);
#10365=VECTOR('',#34623,1.);
#10366=VECTOR('',#34624,1.);
#10367=VECTOR('',#34627,1.);
#10368=VECTOR('',#34628,1.);
#10369=VECTOR('',#34629,1.);
#10370=VECTOR('',#34630,1.);
#10371=VECTOR('',#34645,1.);
#10372=VECTOR('',#34648,1.);
#10373=VECTOR('',#34653,1.);
#10374=VECTOR('',#34656,1.);
#10375=VECTOR('',#34659,1.);
#10376=VECTOR('',#34660,1.);
#10377=VECTOR('',#34663,1.);
#10378=VECTOR('',#34664,1.);
#10379=VECTOR('',#34665,1.);
#10380=VECTOR('',#34678,1.);
#10381=VECTOR('',#34681,1.);
#10382=VECTOR('',#34686,1.);
#10383=VECTOR('',#34689,1.);
#10384=VECTOR('',#34690,1.);
#10385=VECTOR('',#34693,1.);
#10386=VECTOR('',#34694,1.);
#10387=VECTOR('',#34695,1.);
#10388=VECTOR('',#34698,1.);
#10389=VECTOR('',#34699,1.);
#10390=VECTOR('',#34702,1.);
#10391=VECTOR('',#34703,1.);
#10392=VECTOR('',#34704,1.);
#10393=VECTOR('',#34705,1.);
#10394=VECTOR('',#34708,1.);
#10395=VECTOR('',#34709,1.);
#10396=VECTOR('',#34710,1.);
#10397=VECTOR('',#34711,1.);
#10398=VECTOR('',#34714,1.);
#10399=VECTOR('',#34719,1.);
#10400=VECTOR('',#34720,1.);
#10401=VECTOR('',#34721,1.);
#10402=VECTOR('',#34724,1.);
#10403=VECTOR('',#34725,1.);
#10404=VECTOR('',#34728,1.);
#10405=VECTOR('',#34729,1.);
#10406=VECTOR('',#34732,1.);
#10407=VECTOR('',#34733,1.);
#10408=VECTOR('',#34736,1.);
#10409=VECTOR('',#34737,1.);
#10410=VECTOR('',#34740,1.);
#10411=VECTOR('',#34741,1.);
#10412=VECTOR('',#34744,1.);
#10413=VECTOR('',#34745,1.);
#10414=VECTOR('',#34748,1.);
#10415=VECTOR('',#34749,1.);
#10416=VECTOR('',#34752,1.);
#10417=VECTOR('',#34753,1.);
#10418=VECTOR('',#34756,1.);
#10419=VECTOR('',#34759,1.);
#10420=VECTOR('',#34760,1.);
#10421=VECTOR('',#34761,1.);
#10422=VECTOR('',#34762,1.);
#10423=VECTOR('',#34763,1.);
#10424=VECTOR('',#34764,1.);
#10425=VECTOR('',#34765,1.);
#10426=VECTOR('',#34766,1.);
#10427=VECTOR('',#34767,1.);
#10428=VECTOR('',#34768,1.);
#10429=VECTOR('',#34769,1.);
#10430=VECTOR('',#34770,1.);
#10431=VECTOR('',#34771,1.);
#10432=VECTOR('',#34772,1.);
#10433=VECTOR('',#34773,1.);
#10434=VECTOR('',#34774,1.);
#10435=VECTOR('',#34775,1.);
#10436=VECTOR('',#34776,1.);
#10437=VECTOR('',#34781,1.);
#10438=VECTOR('',#34782,1.);
#10439=VECTOR('',#34783,1.);
#10440=VECTOR('',#34786,1.);
#10441=VECTOR('',#34787,1.);
#10442=VECTOR('',#34790,1.);
#10443=VECTOR('',#34791,1.);
#10444=VECTOR('',#34794,1.);
#10445=VECTOR('',#34803,2.25);
#10446=VECTOR('',#34810,2.25);
#10447=VECTOR('',#34813,2.25);
#10448=VECTOR('',#34816,2.25);
#10449=VECTOR('',#34819,1.);
#10450=VECTOR('',#34822,1.);
#10451=VECTOR('',#34829,1.);
#10452=VECTOR('',#34830,1.);
#10453=VECTOR('',#34833,1.);
#10454=VECTOR('',#34836,1.);
#10455=VECTOR('',#34839,1.);
#10456=VECTOR('',#34842,1.);
#10457=VECTOR('',#34843,1.);
#10458=VECTOR('',#34846,1.);
#10459=VECTOR('',#34847,1.);
#10460=VECTOR('',#34856,6.355);
#10461=VECTOR('',#34865,6.355);
#10462=VECTOR('',#34872,10.15);
#10463=VECTOR('',#34877,10.);
#10464=VECTOR('',#34884,9.85);
#10465=VECTOR('',#34887,10.15);
#10466=VECTOR('',#34894,10.);
#10467=VECTOR('',#34897,9.85);
#10468=VECTOR('',#34902,1.);
#10469=VECTOR('',#34905,1.);
#10470=VECTOR('',#34908,1.);
#10471=VECTOR('',#34911,1.);
#10472=VECTOR('',#34918,1.);
#10473=VECTOR('',#34921,1.);
#10474=VECTOR('',#34926,1.);
#10475=VECTOR('',#34939,1.);
#10476=VECTOR('',#34942,1.);
#10477=VECTOR('',#34949,1.);
#10478=VECTOR('',#34952,1.);
#10479=VECTOR('',#34957,1.);
#10480=VECTOR('',#34958,1.);
#10481=VECTOR('',#34959,1.);
#10482=VECTOR('',#34962,1.);
#10483=VECTOR('',#34967,1.);
#10484=VECTOR('',#34968,1.);
#10485=VECTOR('',#34975,1.);
#10486=VECTOR('',#34980,1.);
#10487=VECTOR('',#34981,1.);
#10488=VECTOR('',#34988,1.);
#10489=VECTOR('',#34993,1.);
#10490=VECTOR('',#34994,1.);
#10491=VECTOR('',#34997,1.);
#10492=VECTOR('',#35002,1.);
#10493=VECTOR('',#35003,1.);
#10494=VECTOR('',#35008,1.);
#10495=VECTOR('',#35011,1.);
#10496=VECTOR('',#35016,1.);
#10497=VECTOR('',#35017,1.);
#10498=VECTOR('',#35020,1.);
#10499=VECTOR('',#35025,1.);
#10500=VECTOR('',#35028,1.);
#10501=VECTOR('',#35033,1.);
#10502=VECTOR('',#35036,1.);
#10503=VECTOR('',#35043,0.8);
#10504=VECTOR('',#35048,0.8);
#10505=VECTOR('',#35051,0.8);
#10506=VECTOR('',#35054,0.8);
#10507=VECTOR('',#35057,0.8);
#10508=VECTOR('',#35060,0.8);
#10509=VECTOR('',#35063,0.8);
#10510=VECTOR('',#35066,0.8);
#10511=VECTOR('',#35069,0.8);
#10512=VECTOR('',#35072,0.8);
#10513=VECTOR('',#35075,0.8);
#10514=VECTOR('',#35078,0.8);
#10515=VECTOR('',#35081,0.8);
#10516=VECTOR('',#35084,0.8);
#10517=VECTOR('',#35087,0.8);
#10518=VECTOR('',#35092,0.6767);
#10519=VECTOR('',#35097,0.6767);
#10520=VECTOR('',#35100,0.6767);
#10521=VECTOR('',#35103,0.6767);
#10522=VECTOR('',#35106,0.6767);
#10523=VECTOR('',#35109,0.6767);
#10524=VECTOR('',#35112,0.6767);
#10525=VECTOR('',#35115,0.6767);
#10526=VECTOR('',#35118,0.6767);
#10527=VECTOR('',#35121,0.6767);
#10528=VECTOR('',#35124,0.6767);
#10529=VECTOR('',#35127,0.6767);
#10530=VECTOR('',#35130,0.6767);
#10531=VECTOR('',#35133,0.6767);
#10532=VECTOR('',#35134,1.);
#10533=VECTOR('',#35135,1.);
#10534=VECTOR('',#35136,1.);
#10535=VECTOR('',#35137,1.);
#10536=VECTOR('',#35138,1.);
#10537=VECTOR('',#35139,1.);
#10538=VECTOR('',#35140,1.);
#10539=VECTOR('',#35141,1.);
#10540=VECTOR('',#35142,1.);
#10541=VECTOR('',#35143,1.);
#10542=VECTOR('',#35144,1.);
#10543=VECTOR('',#35145,1.);
#10544=VECTOR('',#35146,1.);
#10545=VECTOR('',#35147,1.);
#10546=VECTOR('',#35148,1.);
#10547=VECTOR('',#35149,1.);
#10548=VECTOR('',#35150,1.);
#10549=VECTOR('',#35151,1.);
#10550=VECTOR('',#35152,1.);
#10551=VECTOR('',#35153,1.);
#10552=VECTOR('',#35154,1.);
#10553=VECTOR('',#35155,1.);
#10554=VECTOR('',#35156,1.);
#10555=VECTOR('',#35157,1.);
#10556=VECTOR('',#35158,1.);
#10557=VECTOR('',#35159,1.);
#10558=VECTOR('',#35160,1.);
#10559=VECTOR('',#35161,1.);
#10560=VECTOR('',#35162,1.);
#10561=VECTOR('',#35163,1.);
#10562=VECTOR('',#35164,1.);
#10563=VECTOR('',#35165,1.);
#10564=VECTOR('',#35166,1.);
#10565=VECTOR('',#35171,1.);
#10566=VECTOR('',#35172,1.);
#10567=VECTOR('',#35173,1.);
#10568=VECTOR('',#35174,1.);
#10569=VECTOR('',#35177,1.);
#10570=VECTOR('',#35178,1.);
#10571=VECTOR('',#35179,1.);
#10572=VECTOR('',#35182,1.);
#10573=VECTOR('',#35183,1.);
#10574=VECTOR('',#35184,1.);
#10575=VECTOR('',#35187,1.);
#10576=VECTOR('',#35188,1.);
#10577=VECTOR('',#35191,1.);
#10578=VECTOR('',#35192,1.);
#10579=VECTOR('',#35193,1.);
#10580=VECTOR('',#35194,1.);
#10581=VECTOR('',#35195,1.);
#10582=VECTOR('',#35196,1.);
#10583=VECTOR('',#35197,1.);
#10584=VECTOR('',#35198,1.);
#10585=VECTOR('',#35199,1.);
#10586=VECTOR('',#35200,1.);
#10587=VECTOR('',#35201,1.);
#10588=VECTOR('',#35202,1.);
#10589=VECTOR('',#35203,1.);
#10590=VECTOR('',#35204,1.);
#10591=VECTOR('',#35205,1.);
#10592=VECTOR('',#35206,1.);
#10593=VECTOR('',#35207,1.);
#10594=VECTOR('',#35208,1.);
#10595=VECTOR('',#35209,1.);
#10596=VECTOR('',#35210,1.);
#10597=VECTOR('',#35211,1.);
#10598=VECTOR('',#35212,1.);
#10599=VECTOR('',#35213,1.);
#10600=VECTOR('',#35214,1.);
#10601=VECTOR('',#35215,1.);
#10602=VECTOR('',#35216,1.);
#10603=VECTOR('',#35217,1.);
#10604=VECTOR('',#35218,1.);
#10605=VECTOR('',#35219,1.);
#10606=VECTOR('',#35220,1.);
#10607=VECTOR('',#35221,1.);
#10608=VECTOR('',#35222,1.);
#10609=VECTOR('',#35223,1.);
#10610=VECTOR('',#35260,1.);
#10611=VECTOR('',#35261,1.);
#10612=VECTOR('',#35262,1.);
#10613=VECTOR('',#35263,1.);
#10614=VECTOR('',#35264,1.);
#10615=VECTOR('',#35265,1.);
#10616=VECTOR('',#35270,1.28782032302755);
#10617=VECTOR('',#35275,1.);
#10618=VECTOR('',#35276,1.);
#10619=VECTOR('',#35279,1.);
#10620=VECTOR('',#35282,1.);
#10621=VECTOR('',#35285,1.);
#10622=VECTOR('',#35288,1.);
#10623=VECTOR('',#35299,0.75);
#10624=CIRCLE('',#27056,6.25);
#10625=CIRCLE('',#27057,6.25);
#10626=CIRCLE('',#27058,6.1);
#10627=CIRCLE('',#27060,6.);
#10628=CIRCLE('',#27061,4.6500000000004);
#10629=CIRCLE('',#27062,6.);
#10630=CIRCLE('',#27063,4.64999999999896);
#10631=CIRCLE('',#27064,6.);
#10632=CIRCLE('',#27065,4.64999999999943);
#10633=CIRCLE('',#27066,6.);
#10634=CIRCLE('',#27067,4.64999999999968);
#10635=CIRCLE('',#27068,6.);
#10636=CIRCLE('',#27069,4.64999999999985);
#10637=CIRCLE('',#27070,6.);
#10638=CIRCLE('',#27071,4.64999999999964);
#10639=CIRCLE('',#27072,6.);
#10640=CIRCLE('',#27073,4.65000000000067);
#10641=CIRCLE('',#27074,6.);
#10642=CIRCLE('',#27075,4.64999999999845);
#10643=CIRCLE('',#27076,6.);
#10644=CIRCLE('',#27077,4.65000000000029);
#10645=CIRCLE('',#27078,6.);
#10646=CIRCLE('',#27079,4.65000000000076);
#10647=CIRCLE('',#27080,6.);
#10648=CIRCLE('',#27081,4.64999999999928);
#10649=CIRCLE('',#27082,6.);
#10650=CIRCLE('',#27083,4.6499999999995);
#10651=CIRCLE('',#27084,6.);
#10652=CIRCLE('',#27085,4.64999999999968);
#10653=CIRCLE('',#27086,6.);
#10654=CIRCLE('',#27087,4.64999999999985);
#10655=CIRCLE('',#27088,6.);
#10656=CIRCLE('',#27089,4.6500000000015);
#10657=CIRCLE('',#27090,6.);
#10658=CIRCLE('',#27091,4.65000000000067);
#10659=CIRCLE('',#27092,6.);
#10660=CIRCLE('',#27093,4.64999999999896);
#10661=CIRCLE('',#27094,6.);
#10662=CIRCLE('',#27095,4.65000000000016);
#10663=CIRCLE('',#27097,6.25);
#10664=CIRCLE('',#27099,6.1);
#10665=CIRCLE('',#27100,6.25);
#10666=CIRCLE('',#27101,6.25);
#10667=CIRCLE('',#27103,4.65000000000016);
#10668=CIRCLE('',#27104,6.);
#10669=CIRCLE('',#27105,4.64999999999896);
#10670=CIRCLE('',#27106,6.);
#10671=CIRCLE('',#27107,4.65000000000067);
#10672=CIRCLE('',#27108,6.);
#10673=CIRCLE('',#27109,4.6500000000015);
#10674=CIRCLE('',#27110,6.);
#10675=CIRCLE('',#27111,4.64999999999985);
#10676=CIRCLE('',#27112,6.);
#10677=CIRCLE('',#27113,4.64999999999968);
#10678=CIRCLE('',#27114,6.);
#10679=CIRCLE('',#27115,4.6499999999995);
#10680=CIRCLE('',#27116,6.);
#10681=CIRCLE('',#27117,4.64999999999928);
#10682=CIRCLE('',#27118,6.);
#10683=CIRCLE('',#27119,4.65000000000076);
#10684=CIRCLE('',#27120,6.);
#10685=CIRCLE('',#27121,4.65000000000029);
#10686=CIRCLE('',#27122,6.);
#10687=CIRCLE('',#27123,4.64999999999845);
#10688=CIRCLE('',#27124,6.);
#10689=CIRCLE('',#27125,4.65000000000067);
#10690=CIRCLE('',#27126,6.);
#10691=CIRCLE('',#27127,4.64999999999964);
#10692=CIRCLE('',#27128,6.);
#10693=CIRCLE('',#27129,4.64999999999985);
#10694=CIRCLE('',#27130,6.);
#10695=CIRCLE('',#27131,4.64999999999968);
#10696=CIRCLE('',#27132,6.);
#10697=CIRCLE('',#27133,4.64999999999943);
#10698=CIRCLE('',#27134,6.);
#10699=CIRCLE('',#27135,4.64999999999896);
#10700=CIRCLE('',#27136,6.);
#10701=CIRCLE('',#27137,4.6500000000004);
#10702=CIRCLE('',#27138,6.);
#10703=CIRCLE('',#27140,6.25);
#10704=CIRCLE('',#27142,2.9);
#10705=CIRCLE('',#27144,3.);
#10706=CIRCLE('',#27146,3.);
#10707=CIRCLE('',#27148,6.1);
#10708=CIRCLE('',#27151,6.1);
#10709=CIRCLE('',#27153,3.);
#10710=CIRCLE('',#27155,3.);
#10711=CIRCLE('',#27157,2.9);
#10712=CIRCLE('',#27233,1.188225);
#10713=CIRCLE('',#27247,1.016475);
#10714=CIRCLE('',#27249,1.016475);
#10715=CIRCLE('',#27262,1.188225);
#10716=CIRCLE('',#27263,1.188225);
#10717=CIRCLE('',#27265,1.188225);
#10718=CIRCLE('',#27266,1.188225);
#10719=CIRCLE('',#27267,1.016475);
#10720=CIRCLE('',#27270,1.188225);
#10721=CIRCLE('',#27272,1.7);
#10722=CIRCLE('',#27274,2.);
#10723=CIRCLE('',#27276,2.);
#10724=CIRCLE('',#27278,1.25);
#10725=CIRCLE('',#27281,1.05);
#10726=CIRCLE('',#27286,15.75);
#10727=CIRCLE('',#27287,15.75);
#10728=CIRCLE('',#27289,15.6207106781187);
#10729=CIRCLE('',#27296,1.4);
#10730=CIRCLE('',#27297,1.25);
#10731=CIRCLE('',#27300,15.55);
#10732=CIRCLE('',#27301,2.9);
#10733=CIRCLE('',#27302,15.55);
#10734=CIRCLE('',#27303,3.65);
#10735=CIRCLE('',#27304,15.55);
#10736=CIRCLE('',#27305,2.15);
#10737=CIRCLE('',#27306,15.55);
#10738=CIRCLE('',#27307,2.155);
#10739=CIRCLE('',#27316,2.75);
#10740=CIRCLE('',#27318,15.75);
#10741=CIRCLE('',#27320,2.75);
#10742=CIRCLE('',#27323,2.005);
#10743=CIRCLE('',#27325,2.005);
#10744=CIRCLE('',#27332,15.75);
#10745=CIRCLE('',#27333,15.75);
#10746=CIRCLE('',#27337,2.);
#10747=CIRCLE('',#27339,2.);
#10748=CIRCLE('',#27347,15.75);
#10749=CIRCLE('',#27350,3.5);
#10750=CIRCLE('',#27352,3.5);
#10751=CIRCLE('',#27355,15.45);
#10752=CIRCLE('',#27356,15.6207106781187);
#10753=CIRCLE('',#27358,15.6207106781187);
#10754=CIRCLE('',#27359,15.45);
#10755=CIRCLE('',#27361,15.45);
#10756=CIRCLE('',#27363,15.6207106781187);
#10757=CIRCLE('',#27364,15.45);
#10758=CIRCLE('',#27366,2.85);
#10759=CIRCLE('',#27369,3.6);
#10760=CIRCLE('',#27372,1.35);
#10761=CIRCLE('',#27373,1.25);
#10762=CIRCLE('',#27375,2.1);
#10763=CIRCLE('',#27380,2.105);
#10764=CIRCLE('',#27385,15.75);
#10765=CIRCLE('',#27387,15.75);
#10766=CIRCLE('',#27391,1.85);
#10767=CIRCLE('',#27393,2.);
#10768=CIRCLE('',#27395,2.);
#10769=CIRCLE('',#27397,1.85);
#10770=CIRCLE('',#27402,7.5);
#10771=CIRCLE('',#27403,7.5);
#10772=CIRCLE('',#27405,3.0025);
#10773=CIRCLE('',#27406,3.0025);
#10774=CIRCLE('',#27408,1.8);
#10775=CIRCLE('',#27409,19.2);
#10776=CIRCLE('',#27410,19.2);
#10777=CIRCLE('',#27411,19.2);
#10778=CIRCLE('',#27412,19.2);
#10779=CIRCLE('',#27413,19.2);
#10780=CIRCLE('',#27414,19.2);
#10781=CIRCLE('',#27415,19.2);
#10782=CIRCLE('',#27423,3.1025);
#10783=CIRCLE('',#27425,7.3);
#10784=CIRCLE('',#27428,7.3);
#10785=CIRCLE('',#27430,3.1025);
#10786=CIRCLE('',#27434,0.989525);
#10787=CIRCLE('',#27442,0.8469);
#10788=CIRCLE('',#27444,0.8469);
#10789=CIRCLE('',#27451,0.989525);
#10790=CIRCLE('',#27452,0.989525);
#10791=CIRCLE('',#27454,0.989525);
#10792=CIRCLE('',#27455,0.989525);
#10793=CIRCLE('',#27456,0.8469);
#10794=CIRCLE('',#27459,0.577350269189626);
#10795=CIRCLE('',#27461,0.577350269189626);
#10796=CIRCLE('',#27463,0.577350269189626);
#10797=CIRCLE('',#27465,0.577350269189626);
#10798=CIRCLE('',#27467,0.577350269189626);
#10799=CIRCLE('',#27469,0.577350269189626);
#10800=CIRCLE('',#27471,0.575688399926292);
#10801=CIRCLE('',#27472,0.575688399926292);
#10802=CIRCLE('',#27473,0.575688399926292);
#10803=CIRCLE('',#27474,0.575688399926292);
#10804=CIRCLE('',#27475,0.575688399926292);
#10805=CIRCLE('',#27476,0.575688399926292);
#10806=CIRCLE('',#27477,0.575688399926292);
#10807=CIRCLE('',#27503,0.75);
#10808=CIRCLE('',#27506,0.989525);
#10809=CIRCLE('',#27508,0.92);
#10810=CIRCLE('',#27549,0.7911);
#10811=CIRCLE('',#27579,0.6767);
#10812=CIRCLE('',#27581,0.6767);
#10813=CIRCLE('',#27610,0.7911);
#10814=CIRCLE('',#27611,0.7911);
#10815=CIRCLE('',#27613,0.7911);
#10816=CIRCLE('',#27614,0.7911);
#10817=CIRCLE('',#27615,0.6767);
#10818=CIRCLE('',#27618,0.461880215351701);
#10819=CIRCLE('',#27620,0.461880215351701);
#10820=CIRCLE('',#27622,0.461880215351701);
#10821=CIRCLE('',#27624,0.461880215351701);
#10822=CIRCLE('',#27626,0.461880215351701);
#10823=CIRCLE('',#27628,0.461880215351701);
#10824=CIRCLE('',#27630,0.460219541126976);
#10825=CIRCLE('',#27631,0.460219541126976);
#10826=CIRCLE('',#27632,0.460219541126976);
#10827=CIRCLE('',#27633,0.460219541126976);
#10828=CIRCLE('',#27634,0.460219541126976);
#10829=CIRCLE('',#27635,0.460219541126976);
#10830=CIRCLE('',#27636,0.460219541126976);
#10831=CIRCLE('',#27662,0.6);
#10832=CIRCLE('',#27665,0.7911);
#10833=CIRCLE('',#27667,0.72);
#10834=CIRCLE('',#27671,0.805);
#10835=CIRCLE('',#27672,0.885);
#10836=CIRCLE('',#27674,0.805);
#10837=CIRCLE('',#27676,1.14);
#10838=CIRCLE('',#27678,0.885);
#10839=CIRCLE('',#27680,1.14);
#10840=CIRCLE('',#27691,0.7911);
#10841=CIRCLE('',#27711,0.6767);
#10842=CIRCLE('',#27713,0.6767);
#10843=CIRCLE('',#27732,0.7911);
#10844=CIRCLE('',#27733,0.7911);
#10845=CIRCLE('',#27735,0.7911);
#10846=CIRCLE('',#27736,0.7911);
#10847=CIRCLE('',#27737,0.6767);
#10848=CIRCLE('',#27740,0.461880215351701);
#10849=CIRCLE('',#27742,0.461880215351701);
#10850=CIRCLE('',#27744,0.461880215351701);
#10851=CIRCLE('',#27746,0.461880215351701);
#10852=CIRCLE('',#27748,0.461880215351701);
#10853=CIRCLE('',#27750,0.461880215351701);
#10854=CIRCLE('',#27752,0.460219541126976);
#10855=CIRCLE('',#27753,0.460219541126976);
#10856=CIRCLE('',#27754,0.460219541126976);
#10857=CIRCLE('',#27755,0.460219541126976);
#10858=CIRCLE('',#27756,0.460219541126976);
#10859=CIRCLE('',#27757,0.460219541126976);
#10860=CIRCLE('',#27758,0.460219541126976);
#10861=CIRCLE('',#27784,0.6);
#10862=CIRCLE('',#27787,0.7911);
#10863=CIRCLE('',#27789,0.72);
#10864=CIRCLE('',#27793,7.5);
#10865=CIRCLE('',#27794,7.5);
#10866=CIRCLE('',#27797,1.155);
#10867=CIRCLE('',#27798,1.005);
#10868=CIRCLE('',#27800,1.005);
#10869=CIRCLE('',#27801,1.005);
#10870=CIRCLE('',#27802,1.005);
#10871=CIRCLE('',#27804,7.3);
#10872=CIRCLE('',#27807,3.0025);
#10873=CIRCLE('',#27808,3.0025);
#10874=CIRCLE('',#27813,3.1025);
#10875=CIRCLE('',#27815,7.3);
#10876=CIRCLE('',#27911,1.905);
#10877=CIRCLE('',#28167,0.905000000000001);
#10878=CIRCLE('',#28279,0.805);
#10879=CIRCLE('',#28281,1.755);
#10880=CIRCLE('',#28282,1.755);
#10881=CIRCLE('',#28308,0.25);
#10882=CIRCLE('',#28309,0.25);
#10883=CIRCLE('',#28313,0.25);
#10884=CIRCLE('',#28314,0.25);
#10885=CIRCLE('',#28318,0.25);
#10886=CIRCLE('',#28319,0.25);
#10887=CIRCLE('',#28323,0.25);
#10888=CIRCLE('',#28324,0.25);
#10889=CIRCLE('',#28328,0.25);
#10890=CIRCLE('',#28329,0.25);
#10891=CIRCLE('',#28333,0.25);
#10892=CIRCLE('',#28334,0.25);
#10893=CIRCLE('',#28338,0.25);
#10894=CIRCLE('',#28339,0.25);
#10895=CIRCLE('',#28343,0.25);
#10896=CIRCLE('',#28344,0.25);
#10897=CIRCLE('',#28347,2.5);
#10898=CIRCLE('',#28349,2.5);
#10899=CIRCLE('',#28351,2.5);
#10900=CIRCLE('',#28352,2.5);
#10901=CIRCLE('',#28354,2.5);
#10902=CIRCLE('',#28355,2.5);
#10903=CIRCLE('',#28357,2.5);
#10904=CIRCLE('',#28359,2.5);
#10905=CIRCLE('',#28361,2.5);
#10906=CIRCLE('',#28363,2.5);
#10907=CIRCLE('',#28365,2.5);
#10908=CIRCLE('',#28367,2.5);
#10909=CIRCLE('',#28369,2.5);
#10910=CIRCLE('',#28371,2.5);
#10911=CIRCLE('',#28373,2.5);
#10912=CIRCLE('',#28375,2.5);
#10913=CIRCLE('',#28377,2.5);
#10914=CIRCLE('',#28379,2.5);
#10915=CIRCLE('',#28381,1.3);
#10916=CIRCLE('',#28382,1.3);
#10917=CIRCLE('',#28384,1.205);
#10918=CIRCLE('',#28386,1.205);
#10919=CIRCLE('',#28389,2.3);
#10920=CIRCLE('',#28391,2.5);
#10921=CIRCLE('',#28393,2.5);
#10922=CIRCLE('',#28395,4.5);
#10923=CIRCLE('',#28398,6.255);
#10924=CIRCLE('',#28399,6.255);
#10925=CIRCLE('',#28400,6.555);
#10926=CIRCLE('',#28402,0.3);
#10927=CIRCLE('',#28403,0.3);
#10928=CIRCLE('',#28405,0.3);
#10929=CIRCLE('',#28406,0.3);
#10930=CIRCLE('',#28408,6.255);
#10931=CIRCLE('',#28409,6.255);
#10932=CIRCLE('',#28410,6.555);
#10933=CIRCLE('',#28413,0.3);
#10934=CIRCLE('',#28415,6.255);
#10935=CIRCLE('',#28416,6.255);
#10936=CIRCLE('',#28432,0.300000000000001);
#10937=CIRCLE('',#28434,0.3);
#10938=CIRCLE('',#28435,0.3);
#10939=CIRCLE('',#28436,0.3);
#10940=CIRCLE('',#28440,0.300000000000001);
#10941=CIRCLE('',#28441,0.299999999999999);
#10942=CIRCLE('',#28451,0.3);
#10943=CIRCLE('',#28453,0.3);
#10944=CIRCLE('',#28454,4.);
#10945=CIRCLE('',#28455,4.3);
#10946=CIRCLE('',#28464,1.3);
#10947=CIRCLE('',#28465,1.3);
#10948=CIRCLE('',#28466,1.3);
#10949=CIRCLE('',#28467,1.3);
#10950=CIRCLE('',#28468,1.4);
#10951=CIRCLE('',#28469,1.4);
#10952=CIRCLE('',#28470,1.4);
#10953=CIRCLE('',#28471,1.4);
#10954=CIRCLE('',#28473,2.3);
#10955=CIRCLE('',#28477,1.1);
#10956=CIRCLE('',#28478,0.3);
#10957=CIRCLE('',#28479,1.4);
#10958=CIRCLE('',#28481,1.1);
#10959=CIRCLE('',#28483,2.25);
#10960=CIRCLE('',#28485,0.3);
#10961=CIRCLE('',#28487,1.1);
#10962=CIRCLE('',#28488,0.3);
#10963=CIRCLE('',#28489,1.4);
#10964=CIRCLE('',#28491,1.1);
#10965=CIRCLE('',#28493,2.25);
#10966=CIRCLE('',#28495,0.3);
#10967=CIRCLE('',#28497,0.3);
#10968=CIRCLE('',#28498,1.1);
#10969=CIRCLE('',#28500,1.1);
#10970=CIRCLE('',#28502,0.3);
#10971=CIRCLE('',#28503,1.1);
#10972=CIRCLE('',#28505,1.1);
#10973=CIRCLE('',#28507,0.300000000000001);
#10974=CIRCLE('',#28508,0.300000000000004);
#10975=CIRCLE('',#28509,0.300000000000001);
#10976=CIRCLE('',#28511,0.299999999999998);
#10977=CIRCLE('',#28512,0.299999999999997);
#10978=CIRCLE('',#28513,0.300000000000001);
#10979=CIRCLE('',#28517,30.6296013460341);
#10980=CIRCLE('',#28518,30.9296013460341);
#10981=CIRCLE('',#28520,30.9296013460341);
#10982=CIRCLE('',#28521,30.6296013460341);
#10983=CIRCLE('',#28524,8.);
#10984=CIRCLE('',#28525,7.99950242947666);
#10985=CIRCLE('',#28528,0.299999999999997);
#10986=CIRCLE('',#28530,0.3);
#10987=CIRCLE('',#28531,0.299999999999998);
#10988=CIRCLE('',#28533,0.3);
#10989=CIRCLE('',#28535,31.5);
#10990=CIRCLE('',#28536,31.5);
#10991=CIRCLE('',#28537,31.5);
#10992=CIRCLE('',#28538,31.5);
#10993=CIRCLE('',#28540,32.7);
#10994=CIRCLE('',#28542,33.);
#10995=CIRCLE('',#28543,0.299999999999997);
#10996=CIRCLE('',#28545,33.);
#10997=CIRCLE('',#28546,33.);
#10998=CIRCLE('',#28547,33.);
#10999=CIRCLE('',#28548,33.);
#11000=CIRCLE('',#28549,33.);
#11001=CIRCLE('',#28551,0.299999999999997);
#11002=CIRCLE('',#28552,0.3);
#11003=CIRCLE('',#28554,0.300000000000002);
#11004=CIRCLE('',#28556,0.3);
#11005=CIRCLE('',#28558,32.7);
#11006=CIRCLE('',#28559,0.299999999999997);
#11007=CIRCLE('',#28561,31.5);
#11008=CIRCLE('',#28563,31.5);
#11009=CIRCLE('',#28564,31.5);
#11010=CIRCLE('',#28565,31.5);
#11011=CIRCLE('',#28569,1.10499999999999);
#11012=CIRCLE('',#28570,0.3);
#11013=CIRCLE('',#28571,0.804999999999993);
#11014=CIRCLE('',#28572,0.804999999999993);
#11015=CIRCLE('',#28574,1.10499999999999);
#11016=CIRCLE('',#28575,1.10499999999999);
#11017=CIRCLE('',#28576,1.10499999999999);
#11018=CIRCLE('',#28577,1.10499999999999);
#11019=CIRCLE('',#28579,0.804999999999993);
#11020=CIRCLE('',#28581,0.3);
#11021=CIRCLE('',#28582,0.804999999999993);
#11022=CIRCLE('',#28583,0.804999999999993);
#11023=CIRCLE('',#28585,0.804999999999993);
#11024=CIRCLE('',#28587,0.3);
#11025=CIRCLE('',#28588,0.804999999999993);
#11026=CIRCLE('',#28589,0.804999999999993);
#11027=CIRCLE('',#28591,0.804999999999993);
#11028=CIRCLE('',#28593,0.3);
#11029=CIRCLE('',#28594,0.804999999999993);
#11030=CIRCLE('',#28595,0.804999999999993);
#11031=CIRCLE('',#28600,0.804999999999993);
#11032=CIRCLE('',#28602,0.3);
#11033=CIRCLE('',#28603,0.3);
#11034=CIRCLE('',#28605,1.10499999999999);
#11035=CIRCLE('',#28606,1.10499999999999);
#11036=CIRCLE('',#28607,1.10499999999999);
#11037=CIRCLE('',#28608,1.10499999999999);
#11038=CIRCLE('',#28610,0.3);
#11039=CIRCLE('',#28611,2.);
#11040=CIRCLE('',#28613,2.);
#11041=CIRCLE('',#28614,2.);
#11042=CIRCLE('',#28616,30.9296013460341);
#11043=CIRCLE('',#28617,30.6296013460341);
#11044=CIRCLE('',#28619,30.6296013460341);
#11045=CIRCLE('',#28622,30.9296013460341);
#11046=CIRCLE('',#28624,7.99950242947665);
#11047=CIRCLE('',#28627,2.3);
#11048=CIRCLE('',#28628,0.3);
#11049=CIRCLE('',#28630,4.);
#11050=CIRCLE('',#28631,1.2);
#11051=CIRCLE('',#28632,1.2);
#11052=CIRCLE('',#28633,1.2);
#11053=CIRCLE('',#28634,1.2);
#11054=CIRCLE('',#28635,2.25);
#11055=CIRCLE('',#28636,2.25);
#11056=CIRCLE('',#28637,2.25);
#11057=CIRCLE('',#28638,2.25);
#11058=CIRCLE('',#28640,0.3);
#11059=CIRCLE('',#28644,0.3);
#11060=CIRCLE('',#28646,0.3);
#11061=CIRCLE('',#28648,0.3);
#11062=CIRCLE('',#28650,0.3);
#11063=CIRCLE('',#28655,0.3);
#11064=CIRCLE('',#28658,2.8);
#11065=CIRCLE('',#28662,32.7);
#11066=CIRCLE('',#28664,4.00009261333671);
#11067=CIRCLE('',#28666,32.7);
#11068=CIRCLE('',#28668,4.00009261333671);
#11069=CIRCLE('',#28670,0.3);
#11070=CIRCLE('',#28675,3.70000000000001);
#11071=CIRCLE('',#28677,3.70000000000001);
#11072=CIRCLE('',#28679,3.70000000000002);
#11073=CIRCLE('',#28680,8.3);
#11074=CIRCLE('',#28681,8.3);
#11075=CIRCLE('',#28682,2.8);
#11076=CIRCLE('',#28683,11.7);
#11077=CIRCLE('',#28684,5.29999999999999);
#11078=CIRCLE('',#28685,10.3);
#11079=CIRCLE('',#28687,4.00009261333671);
#11080=CIRCLE('',#28692,12.);
#11081=CIRCLE('',#28693,12.);
#11082=CIRCLE('',#28695,11.7);
#11083=CIRCLE('',#28697,8.3);
#11084=CIRCLE('',#28698,8.3);
#11085=CIRCLE('',#28699,3.70000000000002);
#11086=CIRCLE('',#28700,3.70000000000001);
#11087=CIRCLE('',#28701,3.70000000000001);
#11088=CIRCLE('',#28702,5.29999999999999);
#11089=CIRCLE('',#28703,10.3);
#11090=CIRCLE('',#28706,4.00009261333671);
#11091=CIRCLE('',#28713,2.825);
#11092=CIRCLE('',#28714,2.5);
#11093=CIRCLE('',#28716,2.5);
#11094=CIRCLE('',#28717,2.825);
#11095=CIRCLE('',#28719,8.);
#11096=CIRCLE('',#28721,8.);
#11097=CIRCLE('',#28725,8.);
#11098=CIRCLE('',#28742,7.99950242947665);
#11099=CIRCLE('',#28747,12.);
#11100=CIRCLE('',#28748,12.);
#11101=CIRCLE('',#28755,4.00009261333671);
#11102=CIRCLE('',#28757,5.00011576667089);
#11103=CIRCLE('',#28759,4.00009261333671);
#11104=CIRCLE('',#28761,5.00011576667089);
#11105=CIRCLE('',#28771,7.99950242947666);
#11106=CIRCLE('',#28801,2.25);
#11107=CIRCLE('',#28804,2.25);
#11108=CIRCLE('',#28821,6.455);
#11109=CIRCLE('',#28823,9.7);
#11110=CIRCLE('',#28825,6.455);
#11111=CIRCLE('',#28827,9.7);
#11112=CIRCLE('',#28829,10.);
#11113=CIRCLE('',#28831,10.);
#11114=CIRCLE('',#28835,10.);
#11115=CIRCLE('',#28837,10.);
#11116=CIRCLE('',#28844,5.);
#11117=CIRCLE('',#28852,5.);
#11118=CIRCLE('',#28864,1.5);
#11119=CIRCLE('',#28867,1.5);
#11120=CIRCLE('',#28869,1.5);
#11121=CIRCLE('',#28872,1.5);
#11122=CIRCLE('',#28874,1.5);
#11123=CIRCLE('',#28877,1.5);
#11124=CIRCLE('',#28882,1.5);
#11125=CIRCLE('',#28885,1.5);
#11126=CIRCLE('',#28894,0.7911);
#11127=CIRCLE('',#28909,0.7911);
#11128=CIRCLE('',#28911,0.6767);
#11129=CIRCLE('',#28937,0.7911);
#11130=CIRCLE('',#28938,0.7911);
#11131=CIRCLE('',#28940,0.7911);
#11132=CIRCLE('',#28941,0.7911);
#11133=CIRCLE('',#28942,0.6767);
#11134=CIRCLE('',#28945,0.8511);
#11135=CIRCLE('',#28946,0.06);
#11136=CIRCLE('',#28947,0.7911);
#11137=CIRCLE('',#28951,1.14);
#11138=CIRCLE('',#28960,0.7);
#11139=VERTEX_POINT('',#35349);
#11140=VERTEX_POINT('',#35350);
#11141=VERTEX_POINT('',#35353);
#11142=VERTEX_POINT('',#35357);
#11143=VERTEX_POINT('',#35358);
#11144=VERTEX_POINT('',#35367);
#11145=VERTEX_POINT('',#35369);
#11146=VERTEX_POINT('',#35416);
#11147=VERTEX_POINT('',#35418);
#11148=VERTEX_POINT('',#35420);
#11149=VERTEX_POINT('',#35422);
#11150=VERTEX_POINT('',#35431);
#11151=VERTEX_POINT('',#35433);
#11152=VERTEX_POINT('',#35480);
#11153=VERTEX_POINT('',#35482);
#11154=VERTEX_POINT('',#35484);
#11155=VERTEX_POINT('',#35486);
#11156=VERTEX_POINT('',#35495);
#11157=VERTEX_POINT('',#35497);
#11158=VERTEX_POINT('',#35506);
#11159=VERTEX_POINT('',#35508);
#11160=VERTEX_POINT('',#35510);
#11161=VERTEX_POINT('',#35512);
#11162=VERTEX_POINT('',#35521);
#11163=VERTEX_POINT('',#35523);
#11164=VERTEX_POINT('',#35532);
#11165=VERTEX_POINT('',#35534);
#11166=VERTEX_POINT('',#35536);
#11167=VERTEX_POINT('',#35538);
#11168=VERTEX_POINT('',#35547);
#11169=VERTEX_POINT('',#35549);
#11170=VERTEX_POINT('',#35596);
#11171=VERTEX_POINT('',#35598);
#11172=VERTEX_POINT('',#35600);
#11173=VERTEX_POINT('',#35602);
#11174=VERTEX_POINT('',#35611);
#11175=VERTEX_POINT('',#35613);
#11176=VERTEX_POINT('',#35660);
#11177=VERTEX_POINT('',#35662);
#11178=VERTEX_POINT('',#35664);
#11179=VERTEX_POINT('',#35666);
#11180=VERTEX_POINT('',#35675);
#11181=VERTEX_POINT('',#35677);
#11182=VERTEX_POINT('',#35724);
#11183=VERTEX_POINT('',#35726);
#11184=VERTEX_POINT('',#35728);
#11185=VERTEX_POINT('',#35730);
#11186=VERTEX_POINT('',#35739);
#11187=VERTEX_POINT('',#35741);
#11188=VERTEX_POINT('',#35788);
#11189=VERTEX_POINT('',#35790);
#11190=VERTEX_POINT('',#35792);
#11191=VERTEX_POINT('',#35794);
#11192=VERTEX_POINT('',#35803);
#11193=VERTEX_POINT('',#35805);
#11194=VERTEX_POINT('',#35852);
#11195=VERTEX_POINT('',#35854);
#11196=VERTEX_POINT('',#35856);
#11197=VERTEX_POINT('',#35858);
#11198=VERTEX_POINT('',#35867);
#11199=VERTEX_POINT('',#35869);
#11200=VERTEX_POINT('',#35876);
#11201=VERTEX_POINT('',#35878);
#11202=VERTEX_POINT('',#35880);
#11203=VERTEX_POINT('',#35882);
#11204=VERTEX_POINT('',#35891);
#11205=VERTEX_POINT('',#35893);
#11206=VERTEX_POINT('',#35902);
#11207=VERTEX_POINT('',#35904);
#11208=VERTEX_POINT('',#35906);
#11209=VERTEX_POINT('',#35908);
#11210=VERTEX_POINT('',#35917);
#11211=VERTEX_POINT('',#35919);
#11212=VERTEX_POINT('',#35966);
#11213=VERTEX_POINT('',#35968);
#11214=VERTEX_POINT('',#35970);
#11215=VERTEX_POINT('',#35972);
#11216=VERTEX_POINT('',#35981);
#11217=VERTEX_POINT('',#35983);
#11218=VERTEX_POINT('',#36030);
#11219=VERTEX_POINT('',#36032);
#11220=VERTEX_POINT('',#36034);
#11221=VERTEX_POINT('',#36036);
#11222=VERTEX_POINT('',#36045);
#11223=VERTEX_POINT('',#36047);
#11224=VERTEX_POINT('',#36094);
#11225=VERTEX_POINT('',#36096);
#11226=VERTEX_POINT('',#36098);
#11227=VERTEX_POINT('',#36100);
#11228=VERTEX_POINT('',#36109);
#11229=VERTEX_POINT('',#36111);
#11230=VERTEX_POINT('',#36158);
#11231=VERTEX_POINT('',#36160);
#11232=VERTEX_POINT('',#36162);
#11233=VERTEX_POINT('',#36164);
#11234=VERTEX_POINT('',#36173);
#11235=VERTEX_POINT('',#36175);
#11236=VERTEX_POINT('',#36222);
#11237=VERTEX_POINT('',#36224);
#11238=VERTEX_POINT('',#36226);
#11239=VERTEX_POINT('',#36228);
#11240=VERTEX_POINT('',#36237);
#11241=VERTEX_POINT('',#36239);
#11242=VERTEX_POINT('',#36286);
#11243=VERTEX_POINT('',#36288);
#11244=VERTEX_POINT('',#36290);
#11245=VERTEX_POINT('',#36292);
#11246=VERTEX_POINT('',#36301);
#11247=VERTEX_POINT('',#36303);
#11248=VERTEX_POINT('',#36350);
#11249=VERTEX_POINT('',#36352);
#11250=VERTEX_POINT('',#36356);
#11251=VERTEX_POINT('',#36360);
#11252=VERTEX_POINT('',#36362);
#11253=VERTEX_POINT('',#36364);
#11254=VERTEX_POINT('',#36368);
#11255=VERTEX_POINT('',#36369);
#11256=VERTEX_POINT('',#36416);
#11257=VERTEX_POINT('',#36418);
#11258=VERTEX_POINT('',#36420);
#11259=VERTEX_POINT('',#36422);
#11260=VERTEX_POINT('',#36431);
#11261=VERTEX_POINT('',#36433);
#11262=VERTEX_POINT('',#36480);
#11263=VERTEX_POINT('',#36482);
#11264=VERTEX_POINT('',#36484);
#11265=VERTEX_POINT('',#36486);
#11266=VERTEX_POINT('',#36495);
#11267=VERTEX_POINT('',#36497);
#11268=VERTEX_POINT('',#36544);
#11269=VERTEX_POINT('',#36546);
#11270=VERTEX_POINT('',#36548);
#11271=VERTEX_POINT('',#36550);
#11272=VERTEX_POINT('',#36559);
#11273=VERTEX_POINT('',#36561);
#11274=VERTEX_POINT('',#36608);
#11275=VERTEX_POINT('',#36610);
#11276=VERTEX_POINT('',#36612);
#11277=VERTEX_POINT('',#36614);
#11278=VERTEX_POINT('',#36623);
#11279=VERTEX_POINT('',#36625);
#11280=VERTEX_POINT('',#36634);
#11281=VERTEX_POINT('',#36636);
#11282=VERTEX_POINT('',#36638);
#11283=VERTEX_POINT('',#36640);
#11284=VERTEX_POINT('',#36649);
#11285=VERTEX_POINT('',#36651);
#11286=VERTEX_POINT('',#36698);
#11287=VERTEX_POINT('',#36700);
#11288=VERTEX_POINT('',#36702);
#11289=VERTEX_POINT('',#36704);
#11290=VERTEX_POINT('',#36713);
#11291=VERTEX_POINT('',#36715);
#11292=VERTEX_POINT('',#36762);
#11293=VERTEX_POINT('',#36764);
#11294=VERTEX_POINT('',#36766);
#11295=VERTEX_POINT('',#36768);
#11296=VERTEX_POINT('',#36777);
#11297=VERTEX_POINT('',#36779);
#11298=VERTEX_POINT('',#36826);
#11299=VERTEX_POINT('',#36828);
#11300=VERTEX_POINT('',#36830);
#11301=VERTEX_POINT('',#36832);
#11302=VERTEX_POINT('',#36841);
#11303=VERTEX_POINT('',#36843);
#11304=VERTEX_POINT('',#36890);
#11305=VERTEX_POINT('',#36892);
#11306=VERTEX_POINT('',#36894);
#11307=VERTEX_POINT('',#36896);
#11308=VERTEX_POINT('',#36905);
#11309=VERTEX_POINT('',#36907);
#11310=VERTEX_POINT('',#36954);
#11311=VERTEX_POINT('',#36956);
#11312=VERTEX_POINT('',#36958);
#11313=VERTEX_POINT('',#36960);
#11314=VERTEX_POINT('',#36969);
#11315=VERTEX_POINT('',#36971);
#11316=VERTEX_POINT('',#36980);
#11317=VERTEX_POINT('',#36982);
#11318=VERTEX_POINT('',#36984);
#11319=VERTEX_POINT('',#36986);
#11320=VERTEX_POINT('',#36995);
#11321=VERTEX_POINT('',#36997);
#11322=VERTEX_POINT('',#37044);
#11323=VERTEX_POINT('',#37046);
#11324=VERTEX_POINT('',#37048);
#11325=VERTEX_POINT('',#37050);
#11326=VERTEX_POINT('',#37059);
#11327=VERTEX_POINT('',#37061);
#11328=VERTEX_POINT('',#37108);
#11329=VERTEX_POINT('',#37110);
#11330=VERTEX_POINT('',#37112);
#11331=VERTEX_POINT('',#37114);
#11332=VERTEX_POINT('',#37123);
#11333=VERTEX_POINT('',#37125);
#11334=VERTEX_POINT('',#37172);
#11335=VERTEX_POINT('',#37174);
#11336=VERTEX_POINT('',#37176);
#11337=VERTEX_POINT('',#37178);
#11338=VERTEX_POINT('',#37187);
#11339=VERTEX_POINT('',#37189);
#11340=VERTEX_POINT('',#37198);
#11341=VERTEX_POINT('',#37200);
#11342=VERTEX_POINT('',#37202);
#11343=VERTEX_POINT('',#37204);
#11344=VERTEX_POINT('',#37213);
#11345=VERTEX_POINT('',#37215);
#11346=VERTEX_POINT('',#37262);
#11347=VERTEX_POINT('',#37264);
#11348=VERTEX_POINT('',#37266);
#11349=VERTEX_POINT('',#37268);
#11350=VERTEX_POINT('',#37277);
#11351=VERTEX_POINT('',#37279);
#11352=VERTEX_POINT('',#37326);
#11353=VERTEX_POINT('',#37328);
#11354=VERTEX_POINT('',#37330);
#11355=VERTEX_POINT('',#37332);
#11356=VERTEX_POINT('',#37341);
#11357=VERTEX_POINT('',#37343);
#11358=VERTEX_POINT('',#37390);
#11359=VERTEX_POINT('',#37392);
#11360=VERTEX_POINT('',#37394);
#11361=VERTEX_POINT('',#37396);
#11362=VERTEX_POINT('',#37407);
#11363=VERTEX_POINT('',#37411);
#11364=VERTEX_POINT('',#37414);
#11365=VERTEX_POINT('',#37418);
#11366=VERTEX_POINT('',#37422);
#11367=VERTEX_POINT('',#37427);
#11368=VERTEX_POINT('',#37431);
#11369=VERTEX_POINT('',#37434);
#11370=VERTEX_POINT('',#37438);
#11371=VERTEX_POINT('',#40324);
#11372=VERTEX_POINT('',#40325);
#11373=VERTEX_POINT('',#40327);
#11374=VERTEX_POINT('',#40344);
#11375=VERTEX_POINT('',#40357);
#11376=VERTEX_POINT('',#40358);
#11377=VERTEX_POINT('',#40441);
#11378=VERTEX_POINT('',#40442);
#11379=VERTEX_POINT('',#40531);
#11380=VERTEX_POINT('',#40532);
#11381=VERTEX_POINT('',#40621);
#11382=VERTEX_POINT('',#40622);
#11383=VERTEX_POINT('',#40705);
#11384=VERTEX_POINT('',#40706);
#11385=VERTEX_POINT('',#40795);
#11386=VERTEX_POINT('',#40796);
#11387=VERTEX_POINT('',#40879);
#11388=VERTEX_POINT('',#40880);
#11389=VERTEX_POINT('',#40969);
#11390=VERTEX_POINT('',#40970);
#11391=VERTEX_POINT('',#41059);
#11392=VERTEX_POINT('',#41060);
#11393=VERTEX_POINT('',#41143);
#11394=VERTEX_POINT('',#41144);
#11395=VERTEX_POINT('',#41233);
#11396=VERTEX_POINT('',#41234);
#11397=VERTEX_POINT('',#41323);
#11398=VERTEX_POINT('',#41324);
#11399=VERTEX_POINT('',#41407);
#11400=VERTEX_POINT('',#41408);
#11401=VERTEX_POINT('',#41410);
#11402=VERTEX_POINT('',#41417);
#11403=VERTEX_POINT('',#41418);
#11404=VERTEX_POINT('',#41436);
#11405=VERTEX_POINT('',#41453);
#11406=VERTEX_POINT('',#41454);
#11407=VERTEX_POINT('',#41490);
#11408=VERTEX_POINT('',#41491);
#11409=VERTEX_POINT('',#41528);
#11410=VERTEX_POINT('',#41529);
#11411=VERTEX_POINT('',#41565);
#11412=VERTEX_POINT('',#41566);
#11413=VERTEX_POINT('',#41602);
#11414=VERTEX_POINT('',#41603);
#11415=VERTEX_POINT('',#41640);
#11416=VERTEX_POINT('',#41641);
#11417=VERTEX_POINT('',#41677);
#11418=VERTEX_POINT('',#41678);
#11419=VERTEX_POINT('',#41714);
#11420=VERTEX_POINT('',#41715);
#11421=VERTEX_POINT('',#41751);
#11422=VERTEX_POINT('',#41752);
#11423=VERTEX_POINT('',#41788);
#11424=VERTEX_POINT('',#41789);
#11425=VERTEX_POINT('',#41826);
#11426=VERTEX_POINT('',#41827);
#11427=VERTEX_POINT('',#41863);
#11428=VERTEX_POINT('',#41943);
#11429=VERTEX_POINT('',#41945);
#11430=VERTEX_POINT('',#42719);
#11431=VERTEX_POINT('',#42814);
#11432=VERTEX_POINT('',#42817);
#11433=VERTEX_POINT('',#43601);
#11434=VERTEX_POINT('',#43604);
#11435=VERTEX_POINT('',#43608);
#11436=VERTEX_POINT('',#43612);
#11437=VERTEX_POINT('',#43617);
#11438=VERTEX_POINT('',#43623);
#11439=VERTEX_POINT('',#43624);
#11440=VERTEX_POINT('',#43628);
#11441=VERTEX_POINT('',#43630);
#11442=VERTEX_POINT('',#43634);
#11443=VERTEX_POINT('',#43636);
#11444=VERTEX_POINT('',#43640);
#11445=VERTEX_POINT('',#43642);
#11446=VERTEX_POINT('',#43646);
#11447=VERTEX_POINT('',#43650);
#11448=VERTEX_POINT('',#43652);
#11449=VERTEX_POINT('',#43660);
#11450=VERTEX_POINT('',#43662);
#11451=VERTEX_POINT('',#43664);
#11452=VERTEX_POINT('',#43671);
#11453=VERTEX_POINT('',#43672);
#11454=VERTEX_POINT('',#43676);
#11455=VERTEX_POINT('',#43678);
#11456=VERTEX_POINT('',#43682);
#11457=VERTEX_POINT('',#43684);
#11458=VERTEX_POINT('',#43688);
#11459=VERTEX_POINT('',#43690);
#11460=VERTEX_POINT('',#43692);
#11461=VERTEX_POINT('',#43698);
#11462=VERTEX_POINT('',#43702);
#11463=VERTEX_POINT('',#43706);
#11464=VERTEX_POINT('',#43711);
#11465=VERTEX_POINT('',#43715);
#11466=VERTEX_POINT('',#43716);
#11467=VERTEX_POINT('',#43721);
#11468=VERTEX_POINT('',#43728);
#11469=VERTEX_POINT('',#43730);
#11470=VERTEX_POINT('',#43732);
#11471=VERTEX_POINT('',#43734);
#11472=VERTEX_POINT('',#43736);
#11473=VERTEX_POINT('',#43738);
#11474=VERTEX_POINT('',#43740);
#11475=VERTEX_POINT('',#43742);
#11476=VERTEX_POINT('',#43744);
#11477=VERTEX_POINT('',#43746);
#11478=VERTEX_POINT('',#43748);
#11479=VERTEX_POINT('',#43750);
#11480=VERTEX_POINT('',#43753);
#11481=VERTEX_POINT('',#43756);
#11482=VERTEX_POINT('',#43764);
#11483=VERTEX_POINT('',#43765);
#11484=VERTEX_POINT('',#43769);
#11485=VERTEX_POINT('',#43771);
#11486=VERTEX_POINT('',#43775);
#11487=VERTEX_POINT('',#43777);
#11488=VERTEX_POINT('',#43781);
#11489=VERTEX_POINT('',#43783);
#11490=VERTEX_POINT('',#43785);
#11491=VERTEX_POINT('',#43787);
#11492=VERTEX_POINT('',#43796);
#11493=VERTEX_POINT('',#43805);
#11494=VERTEX_POINT('',#43807);
#11495=VERTEX_POINT('',#43811);
#11496=VERTEX_POINT('',#43817);
#11497=VERTEX_POINT('',#43819);
#11498=VERTEX_POINT('',#43827);
#11499=VERTEX_POINT('',#43833);
#11500=VERTEX_POINT('',#43837);
#11501=VERTEX_POINT('',#43841);
#11502=VERTEX_POINT('',#43842);
#11503=VERTEX_POINT('',#43846);
#11504=VERTEX_POINT('',#43848);
#11505=VERTEX_POINT('',#43852);
#11506=VERTEX_POINT('',#43854);
#11507=VERTEX_POINT('',#43858);
#11508=VERTEX_POINT('',#43860);
#11509=VERTEX_POINT('',#43862);
#11510=VERTEX_POINT('',#43864);
#11511=VERTEX_POINT('',#43873);
#11512=VERTEX_POINT('',#43882);
#11513=VERTEX_POINT('',#43883);
#11514=VERTEX_POINT('',#43887);
#11515=VERTEX_POINT('',#43889);
#11516=VERTEX_POINT('',#43893);
#11517=VERTEX_POINT('',#43895);
#11518=VERTEX_POINT('',#43899);
#11519=VERTEX_POINT('',#43901);
#11520=VERTEX_POINT('',#43908);
#11521=VERTEX_POINT('',#43916);
#11522=VERTEX_POINT('',#43922);
#11523=VERTEX_POINT('',#43928);
#11524=VERTEX_POINT('',#43932);
#11525=VERTEX_POINT('',#43934);
#11526=VERTEX_POINT('',#43938);
#11527=VERTEX_POINT('',#43940);
#11528=VERTEX_POINT('',#43942);
#11529=VERTEX_POINT('',#43944);
#11530=VERTEX_POINT('',#43953);
#11531=VERTEX_POINT('',#43959);
#11532=VERTEX_POINT('',#43961);
#11533=VERTEX_POINT('',#43965);
#11534=VERTEX_POINT('',#43967);
#11535=VERTEX_POINT('',#43973);
#11536=VERTEX_POINT('',#43979);
#11537=VERTEX_POINT('',#43988);
#11538=VERTEX_POINT('',#43990);
#11539=VERTEX_POINT('',#43997);
#11540=VERTEX_POINT('',#44004);
#11541=VERTEX_POINT('',#44006);
#11542=VERTEX_POINT('',#44013);
#11543=VERTEX_POINT('',#44019);
#11544=VERTEX_POINT('',#44031);
#11545=VERTEX_POINT('',#44042);
#11546=VERTEX_POINT('',#44056);
#11547=VERTEX_POINT('',#44059);
#11548=VERTEX_POINT('',#44063);
#11549=VERTEX_POINT('',#44067);
#11550=VERTEX_POINT('',#44332);
#11551=VERTEX_POINT('',#44333);
#11552=VERTEX_POINT('',#44466);
#11553=VERTEX_POINT('',#44467);
#11554=VERTEX_POINT('',#44497);
#11555=VERTEX_POINT('',#44499);
#11556=VERTEX_POINT('',#44501);
#11557=VERTEX_POINT('',#44528);
#11558=VERTEX_POINT('',#44531);
#11559=VERTEX_POINT('',#44560);
#11560=VERTEX_POINT('',#44611);
#11561=VERTEX_POINT('',#44662);
#11562=VERTEX_POINT('',#44713);
#11563=VERTEX_POINT('',#44764);
#11564=VERTEX_POINT('',#44907);
#11565=VERTEX_POINT('',#44909);
#11566=VERTEX_POINT('',#44920);
#11567=VERTEX_POINT('',#44943);
#11568=VERTEX_POINT('',#44945);
#11569=VERTEX_POINT('',#44949);
#11570=VERTEX_POINT('',#44951);
#11571=VERTEX_POINT('',#44953);
#11572=VERTEX_POINT('',#44980);
#11573=VERTEX_POINT('',#44982);
#11574=VERTEX_POINT('',#45007);
#11575=VERTEX_POINT('',#45009);
#11576=VERTEX_POINT('',#45036);
#11577=VERTEX_POINT('',#45038);
#11578=VERTEX_POINT('',#45065);
#11579=VERTEX_POINT('',#45067);
#11580=VERTEX_POINT('',#45092);
#11581=VERTEX_POINT('',#45094);
#11582=VERTEX_POINT('',#45122);
#11583=VERTEX_POINT('',#45155);
#11584=VERTEX_POINT('',#45184);
#11585=VERTEX_POINT('',#45217);
#11586=VERTEX_POINT('',#45250);
#11587=VERTEX_POINT('',#45279);
#11588=VERTEX_POINT('',#45325);
#11589=VERTEX_POINT('',#45329);
#11590=VERTEX_POINT('',#45334);
#11591=VERTEX_POINT('',#45338);
#11592=VERTEX_POINT('',#45344);
#11593=VERTEX_POINT('',#45345);
#11594=VERTEX_POINT('',#45347);
#11595=VERTEX_POINT('',#45364);
#11596=VERTEX_POINT('',#45377);
#11597=VERTEX_POINT('',#45378);
#11598=VERTEX_POINT('',#45461);
#11599=VERTEX_POINT('',#45462);
#11600=VERTEX_POINT('',#45551);
#11601=VERTEX_POINT('',#45552);
#11602=VERTEX_POINT('',#45641);
#11603=VERTEX_POINT('',#45642);
#11604=VERTEX_POINT('',#45731);
#11605=VERTEX_POINT('',#45732);
#11606=VERTEX_POINT('',#45815);
#11607=VERTEX_POINT('',#45816);
#11608=VERTEX_POINT('',#45905);
#11609=VERTEX_POINT('',#45906);
#11610=VERTEX_POINT('',#45908);
#11611=VERTEX_POINT('',#45916);
#11612=VERTEX_POINT('',#45917);
#11613=VERTEX_POINT('',#45936);
#11614=VERTEX_POINT('',#45954);
#11615=VERTEX_POINT('',#45955);
#11616=VERTEX_POINT('',#45991);
#11617=VERTEX_POINT('',#45992);
#11618=VERTEX_POINT('',#46028);
#11619=VERTEX_POINT('',#46029);
#11620=VERTEX_POINT('',#46066);
#11621=VERTEX_POINT('',#46067);
#11622=VERTEX_POINT('',#46104);
#11623=VERTEX_POINT('',#46105);
#11624=VERTEX_POINT('',#46141);
#11625=VERTEX_POINT('',#46218);
#11626=VERTEX_POINT('',#46220);
#11627=VERTEX_POINT('',#46698);
#11628=VERTEX_POINT('',#46790);
#11629=VERTEX_POINT('',#46793);
#11630=VERTEX_POINT('',#47279);
#11631=VERTEX_POINT('',#47280);
#11632=VERTEX_POINT('',#47284);
#11633=VERTEX_POINT('',#47288);
#11634=VERTEX_POINT('',#47292);
#11635=VERTEX_POINT('',#47296);
#11636=VERTEX_POINT('',#47303);
#11637=VERTEX_POINT('',#47304);
#11638=VERTEX_POINT('',#47306);
#11639=VERTEX_POINT('',#47311);
#11640=VERTEX_POINT('',#47315);
#11641=VERTEX_POINT('',#47320);
#11642=VERTEX_POINT('',#47324);
#11643=VERTEX_POINT('',#47329);
#11644=VERTEX_POINT('',#47333);
#11645=VERTEX_POINT('',#47338);
#11646=VERTEX_POINT('',#47342);
#11647=VERTEX_POINT('',#47347);
#11648=VERTEX_POINT('',#47351);
#11649=VERTEX_POINT('',#47356);
#11650=VERTEX_POINT('',#47362);
#11651=VERTEX_POINT('',#47364);
#11652=VERTEX_POINT('',#47368);
#11653=VERTEX_POINT('',#47372);
#11654=VERTEX_POINT('',#47376);
#11655=VERTEX_POINT('',#47380);
#11656=VERTEX_POINT('',#47384);
#11657=VERTEX_POINT('',#47388);
#11658=VERTEX_POINT('',#47392);
#11659=VERTEX_POINT('',#47396);
#11660=VERTEX_POINT('',#47407);
#11661=VERTEX_POINT('',#47415);
#11662=VERTEX_POINT('',#47428);
#11663=VERTEX_POINT('',#47435);
#11664=VERTEX_POINT('',#47441);
#11665=VERTEX_POINT('',#47442);
#11666=VERTEX_POINT('',#47444);
#11667=VERTEX_POINT('',#47446);
#11668=VERTEX_POINT('',#47450);
#11669=VERTEX_POINT('',#47452);
#11670=VERTEX_POINT('',#47456);
#11671=VERTEX_POINT('',#47458);
#11672=VERTEX_POINT('',#47466);
#11673=VERTEX_POINT('',#47467);
#11674=VERTEX_POINT('',#47469);
#11675=VERTEX_POINT('',#47471);
#11676=VERTEX_POINT('',#47475);
#11677=VERTEX_POINT('',#47477);
#11678=VERTEX_POINT('',#47481);
#11679=VERTEX_POINT('',#47483);
#11680=VERTEX_POINT('',#47491);
#11681=VERTEX_POINT('',#47492);
#11682=VERTEX_POINT('',#47494);
#11683=VERTEX_POINT('',#47498);
#11684=VERTEX_POINT('',#47499);
#11685=VERTEX_POINT('',#47501);
#11686=VERTEX_POINT('',#47505);
#11687=VERTEX_POINT('',#47506);
#11688=VERTEX_POINT('',#47508);
#11689=VERTEX_POINT('',#47512);
#11690=VERTEX_POINT('',#47513);
#11691=VERTEX_POINT('',#47515);
#11692=VERTEX_POINT('',#47519);
#11693=VERTEX_POINT('',#47520);
#11694=VERTEX_POINT('',#47522);
#11695=VERTEX_POINT('',#47529);
#11696=VERTEX_POINT('',#47530);
#11697=VERTEX_POINT('',#47532);
#11698=VERTEX_POINT('',#47536);
#11699=VERTEX_POINT('',#47537);
#11700=VERTEX_POINT('',#47539);
#11701=VERTEX_POINT('',#47549);
#11702=VERTEX_POINT('',#47550);
#11703=VERTEX_POINT('',#47552);
#11704=VERTEX_POINT('',#47590);
#11705=VERTEX_POINT('',#47591);
#11706=VERTEX_POINT('',#47593);
#11707=VERTEX_POINT('',#47610);
#11708=VERTEX_POINT('',#47623);
#11709=VERTEX_POINT('',#47624);
#11710=VERTEX_POINT('',#47707);
#11711=VERTEX_POINT('',#47708);
#11712=VERTEX_POINT('',#47797);
#11713=VERTEX_POINT('',#47798);
#11714=VERTEX_POINT('',#47887);
#11715=VERTEX_POINT('',#47888);
#11716=VERTEX_POINT('',#47971);
#11717=VERTEX_POINT('',#47972);
#11718=VERTEX_POINT('',#48061);
#11719=VERTEX_POINT('',#48062);
#11720=VERTEX_POINT('',#48145);
#11721=VERTEX_POINT('',#48146);
#11722=VERTEX_POINT('',#48235);
#11723=VERTEX_POINT('',#48236);
#11724=VERTEX_POINT('',#48325);
#11725=VERTEX_POINT('',#48326);
#11726=VERTEX_POINT('',#48409);
#11727=VERTEX_POINT('',#48410);
#11728=VERTEX_POINT('',#48499);
#11729=VERTEX_POINT('',#48500);
#11730=VERTEX_POINT('',#48583);
#11731=VERTEX_POINT('',#48584);
#11732=VERTEX_POINT('',#48673);
#11733=VERTEX_POINT('',#48674);
#11734=VERTEX_POINT('',#48763);
#11735=VERTEX_POINT('',#48764);
#11736=VERTEX_POINT('',#48847);
#11737=VERTEX_POINT('',#48848);
#11738=VERTEX_POINT('',#48937);
#11739=VERTEX_POINT('',#48938);
#11740=VERTEX_POINT('',#49027);
#11741=VERTEX_POINT('',#49028);
#11742=VERTEX_POINT('',#49111);
#11743=VERTEX_POINT('',#49112);
#11744=VERTEX_POINT('',#49201);
#11745=VERTEX_POINT('',#49202);
#11746=VERTEX_POINT('',#49285);
#11747=VERTEX_POINT('',#49286);
#11748=VERTEX_POINT('',#49375);
#11749=VERTEX_POINT('',#49376);
#11750=VERTEX_POINT('',#49465);
#11751=VERTEX_POINT('',#49466);
#11752=VERTEX_POINT('',#49549);
#11753=VERTEX_POINT('',#49550);
#11754=VERTEX_POINT('',#49639);
#11755=VERTEX_POINT('',#49640);
#11756=VERTEX_POINT('',#49723);
#11757=VERTEX_POINT('',#49724);
#11758=VERTEX_POINT('',#49813);
#11759=VERTEX_POINT('',#49814);
#11760=VERTEX_POINT('',#49903);
#11761=VERTEX_POINT('',#49904);
#11762=VERTEX_POINT('',#49987);
#11763=VERTEX_POINT('',#49988);
#11764=VERTEX_POINT('',#50077);
#11765=VERTEX_POINT('',#50078);
#11766=VERTEX_POINT('',#50080);
#11767=VERTEX_POINT('',#50087);
#11768=VERTEX_POINT('',#50088);
#11769=VERTEX_POINT('',#50107);
#11770=VERTEX_POINT('',#50124);
#11771=VERTEX_POINT('',#50125);
#11772=VERTEX_POINT('',#50161);
#11773=VERTEX_POINT('',#50162);
#11774=VERTEX_POINT('',#50198);
#11775=VERTEX_POINT('',#50199);
#11776=VERTEX_POINT('',#50236);
#11777=VERTEX_POINT('',#50237);
#11778=VERTEX_POINT('',#50273);
#11779=VERTEX_POINT('',#50274);
#11780=VERTEX_POINT('',#50310);
#11781=VERTEX_POINT('',#50311);
#11782=VERTEX_POINT('',#50347);
#11783=VERTEX_POINT('',#50348);
#11784=VERTEX_POINT('',#50384);
#11785=VERTEX_POINT('',#50385);
#11786=VERTEX_POINT('',#50422);
#11787=VERTEX_POINT('',#50423);
#11788=VERTEX_POINT('',#50459);
#11789=VERTEX_POINT('',#50460);
#11790=VERTEX_POINT('',#50496);
#11791=VERTEX_POINT('',#50497);
#11792=VERTEX_POINT('',#50533);
#11793=VERTEX_POINT('',#50534);
#11794=VERTEX_POINT('',#50570);
#11795=VERTEX_POINT('',#50571);
#11796=VERTEX_POINT('',#50608);
#11797=VERTEX_POINT('',#50609);
#11798=VERTEX_POINT('',#50645);
#11799=VERTEX_POINT('',#50646);
#11800=VERTEX_POINT('',#50682);
#11801=VERTEX_POINT('',#50683);
#11802=VERTEX_POINT('',#50720);
#11803=VERTEX_POINT('',#50721);
#11804=VERTEX_POINT('',#50757);
#11805=VERTEX_POINT('',#50758);
#11806=VERTEX_POINT('',#50794);
#11807=VERTEX_POINT('',#50795);
#11808=VERTEX_POINT('',#50831);
#11809=VERTEX_POINT('',#50832);
#11810=VERTEX_POINT('',#50868);
#11811=VERTEX_POINT('',#50869);
#11812=VERTEX_POINT('',#50906);
#11813=VERTEX_POINT('',#50907);
#11814=VERTEX_POINT('',#50943);
#11815=VERTEX_POINT('',#50944);
#11816=VERTEX_POINT('',#50980);
#11817=VERTEX_POINT('',#50981);
#11818=VERTEX_POINT('',#51017);
#11819=VERTEX_POINT('',#51018);
#11820=VERTEX_POINT('',#51054);
#11821=VERTEX_POINT('',#51055);
#11822=VERTEX_POINT('',#51092);
#11823=VERTEX_POINT('',#51093);
#11824=VERTEX_POINT('',#51129);
#11825=VERTEX_POINT('',#51203);
#11826=VERTEX_POINT('',#51205);
#11827=VERTEX_POINT('',#52781);
#11828=VERTEX_POINT('',#52870);
#11829=VERTEX_POINT('',#52873);
#11830=VERTEX_POINT('',#54457);
#11831=VERTEX_POINT('',#54458);
#11832=VERTEX_POINT('',#54462);
#11833=VERTEX_POINT('',#54466);
#11834=VERTEX_POINT('',#54470);
#11835=VERTEX_POINT('',#54474);
#11836=VERTEX_POINT('',#54481);
#11837=VERTEX_POINT('',#54482);
#11838=VERTEX_POINT('',#54484);
#11839=VERTEX_POINT('',#54489);
#11840=VERTEX_POINT('',#54493);
#11841=VERTEX_POINT('',#54498);
#11842=VERTEX_POINT('',#54502);
#11843=VERTEX_POINT('',#54507);
#11844=VERTEX_POINT('',#54511);
#11845=VERTEX_POINT('',#54516);
#11846=VERTEX_POINT('',#54520);
#11847=VERTEX_POINT('',#54525);
#11848=VERTEX_POINT('',#54529);
#11849=VERTEX_POINT('',#54534);
#11850=VERTEX_POINT('',#54540);
#11851=VERTEX_POINT('',#54542);
#11852=VERTEX_POINT('',#54546);
#11853=VERTEX_POINT('',#54550);
#11854=VERTEX_POINT('',#54554);
#11855=VERTEX_POINT('',#54558);
#11856=VERTEX_POINT('',#54562);
#11857=VERTEX_POINT('',#54566);
#11858=VERTEX_POINT('',#54570);
#11859=VERTEX_POINT('',#54574);
#11860=VERTEX_POINT('',#54585);
#11861=VERTEX_POINT('',#54593);
#11862=VERTEX_POINT('',#54606);
#11863=VERTEX_POINT('',#54613);
#11864=VERTEX_POINT('',#54619);
#11865=VERTEX_POINT('',#54621);
#11866=VERTEX_POINT('',#54625);
#11867=VERTEX_POINT('',#54629);
#11868=VERTEX_POINT('',#54632);
#11869=VERTEX_POINT('',#54636);
#11870=VERTEX_POINT('',#54639);
#11871=VERTEX_POINT('',#54641);
#11872=VERTEX_POINT('',#54645);
#11873=VERTEX_POINT('',#54649);
#11874=VERTEX_POINT('',#54653);
#11875=VERTEX_POINT('',#54657);
#11876=VERTEX_POINT('',#54661);
#11877=VERTEX_POINT('',#54669);
#11878=VERTEX_POINT('',#54671);
#11879=VERTEX_POINT('',#54677);
#11880=VERTEX_POINT('',#54683);
#11881=VERTEX_POINT('',#54689);
#11882=VERTEX_POINT('',#54693);
#11883=VERTEX_POINT('',#54698);
#11884=VERTEX_POINT('',#54712);
#11885=VERTEX_POINT('',#54713);
#11886=VERTEX_POINT('',#54715);
#11887=VERTEX_POINT('',#54732);
#11888=VERTEX_POINT('',#54745);
#11889=VERTEX_POINT('',#54746);
#11890=VERTEX_POINT('',#54829);
#11891=VERTEX_POINT('',#54830);
#11892=VERTEX_POINT('',#54919);
#11893=VERTEX_POINT('',#54920);
#11894=VERTEX_POINT('',#55009);
#11895=VERTEX_POINT('',#55010);
#11896=VERTEX_POINT('',#55093);
#11897=VERTEX_POINT('',#55094);
#11898=VERTEX_POINT('',#55183);
#11899=VERTEX_POINT('',#55184);
#11900=VERTEX_POINT('',#55267);
#11901=VERTEX_POINT('',#55268);
#11902=VERTEX_POINT('',#55357);
#11903=VERTEX_POINT('',#55358);
#11904=VERTEX_POINT('',#55447);
#11905=VERTEX_POINT('',#55448);
#11906=VERTEX_POINT('',#55531);
#11907=VERTEX_POINT('',#55532);
#11908=VERTEX_POINT('',#55621);
#11909=VERTEX_POINT('',#55622);
#11910=VERTEX_POINT('',#55711);
#11911=VERTEX_POINT('',#55712);
#11912=VERTEX_POINT('',#55795);
#11913=VERTEX_POINT('',#55796);
#11914=VERTEX_POINT('',#55885);
#11915=VERTEX_POINT('',#55886);
#11916=VERTEX_POINT('',#55969);
#11917=VERTEX_POINT('',#55970);
#11918=VERTEX_POINT('',#56059);
#11919=VERTEX_POINT('',#56060);
#11920=VERTEX_POINT('',#56149);
#11921=VERTEX_POINT('',#56150);
#11922=VERTEX_POINT('',#56233);
#11923=VERTEX_POINT('',#56234);
#11924=VERTEX_POINT('',#56323);
#11925=VERTEX_POINT('',#56324);
#11926=VERTEX_POINT('',#56326);
#11927=VERTEX_POINT('',#56333);
#11928=VERTEX_POINT('',#56334);
#11929=VERTEX_POINT('',#56353);
#11930=VERTEX_POINT('',#56370);
#11931=VERTEX_POINT('',#56371);
#11932=VERTEX_POINT('',#56407);
#11933=VERTEX_POINT('',#56408);
#11934=VERTEX_POINT('',#56444);
#11935=VERTEX_POINT('',#56445);
#11936=VERTEX_POINT('',#56482);
#11937=VERTEX_POINT('',#56483);
#11938=VERTEX_POINT('',#56519);
#11939=VERTEX_POINT('',#56520);
#11940=VERTEX_POINT('',#56556);
#11941=VERTEX_POINT('',#56557);
#11942=VERTEX_POINT('',#56593);
#11943=VERTEX_POINT('',#56594);
#11944=VERTEX_POINT('',#56630);
#11945=VERTEX_POINT('',#56631);
#11946=VERTEX_POINT('',#56668);
#11947=VERTEX_POINT('',#56669);
#11948=VERTEX_POINT('',#56705);
#11949=VERTEX_POINT('',#56706);
#11950=VERTEX_POINT('',#56742);
#11951=VERTEX_POINT('',#56743);
#11952=VERTEX_POINT('',#56780);
#11953=VERTEX_POINT('',#56781);
#11954=VERTEX_POINT('',#56817);
#11955=VERTEX_POINT('',#56818);
#11956=VERTEX_POINT('',#56854);
#11957=VERTEX_POINT('',#56855);
#11958=VERTEX_POINT('',#56891);
#11959=VERTEX_POINT('',#56892);
#11960=VERTEX_POINT('',#56928);
#11961=VERTEX_POINT('',#56929);
#11962=VERTEX_POINT('',#56966);
#11963=VERTEX_POINT('',#56967);
#11964=VERTEX_POINT('',#57003);
#11965=VERTEX_POINT('',#57077);
#11966=VERTEX_POINT('',#57079);
#11967=VERTEX_POINT('',#58151);
#11968=VERTEX_POINT('',#58240);
#11969=VERTEX_POINT('',#58243);
#11970=VERTEX_POINT('',#59323);
#11971=VERTEX_POINT('',#59324);
#11972=VERTEX_POINT('',#59328);
#11973=VERTEX_POINT('',#59332);
#11974=VERTEX_POINT('',#59336);
#11975=VERTEX_POINT('',#59340);
#11976=VERTEX_POINT('',#59347);
#11977=VERTEX_POINT('',#59348);
#11978=VERTEX_POINT('',#59350);
#11979=VERTEX_POINT('',#59355);
#11980=VERTEX_POINT('',#59359);
#11981=VERTEX_POINT('',#59364);
#11982=VERTEX_POINT('',#59368);
#11983=VERTEX_POINT('',#59373);
#11984=VERTEX_POINT('',#59377);
#11985=VERTEX_POINT('',#59382);
#11986=VERTEX_POINT('',#59386);
#11987=VERTEX_POINT('',#59391);
#11988=VERTEX_POINT('',#59395);
#11989=VERTEX_POINT('',#59400);
#11990=VERTEX_POINT('',#59406);
#11991=VERTEX_POINT('',#59408);
#11992=VERTEX_POINT('',#59412);
#11993=VERTEX_POINT('',#59416);
#11994=VERTEX_POINT('',#59420);
#11995=VERTEX_POINT('',#59424);
#11996=VERTEX_POINT('',#59428);
#11997=VERTEX_POINT('',#59432);
#11998=VERTEX_POINT('',#59436);
#11999=VERTEX_POINT('',#59440);
#12000=VERTEX_POINT('',#59451);
#12001=VERTEX_POINT('',#59459);
#12002=VERTEX_POINT('',#59472);
#12003=VERTEX_POINT('',#59479);
#12004=VERTEX_POINT('',#59668);
#12005=VERTEX_POINT('',#59669);
#12006=VERTEX_POINT('',#59764);
#12007=VERTEX_POINT('',#59766);
#12008=VERTEX_POINT('',#59769);
#12009=VERTEX_POINT('',#59824);
#12010=VERTEX_POINT('',#59884);
#12011=VERTEX_POINT('',#59940);
#12012=VERTEX_POINT('',#59941);
#12013=VERTEX_POINT('',#59943);
#12014=VERTEX_POINT('',#59953);
#12015=VERTEX_POINT('',#60183);
#12016=VERTEX_POINT('',#60185);
#12017=VERTEX_POINT('',#60189);
#12018=VERTEX_POINT('',#60190);
#12019=VERTEX_POINT('',#60206);
#12020=VERTEX_POINT('',#60208);
#12021=VERTEX_POINT('',#60223);
#12022=VERTEX_POINT('',#60228);
#12023=VERTEX_POINT('',#60466);
#12024=VERTEX_POINT('',#60467);
#12025=VERTEX_POINT('',#60469);
#12026=VERTEX_POINT('',#60498);
#12027=VERTEX_POINT('',#60510);
#12028=VERTEX_POINT('',#60533);
#12029=VERTEX_POINT('',#60594);
#12030=VERTEX_POINT('',#60596);
#12031=VERTEX_POINT('',#60836);
#12032=VERTEX_POINT('',#60840);
#12033=VERTEX_POINT('',#60848);
#12034=VERTEX_POINT('',#60849);
#12035=VERTEX_POINT('',#60851);
#12036=VERTEX_POINT('',#60853);
#12037=VERTEX_POINT('',#60855);
#12038=VERTEX_POINT('',#60857);
#12039=VERTEX_POINT('',#60861);
#12040=VERTEX_POINT('',#60863);
#12041=VERTEX_POINT('',#60865);
#12042=VERTEX_POINT('',#60869);
#12043=VERTEX_POINT('',#60873);
#12044=VERTEX_POINT('',#60875);
#12045=VERTEX_POINT('',#60879);
#12046=VERTEX_POINT('',#60880);
#12047=VERTEX_POINT('',#60882);
#12048=VERTEX_POINT('',#60884);
#12049=VERTEX_POINT('',#60886);
#12050=VERTEX_POINT('',#60888);
#12051=VERTEX_POINT('',#60892);
#12052=VERTEX_POINT('',#60894);
#12053=VERTEX_POINT('',#60896);
#12054=VERTEX_POINT('',#60900);
#12055=VERTEX_POINT('',#60904);
#12056=VERTEX_POINT('',#60906);
#12057=VERTEX_POINT('',#60910);
#12058=VERTEX_POINT('',#60911);
#12059=VERTEX_POINT('',#60913);
#12060=VERTEX_POINT('',#60915);
#12061=VERTEX_POINT('',#60917);
#12062=VERTEX_POINT('',#60919);
#12063=VERTEX_POINT('',#60923);
#12064=VERTEX_POINT('',#60925);
#12065=VERTEX_POINT('',#60929);
#12066=VERTEX_POINT('',#60931);
#12067=VERTEX_POINT('',#60935);
#12068=VERTEX_POINT('',#60937);
#12069=VERTEX_POINT('',#60939);
#12070=VERTEX_POINT('',#60943);
#12071=VERTEX_POINT('',#60944);
#12072=VERTEX_POINT('',#60946);
#12073=VERTEX_POINT('',#60948);
#12074=VERTEX_POINT('',#60950);
#12075=VERTEX_POINT('',#60952);
#12076=VERTEX_POINT('',#60956);
#12077=VERTEX_POINT('',#60958);
#12078=VERTEX_POINT('',#60960);
#12079=VERTEX_POINT('',#60964);
#12080=VERTEX_POINT('',#60968);
#12081=VERTEX_POINT('',#60970);
#12082=VERTEX_POINT('',#60974);
#12083=VERTEX_POINT('',#60975);
#12084=VERTEX_POINT('',#60977);
#12085=VERTEX_POINT('',#60979);
#12086=VERTEX_POINT('',#60981);
#12087=VERTEX_POINT('',#60983);
#12088=VERTEX_POINT('',#60987);
#12089=VERTEX_POINT('',#60989);
#12090=VERTEX_POINT('',#60993);
#12091=VERTEX_POINT('',#60995);
#12092=VERTEX_POINT('',#60997);
#12093=VERTEX_POINT('',#61001);
#12094=VERTEX_POINT('',#61003);
#12095=VERTEX_POINT('',#61007);
#12096=VERTEX_POINT('',#61008);
#12097=VERTEX_POINT('',#61010);
#12098=VERTEX_POINT('',#61012);
#12099=VERTEX_POINT('',#61014);
#12100=VERTEX_POINT('',#61016);
#12101=VERTEX_POINT('',#61020);
#12102=VERTEX_POINT('',#61022);
#12103=VERTEX_POINT('',#61024);
#12104=VERTEX_POINT('',#61028);
#12105=VERTEX_POINT('',#61030);
#12106=VERTEX_POINT('',#61032);
#12107=VERTEX_POINT('',#61036);
#12108=VERTEX_POINT('',#61040);
#12109=VERTEX_POINT('',#61042);
#12110=VERTEX_POINT('',#61044);
#12111=VERTEX_POINT('',#61048);
#12112=VERTEX_POINT('',#61050);
#12113=VERTEX_POINT('',#61054);
#12114=VERTEX_POINT('',#61055);
#12115=VERTEX_POINT('',#61057);
#12116=VERTEX_POINT('',#61059);
#12117=VERTEX_POINT('',#61061);
#12118=VERTEX_POINT('',#61063);
#12119=VERTEX_POINT('',#61067);
#12120=VERTEX_POINT('',#61069);
#12121=VERTEX_POINT('',#61073);
#12122=VERTEX_POINT('',#61075);
#12123=VERTEX_POINT('',#61082);
#12124=VERTEX_POINT('',#61083);
#12125=VERTEX_POINT('',#61085);
#12126=VERTEX_POINT('',#61087);
#12127=VERTEX_POINT('',#61089);
#12128=VERTEX_POINT('',#61091);
#12129=VERTEX_POINT('',#61095);
#12130=VERTEX_POINT('',#61097);
#12131=VERTEX_POINT('',#61101);
#12132=VERTEX_POINT('',#61103);
#12133=VERTEX_POINT('',#61105);
#12134=VERTEX_POINT('',#61109);
#12135=VERTEX_POINT('',#61111);
#12136=VERTEX_POINT('',#61115);
#12137=VERTEX_POINT('',#61116);
#12138=VERTEX_POINT('',#61118);
#12139=VERTEX_POINT('',#61120);
#12140=VERTEX_POINT('',#61122);
#12141=VERTEX_POINT('',#61124);
#12142=VERTEX_POINT('',#61128);
#12143=VERTEX_POINT('',#61130);
#12144=VERTEX_POINT('',#61132);
#12145=VERTEX_POINT('',#61136);
#12146=VERTEX_POINT('',#61138);
#12147=VERTEX_POINT('',#61140);
#12148=VERTEX_POINT('',#61144);
#12149=VERTEX_POINT('',#61148);
#12150=VERTEX_POINT('',#61150);
#12151=VERTEX_POINT('',#61152);
#12152=VERTEX_POINT('',#61156);
#12153=VERTEX_POINT('',#61158);
#12154=VERTEX_POINT('',#61162);
#12155=VERTEX_POINT('',#61163);
#12156=VERTEX_POINT('',#61165);
#12157=VERTEX_POINT('',#61167);
#12158=VERTEX_POINT('',#61169);
#12159=VERTEX_POINT('',#61171);
#12160=VERTEX_POINT('',#61175);
#12161=VERTEX_POINT('',#61177);
#12162=VERTEX_POINT('',#61181);
#12163=VERTEX_POINT('',#61183);
#12164=VERTEX_POINT('',#61190);
#12165=VERTEX_POINT('',#61191);
#12166=VERTEX_POINT('',#61193);
#12167=VERTEX_POINT('',#61195);
#12168=VERTEX_POINT('',#61197);
#12169=VERTEX_POINT('',#61199);
#12170=VERTEX_POINT('',#61203);
#12171=VERTEX_POINT('',#61205);
#12172=VERTEX_POINT('',#61207);
#12173=VERTEX_POINT('',#61211);
#12174=VERTEX_POINT('',#61213);
#12175=VERTEX_POINT('',#61215);
#12176=VERTEX_POINT('',#61219);
#12177=VERTEX_POINT('',#61223);
#12178=VERTEX_POINT('',#61225);
#12179=VERTEX_POINT('',#61227);
#12180=VERTEX_POINT('',#61231);
#12181=VERTEX_POINT('',#61233);
#12182=VERTEX_POINT('',#61237);
#12183=VERTEX_POINT('',#61238);
#12184=VERTEX_POINT('',#61240);
#12185=VERTEX_POINT('',#61242);
#12186=VERTEX_POINT('',#61244);
#12187=VERTEX_POINT('',#61246);
#12188=VERTEX_POINT('',#61250);
#12189=VERTEX_POINT('',#61252);
#12190=VERTEX_POINT('',#61256);
#12191=VERTEX_POINT('',#61258);
#12192=VERTEX_POINT('',#61262);
#12193=VERTEX_POINT('',#61264);
#12194=VERTEX_POINT('',#61266);
#12195=VERTEX_POINT('',#61270);
#12196=VERTEX_POINT('',#61272);
#12197=VERTEX_POINT('',#61274);
#12198=VERTEX_POINT('',#61276);
#12199=VERTEX_POINT('',#61280);
#12200=VERTEX_POINT('',#61282);
#12201=VERTEX_POINT('',#61286);
#12202=VERTEX_POINT('',#61288);
#12203=VERTEX_POINT('',#61292);
#12204=VERTEX_POINT('',#61297);
#12205=VERTEX_POINT('',#61298);
#12206=VERTEX_POINT('',#61300);
#12207=VERTEX_POINT('',#61302);
#12208=VERTEX_POINT('',#61304);
#12209=VERTEX_POINT('',#61306);
#12210=VERTEX_POINT('',#61310);
#12211=VERTEX_POINT('',#61312);
#12212=VERTEX_POINT('',#61314);
#12213=VERTEX_POINT('',#61318);
#12214=VERTEX_POINT('',#61320);
#12215=VERTEX_POINT('',#61322);
#12216=VERTEX_POINT('',#61326);
#12217=VERTEX_POINT('',#61330);
#12218=VERTEX_POINT('',#61332);
#12219=VERTEX_POINT('',#61334);
#12220=VERTEX_POINT('',#61338);
#12221=VERTEX_POINT('',#61340);
#12222=VERTEX_POINT('',#61344);
#12223=VERTEX_POINT('',#61345);
#12224=VERTEX_POINT('',#61347);
#12225=VERTEX_POINT('',#61349);
#12226=VERTEX_POINT('',#61351);
#12227=VERTEX_POINT('',#61353);
#12228=VERTEX_POINT('',#61357);
#12229=VERTEX_POINT('',#61359);
#12230=VERTEX_POINT('',#61361);
#12231=VERTEX_POINT('',#61365);
#12232=VERTEX_POINT('',#61367);
#12233=VERTEX_POINT('',#61369);
#12234=VERTEX_POINT('',#61373);
#12235=VERTEX_POINT('',#61377);
#12236=VERTEX_POINT('',#61379);
#12237=VERTEX_POINT('',#61381);
#12238=VERTEX_POINT('',#61385);
#12239=VERTEX_POINT('',#61387);
#12240=VERTEX_POINT('',#61391);
#12241=VERTEX_POINT('',#61392);
#12242=VERTEX_POINT('',#61394);
#12243=VERTEX_POINT('',#61396);
#12244=VERTEX_POINT('',#61398);
#12245=VERTEX_POINT('',#61400);
#12246=VERTEX_POINT('',#61404);
#12247=VERTEX_POINT('',#61406);
#12248=VERTEX_POINT('',#61408);
#12249=VERTEX_POINT('',#61412);
#12250=VERTEX_POINT('',#61416);
#12251=VERTEX_POINT('',#61418);
#12252=VERTEX_POINT('',#61422);
#12253=VERTEX_POINT('',#61423);
#12254=VERTEX_POINT('',#61425);
#12255=VERTEX_POINT('',#61427);
#12256=VERTEX_POINT('',#61429);
#12257=VERTEX_POINT('',#61431);
#12258=VERTEX_POINT('',#61435);
#12259=VERTEX_POINT('',#61437);
#12260=VERTEX_POINT('',#61439);
#12261=VERTEX_POINT('',#61443);
#12262=VERTEX_POINT('',#61445);
#12263=VERTEX_POINT('',#61447);
#12264=VERTEX_POINT('',#61451);
#12265=VERTEX_POINT('',#61455);
#12266=VERTEX_POINT('',#61457);
#12267=VERTEX_POINT('',#61459);
#12268=VERTEX_POINT('',#61463);
#12269=VERTEX_POINT('',#61465);
#12270=VERTEX_POINT('',#61469);
#12271=VERTEX_POINT('',#61470);
#12272=VERTEX_POINT('',#61472);
#12273=VERTEX_POINT('',#61474);
#12274=VERTEX_POINT('',#61476);
#12275=VERTEX_POINT('',#61478);
#12276=VERTEX_POINT('',#61482);
#12277=VERTEX_POINT('',#61484);
#12278=VERTEX_POINT('',#61486);
#12279=VERTEX_POINT('',#61490);
#12280=VERTEX_POINT('',#61492);
#12281=VERTEX_POINT('',#61494);
#12282=VERTEX_POINT('',#61498);
#12283=VERTEX_POINT('',#61502);
#12284=VERTEX_POINT('',#61504);
#12285=VERTEX_POINT('',#61506);
#12286=VERTEX_POINT('',#61510);
#12287=VERTEX_POINT('',#61512);
#12288=VERTEX_POINT('',#61516);
#12289=VERTEX_POINT('',#61518);
#12290=VERTEX_POINT('',#61520);
#12291=VERTEX_POINT('',#61522);
#12292=VERTEX_POINT('',#61526);
#12293=VERTEX_POINT('',#61528);
#12294=VERTEX_POINT('',#61532);
#12295=VERTEX_POINT('',#61536);
#12296=VERTEX_POINT('',#61538);
#12297=VERTEX_POINT('',#61542);
#12298=VERTEX_POINT('',#61543);
#12299=VERTEX_POINT('',#61545);
#12300=VERTEX_POINT('',#61547);
#12301=VERTEX_POINT('',#61551);
#12302=VERTEX_POINT('',#61553);
#12303=VERTEX_POINT('',#61556);
#12304=VERTEX_POINT('',#61559);
#12305=VERTEX_POINT('',#61561);
#12306=VERTEX_POINT('',#61563);
#12307=VERTEX_POINT('',#61567);
#12308=VERTEX_POINT('',#61568);
#12309=VERTEX_POINT('',#61571);
#12310=VERTEX_POINT('',#61573);
#12311=VERTEX_POINT('',#61575);
#12312=VERTEX_POINT('',#61579);
#12313=VERTEX_POINT('',#61583);
#12314=VERTEX_POINT('',#61585);
#12315=VERTEX_POINT('',#61587);
#12316=VERTEX_POINT('',#61589);
#12317=VERTEX_POINT('',#61593);
#12318=VERTEX_POINT('',#61595);
#12319=VERTEX_POINT('',#61597);
#12320=VERTEX_POINT('',#61603);
#12321=VERTEX_POINT('',#61604);
#12322=VERTEX_POINT('',#61606);
#12323=VERTEX_POINT('',#61608);
#12324=VERTEX_POINT('',#61610);
#12325=VERTEX_POINT('',#61612);
#12326=VERTEX_POINT('',#61616);
#12327=VERTEX_POINT('',#61619);
#12328=VERTEX_POINT('',#61623);
#12329=VERTEX_POINT('',#61625);
#12330=VERTEX_POINT('',#61627);
#12331=VERTEX_POINT('',#61631);
#12332=VERTEX_POINT('',#61635);
#12333=VERTEX_POINT('',#61636);
#12334=VERTEX_POINT('',#61638);
#12335=VERTEX_POINT('',#61640);
#12336=VERTEX_POINT('',#61642);
#12337=VERTEX_POINT('',#61644);
#12338=VERTEX_POINT('',#61648);
#12339=VERTEX_POINT('',#61650);
#12340=VERTEX_POINT('',#61652);
#12341=VERTEX_POINT('',#61656);
#12342=VERTEX_POINT('',#61658);
#12343=VERTEX_POINT('',#61660);
#12344=VERTEX_POINT('',#61664);
#12345=VERTEX_POINT('',#61668);
#12346=VERTEX_POINT('',#61670);
#12347=VERTEX_POINT('',#61672);
#12348=VERTEX_POINT('',#61676);
#12349=VERTEX_POINT('',#61678);
#12350=VERTEX_POINT('',#61682);
#12351=VERTEX_POINT('',#61683);
#12352=VERTEX_POINT('',#61685);
#12353=VERTEX_POINT('',#61687);
#12354=VERTEX_POINT('',#61689);
#12355=VERTEX_POINT('',#61691);
#12356=VERTEX_POINT('',#61695);
#12357=VERTEX_POINT('',#61697);
#12358=VERTEX_POINT('',#61699);
#12359=VERTEX_POINT('',#61703);
#12360=VERTEX_POINT('',#61705);
#12361=VERTEX_POINT('',#61707);
#12362=VERTEX_POINT('',#61711);
#12363=VERTEX_POINT('',#61715);
#12364=VERTEX_POINT('',#61717);
#12365=VERTEX_POINT('',#61719);
#12366=VERTEX_POINT('',#61723);
#12367=VERTEX_POINT('',#61725);
#12368=VERTEX_POINT('',#61729);
#12369=VERTEX_POINT('',#61730);
#12370=VERTEX_POINT('',#61732);
#12371=VERTEX_POINT('',#61734);
#12372=VERTEX_POINT('',#61736);
#12373=VERTEX_POINT('',#61738);
#12374=VERTEX_POINT('',#61742);
#12375=VERTEX_POINT('',#61744);
#12376=VERTEX_POINT('',#61746);
#12377=VERTEX_POINT('',#61750);
#12378=VERTEX_POINT('',#61752);
#12379=VERTEX_POINT('',#61754);
#12380=VERTEX_POINT('',#61758);
#12381=VERTEX_POINT('',#61762);
#12382=VERTEX_POINT('',#61764);
#12383=VERTEX_POINT('',#61766);
#12384=VERTEX_POINT('',#61770);
#12385=VERTEX_POINT('',#61772);
#12386=VERTEX_POINT('',#61776);
#12387=VERTEX_POINT('',#61777);
#12388=VERTEX_POINT('',#61779);
#12389=VERTEX_POINT('',#61781);
#12390=VERTEX_POINT('',#61783);
#12391=VERTEX_POINT('',#61785);
#12392=VERTEX_POINT('',#61789);
#12393=VERTEX_POINT('',#61791);
#12394=VERTEX_POINT('',#61793);
#12395=VERTEX_POINT('',#61797);
#12396=VERTEX_POINT('',#61799);
#12397=VERTEX_POINT('',#61801);
#12398=VERTEX_POINT('',#61805);
#12399=VERTEX_POINT('',#61809);
#12400=VERTEX_POINT('',#61811);
#12401=VERTEX_POINT('',#61813);
#12402=VERTEX_POINT('',#61817);
#12403=VERTEX_POINT('',#61819);
#12404=VERTEX_POINT('',#61823);
#12405=VERTEX_POINT('',#61824);
#12406=VERTEX_POINT('',#61826);
#12407=VERTEX_POINT('',#61828);
#12408=VERTEX_POINT('',#61830);
#12409=VERTEX_POINT('',#61832);
#12410=VERTEX_POINT('',#61836);
#12411=VERTEX_POINT('',#61838);
#12412=VERTEX_POINT('',#61842);
#12413=VERTEX_POINT('',#61844);
#12414=VERTEX_POINT('',#61854);
#12415=VERTEX_POINT('',#61863);
#12416=VERTEX_POINT('',#61867);
#12417=VERTEX_POINT('',#61876);
#12418=VERTEX_POINT('',#61882);
#12419=VERTEX_POINT('',#61884);
#12420=VERTEX_POINT('',#61886);
#12421=VERTEX_POINT('',#61888);
#12422=VERTEX_POINT('',#61890);
#12423=VERTEX_POINT('',#61892);
#12424=VERTEX_POINT('',#61894);
#12425=VERTEX_POINT('',#61896);
#12426=VERTEX_POINT('',#61898);
#12427=VERTEX_POINT('',#61900);
#12428=VERTEX_POINT('',#61902);
#12429=VERTEX_POINT('',#61904);
#12430=VERTEX_POINT('',#61906);
#12431=VERTEX_POINT('',#61908);
#12432=VERTEX_POINT('',#61910);
#12433=VERTEX_POINT('',#61912);
#12434=VERTEX_POINT('',#61914);
#12435=VERTEX_POINT('',#61916);
#12436=VERTEX_POINT('',#61918);
#12437=VERTEX_POINT('',#61920);
#12438=VERTEX_POINT('',#61922);
#12439=VERTEX_POINT('',#61924);
#12440=VERTEX_POINT('',#61926);
#12441=VERTEX_POINT('',#61928);
#12442=VERTEX_POINT('',#61930);
#12443=VERTEX_POINT('',#61932);
#12444=VERTEX_POINT('',#61934);
#12445=VERTEX_POINT('',#61939);
#12446=VERTEX_POINT('',#61941);
#12447=VERTEX_POINT('',#61943);
#12448=VERTEX_POINT('',#61945);
#12449=VERTEX_POINT('',#61947);
#12450=VERTEX_POINT('',#61949);
#12451=VERTEX_POINT('',#61951);
#12452=VERTEX_POINT('',#61953);
#12453=VERTEX_POINT('',#61955);
#12454=VERTEX_POINT('',#61957);
#12455=VERTEX_POINT('',#61959);
#12456=VERTEX_POINT('',#61961);
#12457=VERTEX_POINT('',#61963);
#12458=VERTEX_POINT('',#61965);
#12459=VERTEX_POINT('',#61967);
#12460=VERTEX_POINT('',#61969);
#12461=VERTEX_POINT('',#61971);
#12462=VERTEX_POINT('',#61973);
#12463=VERTEX_POINT('',#61975);
#12464=VERTEX_POINT('',#61977);
#12465=VERTEX_POINT('',#61979);
#12466=VERTEX_POINT('',#61981);
#12467=VERTEX_POINT('',#61983);
#12468=VERTEX_POINT('',#61985);
#12469=VERTEX_POINT('',#61987);
#12470=VERTEX_POINT('',#61994);
#12471=VERTEX_POINT('',#62000);
#12472=VERTEX_POINT('',#62002);
#12473=VERTEX_POINT('',#62004);
#12474=VERTEX_POINT('',#62006);
#12475=VERTEX_POINT('',#62008);
#12476=VERTEX_POINT('',#62018);
#12477=VERTEX_POINT('',#62026);
#12478=VERTEX_POINT('',#62030);
#12479=VERTEX_POINT('',#62038);
#12480=VERTEX_POINT('',#62042);
#12481=VERTEX_POINT('',#62050);
#12482=VERTEX_POINT('',#62054);
#12483=VERTEX_POINT('',#62060);
#12484=VERTEX_POINT('',#62064);
#12485=VERTEX_POINT('',#62068);
#12486=VERTEX_POINT('',#62072);
#12487=VERTEX_POINT('',#62073);
#12488=VERTEX_POINT('',#62075);
#12489=VERTEX_POINT('',#62077);
#12490=VERTEX_POINT('',#62081);
#12491=VERTEX_POINT('',#62084);
#12492=VERTEX_POINT('',#62091);
#12493=VERTEX_POINT('',#62093);
#12494=VERTEX_POINT('',#62097);
#12495=VERTEX_POINT('',#62099);
#12496=VERTEX_POINT('',#62103);
#12497=VERTEX_POINT('',#62108);
#12498=VERTEX_POINT('',#62110);
#12499=VERTEX_POINT('',#62112);
#12500=VERTEX_POINT('',#62116);
#12501=VERTEX_POINT('',#62120);
#12502=VERTEX_POINT('',#62121);
#12503=VERTEX_POINT('',#62123);
#12504=VERTEX_POINT('',#62125);
#12505=VERTEX_POINT('',#62127);
#12506=VERTEX_POINT('',#62129);
#12507=VERTEX_POINT('',#62134);
#12508=VERTEX_POINT('',#62138);
#12509=VERTEX_POINT('',#62140);
#12510=VERTEX_POINT('',#62144);
#12511=VERTEX_POINT('',#62148);
#12512=VERTEX_POINT('',#62150);
#12513=VERTEX_POINT('',#62152);
#12514=VERTEX_POINT('',#62162);
#12515=VERTEX_POINT('',#62166);
#12516=VERTEX_POINT('',#62174);
#12517=VERTEX_POINT('',#62182);
#12518=VERTEX_POINT('',#62186);
#12519=VERTEX_POINT('',#62196);
#12520=VERTEX_POINT('',#62204);
#12521=VERTEX_POINT('',#62212);
#12522=VERTEX_POINT('',#62220);
#12523=VERTEX_POINT('',#62228);
#12524=VERTEX_POINT('',#62232);
#12525=VERTEX_POINT('',#62238);
#12526=VERTEX_POINT('',#62239);
#12527=VERTEX_POINT('',#62241);
#12528=VERTEX_POINT('',#62243);
#12529=VERTEX_POINT('',#62245);
#12530=VERTEX_POINT('',#62247);
#12531=VERTEX_POINT('',#62252);
#12532=VERTEX_POINT('',#62256);
#12533=VERTEX_POINT('',#62258);
#12534=VERTEX_POINT('',#62262);
#12535=VERTEX_POINT('',#62266);
#12536=VERTEX_POINT('',#62268);
#12537=VERTEX_POINT('',#62270);
#12538=VERTEX_POINT('',#62274);
#12539=VERTEX_POINT('',#62278);
#12540=VERTEX_POINT('',#62279);
#12541=VERTEX_POINT('',#62281);
#12542=VERTEX_POINT('',#62283);
#12543=VERTEX_POINT('',#62285);
#12544=VERTEX_POINT('',#62287);
#12545=VERTEX_POINT('',#62292);
#12546=VERTEX_POINT('',#62296);
#12547=VERTEX_POINT('',#62298);
#12548=VERTEX_POINT('',#62302);
#12549=VERTEX_POINT('',#62306);
#12550=VERTEX_POINT('',#62308);
#12551=VERTEX_POINT('',#62310);
#12552=VERTEX_POINT('',#62314);
#12553=VERTEX_POINT('',#62318);
#12554=VERTEX_POINT('',#62319);
#12555=VERTEX_POINT('',#62321);
#12556=VERTEX_POINT('',#62323);
#12557=VERTEX_POINT('',#62325);
#12558=VERTEX_POINT('',#62327);
#12559=VERTEX_POINT('',#62332);
#12560=VERTEX_POINT('',#62336);
#12561=VERTEX_POINT('',#62338);
#12562=VERTEX_POINT('',#62342);
#12563=VERTEX_POINT('',#62346);
#12564=VERTEX_POINT('',#62348);
#12565=VERTEX_POINT('',#62350);
#12566=VERTEX_POINT('',#62354);
#12567=VERTEX_POINT('',#62358);
#12568=VERTEX_POINT('',#62359);
#12569=VERTEX_POINT('',#62361);
#12570=VERTEX_POINT('',#62363);
#12571=VERTEX_POINT('',#62365);
#12572=VERTEX_POINT('',#62367);
#12573=VERTEX_POINT('',#62371);
#12574=VERTEX_POINT('',#62373);
#12575=VERTEX_POINT('',#62380);
#12576=VERTEX_POINT('',#62382);
#12577=VERTEX_POINT('',#62386);
#12578=VERTEX_POINT('',#62388);
#12579=VERTEX_POINT('',#62390);
#12580=VERTEX_POINT('',#62392);
#12581=VERTEX_POINT('',#62396);
#12582=VERTEX_POINT('',#62398);
#12583=VERTEX_POINT('',#62402);
#12584=VERTEX_POINT('',#62404);
#12585=VERTEX_POINT('',#62408);
#12586=VERTEX_POINT('',#62413);
#12587=VERTEX_POINT('',#62414);
#12588=VERTEX_POINT('',#62416);
#12589=VERTEX_POINT('',#62418);
#12590=VERTEX_POINT('',#62420);
#12591=VERTEX_POINT('',#62422);
#12592=VERTEX_POINT('',#62427);
#12593=VERTEX_POINT('',#62431);
#12594=VERTEX_POINT('',#62433);
#12595=VERTEX_POINT('',#62437);
#12596=VERTEX_POINT('',#62441);
#12597=VERTEX_POINT('',#62443);
#12598=VERTEX_POINT('',#62445);
#12599=VERTEX_POINT('',#62449);
#12600=VERTEX_POINT('',#62453);
#12601=VERTEX_POINT('',#62454);
#12602=VERTEX_POINT('',#62456);
#12603=VERTEX_POINT('',#62458);
#12604=VERTEX_POINT('',#62460);
#12605=VERTEX_POINT('',#62462);
#12606=VERTEX_POINT('',#62467);
#12607=VERTEX_POINT('',#62471);
#12608=VERTEX_POINT('',#62473);
#12609=VERTEX_POINT('',#62477);
#12610=VERTEX_POINT('',#62481);
#12611=VERTEX_POINT('',#62483);
#12612=VERTEX_POINT('',#62485);
#12613=VERTEX_POINT('',#62489);
#12614=VERTEX_POINT('',#62493);
#12615=VERTEX_POINT('',#62495);
#12616=VERTEX_POINT('',#62497);
#12617=VERTEX_POINT('',#62501);
#12618=VERTEX_POINT('',#62503);
#12619=VERTEX_POINT('',#62505);
#12620=VERTEX_POINT('',#62509);
#12621=VERTEX_POINT('',#62517);
#12622=VERTEX_POINT('',#62525);
#12623=VERTEX_POINT('',#62529);
#12624=VERTEX_POINT('',#62539);
#12625=VERTEX_POINT('',#62547);
#12626=VERTEX_POINT('',#62555);
#12627=VERTEX_POINT('',#62559);
#12628=VERTEX_POINT('',#62567);
#12629=VERTEX_POINT('',#62571);
#12630=VERTEX_POINT('',#62579);
#12631=VERTEX_POINT('',#62587);
#12632=VERTEX_POINT('',#62595);
#12633=VERTEX_POINT('',#62599);
#12634=VERTEX_POINT('',#62605);
#12635=VERTEX_POINT('',#62606);
#12636=VERTEX_POINT('',#62608);
#12637=VERTEX_POINT('',#62610);
#12638=VERTEX_POINT('',#62612);
#12639=VERTEX_POINT('',#62614);
#12640=VERTEX_POINT('',#62619);
#12641=VERTEX_POINT('',#62623);
#12642=VERTEX_POINT('',#62625);
#12643=VERTEX_POINT('',#62629);
#12644=VERTEX_POINT('',#62633);
#12645=VERTEX_POINT('',#62635);
#12646=VERTEX_POINT('',#62637);
#12647=VERTEX_POINT('',#62641);
#12648=VERTEX_POINT('',#62645);
#12649=VERTEX_POINT('',#62646);
#12650=VERTEX_POINT('',#62648);
#12651=VERTEX_POINT('',#62650);
#12652=VERTEX_POINT('',#62652);
#12653=VERTEX_POINT('',#62654);
#12654=VERTEX_POINT('',#62659);
#12655=VERTEX_POINT('',#62663);
#12656=VERTEX_POINT('',#62665);
#12657=VERTEX_POINT('',#62669);
#12658=VERTEX_POINT('',#62673);
#12659=VERTEX_POINT('',#62675);
#12660=VERTEX_POINT('',#62677);
#12661=VERTEX_POINT('',#62681);
#12662=VERTEX_POINT('',#62685);
#12663=VERTEX_POINT('',#62686);
#12664=VERTEX_POINT('',#62688);
#12665=VERTEX_POINT('',#62690);
#12666=VERTEX_POINT('',#62692);
#12667=VERTEX_POINT('',#62694);
#12668=VERTEX_POINT('',#62699);
#12669=VERTEX_POINT('',#62703);
#12670=VERTEX_POINT('',#62705);
#12671=VERTEX_POINT('',#62709);
#12672=VERTEX_POINT('',#62713);
#12673=VERTEX_POINT('',#62715);
#12674=VERTEX_POINT('',#62717);
#12675=VERTEX_POINT('',#62721);
#12676=VERTEX_POINT('',#62725);
#12677=VERTEX_POINT('',#62726);
#12678=VERTEX_POINT('',#62728);
#12679=VERTEX_POINT('',#62730);
#12680=VERTEX_POINT('',#62732);
#12681=VERTEX_POINT('',#62734);
#12682=VERTEX_POINT('',#62739);
#12683=VERTEX_POINT('',#62743);
#12684=VERTEX_POINT('',#62745);
#12685=VERTEX_POINT('',#62749);
#12686=VERTEX_POINT('',#62753);
#12687=VERTEX_POINT('',#62755);
#12688=VERTEX_POINT('',#62757);
#12689=VERTEX_POINT('',#62761);
#12690=VERTEX_POINT('',#62765);
#12691=VERTEX_POINT('',#62766);
#12692=VERTEX_POINT('',#62768);
#12693=VERTEX_POINT('',#62770);
#12694=VERTEX_POINT('',#62772);
#12695=VERTEX_POINT('',#62774);
#12696=VERTEX_POINT('',#62779);
#12697=VERTEX_POINT('',#62783);
#12698=VERTEX_POINT('',#62785);
#12699=VERTEX_POINT('',#62789);
#12700=VERTEX_POINT('',#62793);
#12701=VERTEX_POINT('',#62795);
#12702=VERTEX_POINT('',#62797);
#12703=VERTEX_POINT('',#62801);
#12704=VERTEX_POINT('',#62805);
#12705=VERTEX_POINT('',#62806);
#12706=VERTEX_POINT('',#62808);
#12707=VERTEX_POINT('',#62810);
#12708=VERTEX_POINT('',#62812);
#12709=VERTEX_POINT('',#62814);
#12710=VERTEX_POINT('',#62819);
#12711=VERTEX_POINT('',#62823);
#12712=VERTEX_POINT('',#62825);
#12713=VERTEX_POINT('',#62829);
#12714=VERTEX_POINT('',#62833);
#12715=VERTEX_POINT('',#62835);
#12716=VERTEX_POINT('',#62837);
#12717=VERTEX_POINT('',#62841);
#12718=VERTEX_POINT('',#62845);
#12719=VERTEX_POINT('',#62847);
#12720=VERTEX_POINT('',#62849);
#12721=VERTEX_POINT('',#62853);
#12722=VERTEX_POINT('',#62855);
#12723=VERTEX_POINT('',#62857);
#12724=VERTEX_POINT('',#62861);
#12725=VERTEX_POINT('',#62869);
#12726=VERTEX_POINT('',#62877);
#12727=VERTEX_POINT('',#62881);
#12728=VERTEX_POINT('',#62889);
#12729=VERTEX_POINT('',#62893);
#12730=VERTEX_POINT('',#62901);
#12731=VERTEX_POINT('',#62905);
#12732=VERTEX_POINT('',#62913);
#12733=VERTEX_POINT('',#62917);
#12734=VERTEX_POINT('',#62925);
#12735=VERTEX_POINT('',#62929);
#12736=VERTEX_POINT('',#62938);
#12737=VERTEX_POINT('',#62946);
#12738=VERTEX_POINT('',#62948);
#12739=VERTEX_POINT('',#62952);
#12740=VERTEX_POINT('',#62956);
#12741=VERTEX_POINT('',#62960);
#12742=VERTEX_POINT('',#62962);
#12743=VERTEX_POINT('',#62964);
#12744=VERTEX_POINT('',#62966);
#12745=VERTEX_POINT('',#62968);
#12746=VERTEX_POINT('',#62970);
#12747=VERTEX_POINT('',#62972);
#12748=VERTEX_POINT('',#62974);
#12749=VERTEX_POINT('',#62977);
#12750=VERTEX_POINT('',#62980);
#12751=VERTEX_POINT('',#62982);
#12752=VERTEX_POINT('',#62984);
#12753=VERTEX_POINT('',#62986);
#12754=VERTEX_POINT('',#62988);
#12755=VERTEX_POINT('',#62990);
#12756=VERTEX_POINT('',#62992);
#12757=VERTEX_POINT('',#62994);
#12758=VERTEX_POINT('',#62997);
#12759=VERTEX_POINT('',#62999);
#12760=VERTEX_POINT('',#63001);
#12761=VERTEX_POINT('',#63003);
#12762=VERTEX_POINT('',#63005);
#12763=VERTEX_POINT('',#63008);
#12764=VERTEX_POINT('',#63010);
#12765=VERTEX_POINT('',#63012);
#12766=VERTEX_POINT('',#63014);
#12767=VERTEX_POINT('',#63016);
#12768=VERTEX_POINT('',#63018);
#12769=VERTEX_POINT('',#63020);
#12770=VERTEX_POINT('',#63022);
#12771=VERTEX_POINT('',#63025);
#12772=VERTEX_POINT('',#63027);
#12773=VERTEX_POINT('',#63029);
#12774=VERTEX_POINT('',#63031);
#12775=VERTEX_POINT('',#63033);
#12776=VERTEX_POINT('',#63035);
#12777=VERTEX_POINT('',#63037);
#12778=VERTEX_POINT('',#63039);
#12779=VERTEX_POINT('',#63042);
#12780=VERTEX_POINT('',#63044);
#12781=VERTEX_POINT('',#63046);
#12782=VERTEX_POINT('',#63048);
#12783=VERTEX_POINT('',#63050);
#12784=VERTEX_POINT('',#63052);
#12785=VERTEX_POINT('',#63054);
#12786=VERTEX_POINT('',#63056);
#12787=VERTEX_POINT('',#63058);
#12788=VERTEX_POINT('',#63060);
#12789=VERTEX_POINT('',#63062);
#12790=VERTEX_POINT('',#63064);
#12791=VERTEX_POINT('',#63066);
#12792=VERTEX_POINT('',#63069);
#12793=VERTEX_POINT('',#63071);
#12794=VERTEX_POINT('',#63073);
#12795=VERTEX_POINT('',#63075);
#12796=VERTEX_POINT('',#63077);
#12797=VERTEX_POINT('',#63079);
#12798=VERTEX_POINT('',#63081);
#12799=VERTEX_POINT('',#63083);
#12800=VERTEX_POINT('',#63086);
#12801=VERTEX_POINT('',#63088);
#12802=VERTEX_POINT('',#63090);
#12803=VERTEX_POINT('',#63092);
#12804=VERTEX_POINT('',#63094);
#12805=VERTEX_POINT('',#63096);
#12806=VERTEX_POINT('',#63098);
#12807=VERTEX_POINT('',#63100);
#12808=VERTEX_POINT('',#63102);
#12809=VERTEX_POINT('',#63104);
#12810=VERTEX_POINT('',#63106);
#12811=VERTEX_POINT('',#63108);
#12812=VERTEX_POINT('',#63110);
#12813=VERTEX_POINT('',#63112);
#12814=VERTEX_POINT('',#63114);
#12815=VERTEX_POINT('',#63116);
#12816=VERTEX_POINT('',#63118);
#12817=VERTEX_POINT('',#63120);
#12818=VERTEX_POINT('',#63122);
#12819=VERTEX_POINT('',#63124);
#12820=VERTEX_POINT('',#63126);
#12821=VERTEX_POINT('',#63128);
#12822=VERTEX_POINT('',#63130);
#12823=VERTEX_POINT('',#63132);
#12824=VERTEX_POINT('',#63135);
#12825=VERTEX_POINT('',#63137);
#12826=VERTEX_POINT('',#63139);
#12827=VERTEX_POINT('',#63141);
#12828=VERTEX_POINT('',#63143);
#12829=VERTEX_POINT('',#63145);
#12830=VERTEX_POINT('',#63147);
#12831=VERTEX_POINT('',#63149);
#12832=VERTEX_POINT('',#63152);
#12833=VERTEX_POINT('',#63154);
#12834=VERTEX_POINT('',#63156);
#12835=VERTEX_POINT('',#63158);
#12836=VERTEX_POINT('',#63160);
#12837=VERTEX_POINT('',#63162);
#12838=VERTEX_POINT('',#63164);
#12839=VERTEX_POINT('',#63166);
#12840=VERTEX_POINT('',#63168);
#12841=VERTEX_POINT('',#63170);
#12842=VERTEX_POINT('',#63172);
#12843=VERTEX_POINT('',#63174);
#12844=VERTEX_POINT('',#63177);
#12845=VERTEX_POINT('',#63379);
#12846=VERTEX_POINT('',#63557);
#12847=VERTEX_POINT('',#63558);
#12848=VERTEX_POINT('',#63560);
#12849=VERTEX_POINT('',#63646);
#12850=VERTEX_POINT('',#63650);
#12851=VERTEX_POINT('',#63652);
#12852=VERTEX_POINT('',#63660);
#12853=VERTEX_POINT('',#63663);
#12854=VERTEX_POINT('',#63669);
#12855=VERTEX_POINT('',#63684);
#12856=VERTEX_POINT('',#63696);
#12857=VERTEX_POINT('',#63697);
#12858=VERTEX_POINT('',#63699);
#12859=VERTEX_POINT('',#63701);
#12860=VERTEX_POINT('',#63705);
#12861=VERTEX_POINT('',#63707);
#12862=VERTEX_POINT('',#63711);
#12863=VERTEX_POINT('',#63713);
#12864=VERTEX_POINT('',#63717);
#12865=VERTEX_POINT('',#63718);
#12866=VERTEX_POINT('',#63720);
#12867=VERTEX_POINT('',#63722);
#12868=VERTEX_POINT('',#63726);
#12869=VERTEX_POINT('',#63728);
#12870=VERTEX_POINT('',#63732);
#12871=VERTEX_POINT('',#63734);
#12872=VERTEX_POINT('',#63738);
#12873=VERTEX_POINT('',#63739);
#12874=VERTEX_POINT('',#63741);
#12875=VERTEX_POINT('',#63743);
#12876=VERTEX_POINT('',#63747);
#12877=VERTEX_POINT('',#63749);
#12878=VERTEX_POINT('',#63753);
#12879=VERTEX_POINT('',#63755);
#12880=VERTEX_POINT('',#63759);
#12881=VERTEX_POINT('',#63760);
#12882=VERTEX_POINT('',#63762);
#12883=VERTEX_POINT('',#63764);
#12884=VERTEX_POINT('',#63768);
#12885=VERTEX_POINT('',#63770);
#12886=VERTEX_POINT('',#63774);
#12887=VERTEX_POINT('',#63776);
#12888=VERTEX_POINT('',#63780);
#12889=VERTEX_POINT('',#63781);
#12890=VERTEX_POINT('',#63783);
#12891=VERTEX_POINT('',#63785);
#12892=VERTEX_POINT('',#63789);
#12893=VERTEX_POINT('',#63791);
#12894=VERTEX_POINT('',#63795);
#12895=VERTEX_POINT('',#63797);
#12896=VERTEX_POINT('',#63801);
#12897=VERTEX_POINT('',#63802);
#12898=VERTEX_POINT('',#63804);
#12899=VERTEX_POINT('',#63806);
#12900=VERTEX_POINT('',#63810);
#12901=VERTEX_POINT('',#63812);
#12902=VERTEX_POINT('',#63816);
#12903=VERTEX_POINT('',#63818);
#12904=VERTEX_POINT('',#63822);
#12905=VERTEX_POINT('',#63823);
#12906=VERTEX_POINT('',#63825);
#12907=VERTEX_POINT('',#63827);
#12908=VERTEX_POINT('',#63831);
#12909=VERTEX_POINT('',#63833);
#12910=VERTEX_POINT('',#63837);
#12911=VERTEX_POINT('',#63839);
#12912=VERTEX_POINT('',#63843);
#12913=VERTEX_POINT('',#63844);
#12914=VERTEX_POINT('',#63846);
#12915=VERTEX_POINT('',#63848);
#12916=VERTEX_POINT('',#63852);
#12917=VERTEX_POINT('',#63854);
#12918=VERTEX_POINT('',#63858);
#12919=VERTEX_POINT('',#63860);
#12920=VERTEX_POINT('',#63868);
#12921=VERTEX_POINT('',#63872);
#12922=VERTEX_POINT('',#63900);
#12923=VERTEX_POINT('',#63902);
#12924=VERTEX_POINT('',#63906);
#12925=VERTEX_POINT('',#63909);
#12926=VERTEX_POINT('',#63913);
#12927=VERTEX_POINT('',#63916);
#12928=VERTEX_POINT('',#63919);
#12929=VERTEX_POINT('',#63923);
#12930=VERTEX_POINT('',#63928);
#12931=VERTEX_POINT('',#63932);
#12932=VERTEX_POINT('',#63933);
#12933=VERTEX_POINT('',#63935);
#12934=VERTEX_POINT('',#63937);
#12935=VERTEX_POINT('',#63950);
#12936=VERTEX_POINT('',#63967);
#12937=VERTEX_POINT('',#63968);
#12938=VERTEX_POINT('',#63971);
#12939=VERTEX_POINT('',#63973);
#12940=VERTEX_POINT('',#63988);
#12941=VERTEX_POINT('',#63990);
#12942=VERTEX_POINT('',#63992);
#12943=VERTEX_POINT('',#63994);
#12944=VERTEX_POINT('',#64011);
#12945=VERTEX_POINT('',#64016);
#12946=VERTEX_POINT('',#64018);
#12947=VERTEX_POINT('',#64022);
#12948=VERTEX_POINT('',#64024);
#12949=VERTEX_POINT('',#64026);
#12950=VERTEX_POINT('',#64028);
#12951=VERTEX_POINT('',#64032);
#12952=VERTEX_POINT('',#64035);
#12953=VERTEX_POINT('',#64039);
#12954=VERTEX_POINT('',#64040);
#12955=VERTEX_POINT('',#64042);
#12956=VERTEX_POINT('',#64044);
#12957=VERTEX_POINT('',#64046);
#12958=VERTEX_POINT('',#64050);
#12959=VERTEX_POINT('',#64052);
#12960=VERTEX_POINT('',#64054);
#12961=VERTEX_POINT('',#64056);
#12962=VERTEX_POINT('',#64060);
#12963=VERTEX_POINT('',#64062);
#12964=VERTEX_POINT('',#64066);
#12965=VERTEX_POINT('',#64070);
#12966=VERTEX_POINT('',#64071);
#12967=VERTEX_POINT('',#64073);
#12968=VERTEX_POINT('',#64075);
#12969=VERTEX_POINT('',#64077);
#12970=VERTEX_POINT('',#64081);
#12971=VERTEX_POINT('',#64083);
#12972=VERTEX_POINT('',#64087);
#12973=VERTEX_POINT('',#64089);
#12974=VERTEX_POINT('',#64091);
#12975=VERTEX_POINT('',#64093);
#12976=VERTEX_POINT('',#64097);
#12977=VERTEX_POINT('',#64099);
#12978=VERTEX_POINT('',#64103);
#12979=VERTEX_POINT('',#64105);
#12980=VERTEX_POINT('',#64109);
#12981=VERTEX_POINT('',#64113);
#12982=VERTEX_POINT('',#64117);
#12983=VERTEX_POINT('',#64118);
#12984=VERTEX_POINT('',#64120);
#12985=VERTEX_POINT('',#64122);
#12986=VERTEX_POINT('',#64129);
#12987=VERTEX_POINT('',#64133);
#12988=VERTEX_POINT('',#64135);
#12989=VERTEX_POINT('',#64139);
#12990=VERTEX_POINT('',#64143);
#12991=VERTEX_POINT('',#64150);
#12992=VERTEX_POINT('',#64152);
#12993=VERTEX_POINT('',#64159);
#12994=VERTEX_POINT('',#64163);
#12995=VERTEX_POINT('',#64167);
#12996=VERTEX_POINT('',#64169);
#12997=VERTEX_POINT('',#64171);
#12998=VERTEX_POINT('',#64173);
#12999=VERTEX_POINT('',#64175);
#13000=VERTEX_POINT('',#64177);
#13001=VERTEX_POINT('',#64179);
#13002=VERTEX_POINT('',#64182);
#13003=VERTEX_POINT('',#64184);
#13004=VERTEX_POINT('',#64186);
#13005=VERTEX_POINT('',#64188);
#13006=VERTEX_POINT('',#64191);
#13007=VERTEX_POINT('',#64193);
#13008=VERTEX_POINT('',#64195);
#13009=VERTEX_POINT('',#64197);
#13010=VERTEX_POINT('',#64200);
#13011=VERTEX_POINT('',#64207);
#13012=VERTEX_POINT('',#64209);
#13013=VERTEX_POINT('',#64213);
#13014=VERTEX_POINT('',#64217);
#13015=VERTEX_POINT('',#64222);
#13016=VERTEX_POINT('',#64224);
#13017=VERTEX_POINT('',#64228);
#13018=VERTEX_POINT('',#64232);
#13019=VERTEX_POINT('',#64237);
#13020=VERTEX_POINT('',#64241);
#13021=VERTEX_POINT('',#64245);
#13022=VERTEX_POINT('',#64249);
#13023=VERTEX_POINT('',#64253);
#13024=VERTEX_POINT('',#64254);
#13025=VERTEX_POINT('',#64256);
#13026=VERTEX_POINT('',#64260);
#13027=VERTEX_POINT('',#64261);
#13028=VERTEX_POINT('',#64263);
#13029=VERTEX_POINT('',#64270);
#13030=VERTEX_POINT('',#64271);
#13031=VERTEX_POINT('',#64285);
#13032=VERTEX_POINT('',#64286);
#13033=VERTEX_POINT('',#64304);
#13034=VERTEX_POINT('',#64305);
#13035=VERTEX_POINT('',#64323);
#13036=VERTEX_POINT('',#64324);
#13037=VERTEX_POINT('',#64338);
#13038=VERTEX_POINT('',#64340);
#13039=VERTEX_POINT('',#64342);
#13040=VERTEX_POINT('',#64346);
#13041=VERTEX_POINT('',#64348);
#13042=VERTEX_POINT('',#64350);
#13043=VERTEX_POINT('',#64352);
#13044=VERTEX_POINT('',#64356);
#13045=VERTEX_POINT('',#64357);
#13046=VERTEX_POINT('',#64368);
#13047=VERTEX_POINT('',#64370);
#13048=VERTEX_POINT('',#64374);
#13049=VERTEX_POINT('',#64375);
#13050=VERTEX_POINT('',#64382);
#13051=VERTEX_POINT('',#64384);
#13052=VERTEX_POINT('',#64386);
#13053=VERTEX_POINT('',#64393);
#13054=VERTEX_POINT('',#64395);
#13055=VERTEX_POINT('',#64397);
#13056=VERTEX_POINT('',#64399);
#13057=VERTEX_POINT('',#64406);
#13058=VERTEX_POINT('',#64408);
#13059=VERTEX_POINT('',#64410);
#13060=VERTEX_POINT('',#64412);
#13061=VERTEX_POINT('',#64419);
#13062=VERTEX_POINT('',#64423);
#13063=VERTEX_POINT('',#64425);
#13064=VERTEX_POINT('',#64427);
#13065=VERTEX_POINT('',#64431);
#13066=VERTEX_POINT('',#64435);
#13067=VERTEX_POINT('',#64437);
#13068=VERTEX_POINT('',#64439);
#13069=VERTEX_POINT('',#64441);
#13070=VERTEX_POINT('',#64443);
#13071=VERTEX_POINT('',#64446);
#13072=VERTEX_POINT('',#64447);
#13073=VERTEX_POINT('',#64449);
#13074=VERTEX_POINT('',#64451);
#13075=VERTEX_POINT('',#64455);
#13076=VERTEX_POINT('',#64456);
#13077=VERTEX_POINT('',#64463);
#13078=VERTEX_POINT('',#64466);
#13079=VERTEX_POINT('',#64470);
#13080=VERTEX_POINT('',#64471);
#13081=VERTEX_POINT('',#64482);
#13082=VERTEX_POINT('',#64489);
#13083=VERTEX_POINT('',#64493);
#13084=VERTEX_POINT('',#64495);
#13085=VERTEX_POINT('',#64497);
#13086=VERTEX_POINT('',#64501);
#13087=VERTEX_POINT('',#64503);
#13088=VERTEX_POINT('',#64505);
#13089=VERTEX_POINT('',#64512);
#13090=VERTEX_POINT('',#64514);
#13091=VERTEX_POINT('',#64516);
#13092=VERTEX_POINT('',#64518);
#13093=VERTEX_POINT('',#64525);
#13094=VERTEX_POINT('',#64529);
#13095=VERTEX_POINT('',#64540);
#13096=VERTEX_POINT('',#64553);
#13097=VERTEX_POINT('',#64560);
#13098=VERTEX_POINT('',#64562);
#13099=VERTEX_POINT('',#64564);
#13100=VERTEX_POINT('',#64573);
#13101=VERTEX_POINT('',#64575);
#13102=VERTEX_POINT('',#64577);
#13103=VERTEX_POINT('',#64581);
#13104=VERTEX_POINT('',#64582);
#13105=VERTEX_POINT('',#64584);
#13106=VERTEX_POINT('',#64586);
#13107=VERTEX_POINT('',#64588);
#13108=VERTEX_POINT('',#64591);
#13109=VERTEX_POINT('',#64593);
#13110=VERTEX_POINT('',#64595);
#13111=VERTEX_POINT('',#64597);
#13112=VERTEX_POINT('',#64600);
#13113=VERTEX_POINT('',#64602);
#13114=VERTEX_POINT('',#64605);
#13115=VERTEX_POINT('',#64609);
#13116=VERTEX_POINT('',#64611);
#13117=VERTEX_POINT('',#64615);
#13118=VERTEX_POINT('',#64619);
#13119=VERTEX_POINT('',#64621);
#13120=VERTEX_POINT('',#64625);
#13121=VERTEX_POINT('',#64639);
#13122=VERTEX_POINT('',#64641);
#13123=VERTEX_POINT('',#64645);
#13124=VERTEX_POINT('',#64664);
#13125=VERTEX_POINT('',#64666);
#13126=VERTEX_POINT('',#64668);
#13127=VERTEX_POINT('',#64670);
#13128=VERTEX_POINT('',#64672);
#13129=VERTEX_POINT('',#64693);
#13130=VERTEX_POINT('',#64697);
#13131=VERTEX_POINT('',#64712);
#13132=VERTEX_POINT('',#64727);
#13133=VERTEX_POINT('',#64729);
#13134=VERTEX_POINT('',#64733);
#13135=VERTEX_POINT('',#64735);
#13136=VERTEX_POINT('',#64737);
#13137=VERTEX_POINT('',#64739);
#13138=VERTEX_POINT('',#64742);
#13139=VERTEX_POINT('',#64744);
#13140=VERTEX_POINT('',#64747);
#13141=VERTEX_POINT('',#64749);
#13142=VERTEX_POINT('',#64751);
#13143=VERTEX_POINT('',#64753);
#13144=VERTEX_POINT('',#64756);
#13145=VERTEX_POINT('',#64760);
#13146=VERTEX_POINT('',#64762);
#13147=VERTEX_POINT('',#64766);
#13148=VERTEX_POINT('',#64767);
#13149=VERTEX_POINT('',#64782);
#13150=VERTEX_POINT('',#64784);
#13151=VERTEX_POINT('',#64801);
#13152=VERTEX_POINT('',#64803);
#13153=VERTEX_POINT('',#64807);
#13154=VERTEX_POINT('',#64809);
#13155=VERTEX_POINT('',#64813);
#13156=VERTEX_POINT('',#64828);
#13157=VERTEX_POINT('',#64845);
#13158=VERTEX_POINT('',#64847);
#13159=VERTEX_POINT('',#64851);
#13160=VERTEX_POINT('',#64855);
#13161=VERTEX_POINT('',#64860);
#13162=VERTEX_POINT('',#64862);
#13163=VERTEX_POINT('',#64864);
#13164=VERTEX_POINT('',#64866);
#13165=VERTEX_POINT('',#64868);
#13166=VERTEX_POINT('',#64870);
#13167=VERTEX_POINT('',#64873);
#13168=VERTEX_POINT('',#64875);
#13169=VERTEX_POINT('',#64877);
#13170=VERTEX_POINT('',#64879);
#13171=VERTEX_POINT('',#64881);
#13172=VERTEX_POINT('',#64882);
#13173=VERTEX_POINT('',#64884);
#13174=VERTEX_POINT('',#64886);
#13175=VERTEX_POINT('',#64890);
#13176=VERTEX_POINT('',#64892);
#13177=VERTEX_POINT('',#64894);
#13178=VERTEX_POINT('',#64896);
#13179=VERTEX_POINT('',#64901);
#13180=VERTEX_POINT('',#64914);
#13181=VERTEX_POINT('',#64915);
#13182=VERTEX_POINT('',#64917);
#13183=VERTEX_POINT('',#64919);
#13184=VERTEX_POINT('',#64921);
#13185=VERTEX_POINT('',#64923);
#13186=VERTEX_POINT('',#64930);
#13187=VERTEX_POINT('',#64932);
#13188=VERTEX_POINT('',#64944);
#13189=VERTEX_POINT('',#64946);
#13190=VERTEX_POINT('',#64950);
#13191=VERTEX_POINT('',#64956);
#13192=VERTEX_POINT('',#64960);
#13193=VERTEX_POINT('',#64962);
#13194=VERTEX_POINT('',#64965);
#13195=VERTEX_POINT('',#64967);
#13196=VERTEX_POINT('',#64975);
#13197=VERTEX_POINT('',#64981);
#13198=VERTEX_POINT('',#64987);
#13199=VERTEX_POINT('',#64989);
#13200=VERTEX_POINT('',#64995);
#13201=VERTEX_POINT('',#65001);
#13202=VERTEX_POINT('',#65012);
#13203=VERTEX_POINT('',#65016);
#13204=VERTEX_POINT('',#65018);
#13205=VERTEX_POINT('',#65031);
#13206=VERTEX_POINT('',#65033);
#13207=VERTEX_POINT('',#65035);
#13208=VERTEX_POINT('',#65037);
#13209=VERTEX_POINT('',#65039);
#13210=VERTEX_POINT('',#65041);
#13211=VERTEX_POINT('',#65045);
#13212=VERTEX_POINT('',#65047);
#13213=VERTEX_POINT('',#65049);
#13214=VERTEX_POINT('',#65052);
#13215=VERTEX_POINT('',#65053);
#13216=VERTEX_POINT('',#65057);
#13217=VERTEX_POINT('',#65061);
#13218=VERTEX_POINT('',#65065);
#13219=VERTEX_POINT('',#65069);
#13220=VERTEX_POINT('',#65073);
#13221=VERTEX_POINT('',#65077);
#13222=VERTEX_POINT('',#65081);
#13223=VERTEX_POINT('',#65085);
#13224=VERTEX_POINT('',#65092);
#13225=VERTEX_POINT('',#65093);
#13226=VERTEX_POINT('',#65095);
#13227=VERTEX_POINT('',#65097);
#13228=VERTEX_POINT('',#65100);
#13229=VERTEX_POINT('',#65102);
#13230=VERTEX_POINT('',#65103);
#13231=VERTEX_POINT('',#65105);
#13232=VERTEX_POINT('',#65107);
#13233=VERTEX_POINT('',#65109);
#13234=VERTEX_POINT('',#65111);
#13235=VERTEX_POINT('',#65113);
#13236=VERTEX_POINT('',#65115);
#13237=VERTEX_POINT('',#65117);
#13238=VERTEX_POINT('',#65119);
#13239=VERTEX_POINT('',#65122);
#13240=VERTEX_POINT('',#65123);
#13241=VERTEX_POINT('',#65125);
#13242=VERTEX_POINT('',#65127);
#13243=VERTEX_POINT('',#65129);
#13244=VERTEX_POINT('',#65133);
#13245=VERTEX_POINT('',#65137);
#13246=VERTEX_POINT('',#65139);
#13247=VERTEX_POINT('',#65143);
#13248=VERTEX_POINT('',#65152);
#13249=VERTEX_POINT('',#65160);
#13250=VERTEX_POINT('',#65162);
#13251=VERTEX_POINT('',#65166);
#13252=VERTEX_POINT('',#65170);
#13253=VERTEX_POINT('',#65172);
#13254=VERTEX_POINT('',#65174);
#13255=VERTEX_POINT('',#65176);
#13256=VERTEX_POINT('',#65178);
#13257=VERTEX_POINT('',#65180);
#13258=VERTEX_POINT('',#65182);
#13259=VERTEX_POINT('',#65185);
#13260=VERTEX_POINT('',#65187);
#13261=VERTEX_POINT('',#65189);
#13262=VERTEX_POINT('',#65192);
#13263=VERTEX_POINT('',#65196);
#13264=VERTEX_POINT('',#65211);
#13265=VERTEX_POINT('',#65215);
#13266=VERTEX_POINT('',#65219);
#13267=VERTEX_POINT('',#65221);
#13268=VERTEX_POINT('',#65223);
#13269=VERTEX_POINT('',#65227);
#13270=VERTEX_POINT('',#65229);
#13271=VERTEX_POINT('',#65231);
#13272=VERTEX_POINT('',#65241);
#13273=VERTEX_POINT('',#65245);
#13274=VERTEX_POINT('',#65252);
#13275=VERTEX_POINT('',#65259);
#13276=VERTEX_POINT('',#65261);
#13277=VERTEX_POINT('',#65271);
#13278=VERTEX_POINT('',#65275);
#13279=VERTEX_POINT('',#65277);
#13280=VERTEX_POINT('',#65324);
#13281=VERTEX_POINT('',#65332);
#13282=VERTEX_POINT('',#65334);
#13283=VERTEX_POINT('',#65338);
#13284=VERTEX_POINT('',#65340);
#13285=VERTEX_POINT('',#65344);
#13286=VERTEX_POINT('',#65346);
#13287=VERTEX_POINT('',#65350);
#13288=VERTEX_POINT('',#65352);
#13289=VERTEX_POINT('',#65356);
#13290=VERTEX_POINT('',#65358);
#13291=VERTEX_POINT('',#65360);
#13292=VERTEX_POINT('',#65364);
#13293=VERTEX_POINT('',#65365);
#13294=VERTEX_POINT('',#65367);
#13295=VERTEX_POINT('',#65369);
#13296=VERTEX_POINT('',#65398);
#13297=VERTEX_POINT('',#65402);
#13298=VERTEX_POINT('',#65404);
#13299=VERTEX_POINT('',#65408);
#13300=VERTEX_POINT('',#65427);
#13301=VERTEX_POINT('',#65428);
#13302=VERTEX_POINT('',#65452);
#13303=VERTEX_POINT('',#65465);
#13304=VERTEX_POINT('',#65467);
#13305=VERTEX_POINT('',#65471);
#13306=VERTEX_POINT('',#65475);
#13307=VERTEX_POINT('',#65484);
#13308=VERTEX_POINT('',#65495);
#13309=VERTEX_POINT('',#65501);
#13310=VERTEX_POINT('',#65510);
#13311=VERTEX_POINT('',#65521);
#13312=VERTEX_POINT('',#65530);
#13313=VERTEX_POINT('',#65532);
#13314=VERTEX_POINT('',#65536);
#13315=VERTEX_POINT('',#65540);
#13316=VERTEX_POINT('',#65544);
#13317=VERTEX_POINT('',#65548);
#13318=VERTEX_POINT('',#65552);
#13319=VERTEX_POINT('',#65556);
#13320=VERTEX_POINT('',#65560);
#13321=VERTEX_POINT('',#65564);
#13322=VERTEX_POINT('',#65576);
#13323=VERTEX_POINT('',#65577);
#13324=VERTEX_POINT('',#65581);
#13325=VERTEX_POINT('',#65583);
#13326=VERTEX_POINT('',#65594);
#13327=VERTEX_POINT('',#65598);
#13328=VERTEX_POINT('',#65609);
#13329=VERTEX_POINT('',#65613);
#13330=VERTEX_POINT('',#65624);
#13331=VERTEX_POINT('',#65628);
#13332=VERTEX_POINT('',#65639);
#13333=VERTEX_POINT('',#65643);
#13334=VERTEX_POINT('',#65654);
#13335=VERTEX_POINT('',#65658);
#13336=VERTEX_POINT('',#65669);
#13337=VERTEX_POINT('',#65673);
#13338=VERTEX_POINT('',#65696);
#13339=VERTEX_POINT('',#65698);
#13340=VERTEX_POINT('',#65709);
#13341=VERTEX_POINT('',#65720);
#13342=VERTEX_POINT('',#65731);
#13343=VERTEX_POINT('',#65742);
#13344=VERTEX_POINT('',#65753);
#13345=VERTEX_POINT('',#65764);
#13346=VERTEX_POINT('',#65775);
#13347=VERTEX_POINT('',#65786);
#13348=VERTEX_POINT('',#65802);
#13349=VERTEX_POINT('',#65804);
#13350=VERTEX_POINT('',#65808);
#13351=VERTEX_POINT('',#65812);
#13352=VERTEX_POINT('',#65819);
#13353=VERTEX_POINT('',#65824);
#13354=VERTEX_POINT('',#65839);
#13355=VERTEX_POINT('',#65849);
#13356=VERTEX_POINT('',#65858);
#13357=VERTEX_POINT('',#65862);
#13358=VERTEX_POINT('',#65865);
#13359=VERTEX_POINT('',#65869);
#13360=VERTEX_POINT('',#65872);
#13361=VERTEX_POINT('',#65876);
#13362=VERTEX_POINT('',#65883);
#13363=VERTEX_POINT('',#65887);
#13364=VERTEX_POINT('',#65893);
#13365=VERTEX_POINT('',#65912);
#13366=VERTEX_POINT('',#65935);
#13367=VERTEX_POINT('',#65937);
#13368=VERTEX_POINT('',#65941);
#13369=VERTEX_POINT('',#65945);
#13370=VERTEX_POINT('',#65951);
#13371=VERTEX_POINT('',#65955);
#13372=VERTEX_POINT('',#65961);
#13373=VERTEX_POINT('',#65965);
#13374=VERTEX_POINT('',#65969);
#13375=VERTEX_POINT('',#65973);
#13376=VERTEX_POINT('',#65980);
#13377=VERTEX_POINT('',#65984);
#13378=VERTEX_POINT('',#66002);
#13379=VERTEX_POINT('',#66003);
#13380=VERTEX_POINT('',#66005);
#13381=VERTEX_POINT('',#66022);
#13382=VERTEX_POINT('',#66035);
#13383=VERTEX_POINT('',#66036);
#13384=VERTEX_POINT('',#66119);
#13385=VERTEX_POINT('',#66120);
#13386=VERTEX_POINT('',#66209);
#13387=VERTEX_POINT('',#66210);
#13388=VERTEX_POINT('',#66299);
#13389=VERTEX_POINT('',#66300);
#13390=VERTEX_POINT('',#66383);
#13391=VERTEX_POINT('',#66384);
#13392=VERTEX_POINT('',#66473);
#13393=VERTEX_POINT('',#66474);
#13394=VERTEX_POINT('',#66560);
#13395=VERTEX_POINT('',#66561);
#13396=VERTEX_POINT('',#66647);
#13397=VERTEX_POINT('',#66648);
#13398=VERTEX_POINT('',#66737);
#13399=VERTEX_POINT('',#66738);
#13400=VERTEX_POINT('',#66821);
#13401=VERTEX_POINT('',#66822);
#13402=VERTEX_POINT('',#66911);
#13403=VERTEX_POINT('',#66912);
#13404=VERTEX_POINT('',#67001);
#13405=VERTEX_POINT('',#67002);
#13406=VERTEX_POINT('',#67085);
#13407=VERTEX_POINT('',#67086);
#13408=VERTEX_POINT('',#67175);
#13409=VERTEX_POINT('',#67176);
#13410=VERTEX_POINT('',#67178);
#13411=VERTEX_POINT('',#67258);
#13412=VERTEX_POINT('',#67259);
#13413=VERTEX_POINT('',#67261);
#13414=VERTEX_POINT('',#67273);
#13415=VERTEX_POINT('',#67284);
#13416=VERTEX_POINT('',#67285);
#13417=VERTEX_POINT('',#67322);
#13418=VERTEX_POINT('',#67323);
#13419=VERTEX_POINT('',#67359);
#13420=VERTEX_POINT('',#67360);
#13421=VERTEX_POINT('',#67396);
#13422=VERTEX_POINT('',#67397);
#13423=VERTEX_POINT('',#67434);
#13424=VERTEX_POINT('',#67435);
#13425=VERTEX_POINT('',#67471);
#13426=VERTEX_POINT('',#67472);
#13427=VERTEX_POINT('',#67508);
#13428=VERTEX_POINT('',#67509);
#13429=VERTEX_POINT('',#67546);
#13430=VERTEX_POINT('',#67547);
#13431=VERTEX_POINT('',#67582);
#13432=VERTEX_POINT('',#67583);
#13433=VERTEX_POINT('',#67620);
#13434=VERTEX_POINT('',#67621);
#13435=VERTEX_POINT('',#67657);
#13436=VERTEX_POINT('',#67658);
#13437=VERTEX_POINT('',#67694);
#13438=VERTEX_POINT('',#67695);
#13439=VERTEX_POINT('',#67732);
#13440=VERTEX_POINT('',#67733);
#13441=VERTEX_POINT('',#67774);
#13442=VERTEX_POINT('',#67775);
#13443=VERTEX_POINT('',#67779);
#13444=VERTEX_POINT('',#67781);
#13445=VERTEX_POINT('',#67792);
#13446=VERTEX_POINT('',#67796);
#13447=VERTEX_POINT('',#67807);
#13448=VERTEX_POINT('',#67811);
#13449=VERTEX_POINT('',#67822);
#13450=VERTEX_POINT('',#67826);
#13451=VERTEX_POINT('',#67837);
#13452=VERTEX_POINT('',#67841);
#13453=VERTEX_POINT('',#67852);
#13454=VERTEX_POINT('',#67856);
#13455=VERTEX_POINT('',#67867);
#13456=VERTEX_POINT('',#67871);
#13457=VERTEX_POINT('',#67894);
#13458=VERTEX_POINT('',#67895);
#13459=VERTEX_POINT('',#67899);
#13460=VERTEX_POINT('',#67901);
#13461=VERTEX_POINT('',#67912);
#13462=VERTEX_POINT('',#67916);
#13463=VERTEX_POINT('',#67927);
#13464=VERTEX_POINT('',#67931);
#13465=VERTEX_POINT('',#67942);
#13466=VERTEX_POINT('',#67946);
#13467=VERTEX_POINT('',#67957);
#13468=VERTEX_POINT('',#67961);
#13469=VERTEX_POINT('',#67972);
#13470=VERTEX_POINT('',#67976);
#13471=VERTEX_POINT('',#67987);
#13472=VERTEX_POINT('',#67991);
#13473=VERTEX_POINT('',#68002);
#13474=VERTEX_POINT('',#68006);
#13475=VERTEX_POINT('',#68029);
#13476=VERTEX_POINT('',#68030);
#13477=VERTEX_POINT('',#68034);
#13478=VERTEX_POINT('',#68036);
#13479=VERTEX_POINT('',#68047);
#13480=VERTEX_POINT('',#68051);
#13481=VERTEX_POINT('',#68062);
#13482=VERTEX_POINT('',#68066);
#13483=VERTEX_POINT('',#68077);
#13484=VERTEX_POINT('',#68081);
#13485=VERTEX_POINT('',#68092);
#13486=VERTEX_POINT('',#68096);
#13487=VERTEX_POINT('',#68107);
#13488=VERTEX_POINT('',#68111);
#13489=VERTEX_POINT('',#68122);
#13490=VERTEX_POINT('',#68126);
#13491=VERTEX_POINT('',#68137);
#13492=VERTEX_POINT('',#68141);
#13493=VERTEX_POINT('',#68152);
#13494=VERTEX_POINT('',#68156);
#13495=VERTEX_POINT('',#68167);
#13496=VERTEX_POINT('',#68171);
#13497=VERTEX_POINT('',#68182);
#13498=VERTEX_POINT('',#68186);
#13499=VERTEX_POINT('',#68197);
#13500=VERTEX_POINT('',#68201);
#13501=VERTEX_POINT('',#68212);
#13502=VERTEX_POINT('',#68216);
#13503=VERTEX_POINT('',#68227);
#13504=VERTEX_POINT('',#68231);
#13505=VERTEX_POINT('',#68242);
#13506=VERTEX_POINT('',#68246);
#13507=VERTEX_POINT('',#68265);
#13508=VERTEX_POINT('',#68266);
#13509=VERTEX_POINT('',#68268);
#13510=VERTEX_POINT('',#68270);
#13511=VERTEX_POINT('',#68274);
#13512=VERTEX_POINT('',#68276);
#13513=VERTEX_POINT('',#68280);
#13514=VERTEX_POINT('',#68282);
#13515=VERTEX_POINT('',#68295);
#13516=VERTEX_POINT('',#68296);
#13517=VERTEX_POINT('',#68300);
#13518=VERTEX_POINT('',#68302);
#13519=VERTEX_POINT('',#68313);
#13520=VERTEX_POINT('',#68317);
#13521=VERTEX_POINT('',#68328);
#13522=VERTEX_POINT('',#68332);
#13523=VERTEX_POINT('',#68343);
#13524=VERTEX_POINT('',#68347);
#13525=VERTEX_POINT('',#68358);
#13526=VERTEX_POINT('',#68362);
#13527=VERTEX_POINT('',#68373);
#13528=VERTEX_POINT('',#68377);
#13529=VERTEX_POINT('',#68388);
#13530=VERTEX_POINT('',#68392);
#13531=VERTEX_POINT('',#68415);
#13532=VERTEX_POINT('',#68416);
#13533=VERTEX_POINT('',#68420);
#13534=VERTEX_POINT('',#68422);
#13535=VERTEX_POINT('',#68433);
#13536=VERTEX_POINT('',#68437);
#13537=VERTEX_POINT('',#68448);
#13538=VERTEX_POINT('',#68452);
#13539=VERTEX_POINT('',#68463);
#13540=VERTEX_POINT('',#68467);
#13541=VERTEX_POINT('',#68478);
#13542=VERTEX_POINT('',#68482);
#13543=VERTEX_POINT('',#68493);
#13544=VERTEX_POINT('',#68497);
#13545=VERTEX_POINT('',#68508);
#13546=VERTEX_POINT('',#68512);
#13547=VERTEX_POINT('',#68523);
#13548=VERTEX_POINT('',#68527);
#13549=VERTEX_POINT('',#68550);
#13550=VERTEX_POINT('',#68551);
#13551=VERTEX_POINT('',#68555);
#13552=VERTEX_POINT('',#68557);
#13553=VERTEX_POINT('',#68568);
#13554=VERTEX_POINT('',#68572);
#13555=VERTEX_POINT('',#68583);
#13556=VERTEX_POINT('',#68587);
#13557=VERTEX_POINT('',#68598);
#13558=VERTEX_POINT('',#68602);
#13559=VERTEX_POINT('',#68613);
#13560=VERTEX_POINT('',#68617);
#13561=VERTEX_POINT('',#68628);
#13562=VERTEX_POINT('',#68632);
#13563=VERTEX_POINT('',#68643);
#13564=VERTEX_POINT('',#68647);
#13565=VERTEX_POINT('',#68658);
#13566=VERTEX_POINT('',#68662);
#13567=VERTEX_POINT('',#68673);
#13568=VERTEX_POINT('',#68677);
#13569=VERTEX_POINT('',#68688);
#13570=VERTEX_POINT('',#68692);
#13571=VERTEX_POINT('',#68703);
#13572=VERTEX_POINT('',#68707);
#13573=VERTEX_POINT('',#68718);
#13574=VERTEX_POINT('',#68722);
#13575=VERTEX_POINT('',#68733);
#13576=VERTEX_POINT('',#68737);
#13577=VERTEX_POINT('',#68748);
#13578=VERTEX_POINT('',#68752);
#13579=VERTEX_POINT('',#68763);
#13580=VERTEX_POINT('',#68767);
#13581=VERTEX_POINT('',#68863);
#13582=VERTEX_POINT('',#68865);
#13583=VERTEX_POINT('',#69698);
#13584=VERTEX_POINT('',#69787);
#13585=VERTEX_POINT('',#69790);
#13586=VERTEX_POINT('',#70633);
#13587=VERTEX_POINT('',#70638);
#13588=VERTEX_POINT('',#70639);
#13589=VERTEX_POINT('',#70641);
#13590=VERTEX_POINT('',#70643);
#13591=VERTEX_POINT('',#70645);
#13592=VERTEX_POINT('',#70647);
#13593=VERTEX_POINT('',#70652);
#13594=VERTEX_POINT('',#70653);
#13595=VERTEX_POINT('',#70657);
#13596=VERTEX_POINT('',#70661);
#13597=VERTEX_POINT('',#70665);
#13598=VERTEX_POINT('',#70669);
#13599=VERTEX_POINT('',#70673);
#13600=VERTEX_POINT('',#70676);
#13601=VERTEX_POINT('',#70697);
#13602=EDGE_CURVE('',#11139,#11140,#10624,.T.);
#13603=EDGE_CURVE('',#11140,#11139,#10625,.T.);
#13604=EDGE_CURVE('',#11139,#11141,#5630,.T.);
#13605=EDGE_CURVE('',#11141,#11141,#10626,.T.);
#13606=EDGE_CURVE('',#11142,#11143,#927,.T.);
#13607=EDGE_CURVE('',#11143,#11144,#10627,.T.);
#13608=EDGE_CURVE('',#11144,#11145,#928,.T.);
#13609=EDGE_CURVE('',#11145,#11146,#5631,.T.);
#13610=EDGE_CURVE('',#11146,#11147,#10628,.T.);
#13611=EDGE_CURVE('',#11147,#11148,#5632,.T.);
#13612=EDGE_CURVE('',#11148,#11149,#929,.T.);
#13613=EDGE_CURVE('',#11149,#11150,#10629,.T.);
#13614=EDGE_CURVE('',#11150,#11151,#930,.T.);
#13615=EDGE_CURVE('',#11151,#11152,#5633,.T.);
#13616=EDGE_CURVE('',#11152,#11153,#10630,.T.);
#13617=EDGE_CURVE('',#11153,#11154,#5634,.T.);
#13618=EDGE_CURVE('',#11154,#11155,#931,.T.);
#13619=EDGE_CURVE('',#11155,#11156,#10631,.T.);
#13620=EDGE_CURVE('',#11156,#11157,#932,.T.);
#13621=EDGE_CURVE('',#11157,#11158,#5635,.T.);
#13622=EDGE_CURVE('',#11158,#11159,#10632,.T.);
#13623=EDGE_CURVE('',#11159,#11160,#5636,.T.);
#13624=EDGE_CURVE('',#11160,#11161,#933,.T.);
#13625=EDGE_CURVE('',#11161,#11162,#10633,.T.);
#13626=EDGE_CURVE('',#11162,#11163,#934,.T.);
#13627=EDGE_CURVE('',#11163,#11164,#5637,.T.);
#13628=EDGE_CURVE('',#11164,#11165,#10634,.T.);
#13629=EDGE_CURVE('',#11165,#11166,#5638,.T.);
#13630=EDGE_CURVE('',#11166,#11167,#935,.T.);
#13631=EDGE_CURVE('',#11167,#11168,#10635,.T.);
#13632=EDGE_CURVE('',#11168,#11169,#936,.T.);
#13633=EDGE_CURVE('',#11169,#11170,#5639,.T.);
#13634=EDGE_CURVE('',#11170,#11171,#10636,.T.);
#13635=EDGE_CURVE('',#11171,#11172,#5640,.T.);
#13636=EDGE_CURVE('',#11172,#11173,#937,.T.);
#13637=EDGE_CURVE('',#11173,#11174,#10637,.T.);
#13638=EDGE_CURVE('',#11174,#11175,#938,.T.);
#13639=EDGE_CURVE('',#11175,#11176,#5641,.T.);
#13640=EDGE_CURVE('',#11176,#11177,#10638,.T.);
#13641=EDGE_CURVE('',#11177,#11178,#5642,.T.);
#13642=EDGE_CURVE('',#11178,#11179,#939,.T.);
#13643=EDGE_CURVE('',#11179,#11180,#10639,.T.);
#13644=EDGE_CURVE('',#11180,#11181,#940,.T.);
#13645=EDGE_CURVE('',#11181,#11182,#5643,.T.);
#13646=EDGE_CURVE('',#11182,#11183,#10640,.T.);
#13647=EDGE_CURVE('',#11183,#11184,#5644,.T.);
#13648=EDGE_CURVE('',#11184,#11185,#941,.T.);
#13649=EDGE_CURVE('',#11185,#11186,#10641,.T.);
#13650=EDGE_CURVE('',#11186,#11187,#942,.T.);
#13651=EDGE_CURVE('',#11187,#11188,#5645,.T.);
#13652=EDGE_CURVE('',#11188,#11189,#10642,.T.);
#13653=EDGE_CURVE('',#11189,#11190,#5646,.T.);
#13654=EDGE_CURVE('',#11190,#11191,#943,.T.);
#13655=EDGE_CURVE('',#11191,#11192,#10643,.T.);
#13656=EDGE_CURVE('',#11192,#11193,#944,.T.);
#13657=EDGE_CURVE('',#11193,#11194,#5647,.T.);
#13658=EDGE_CURVE('',#11194,#11195,#10644,.T.);
#13659=EDGE_CURVE('',#11195,#11196,#5648,.T.);
#13660=EDGE_CURVE('',#11196,#11197,#945,.T.);
#13661=EDGE_CURVE('',#11197,#11198,#10645,.T.);
#13662=EDGE_CURVE('',#11198,#11199,#946,.T.);
#13663=EDGE_CURVE('',#11199,#11200,#5649,.T.);
#13664=EDGE_CURVE('',#11200,#11201,#10646,.T.);
#13665=EDGE_CURVE('',#11201,#11202,#5650,.T.);
#13666=EDGE_CURVE('',#11202,#11203,#947,.T.);
#13667=EDGE_CURVE('',#11203,#11204,#10647,.T.);
#13668=EDGE_CURVE('',#11204,#11205,#948,.T.);
#13669=EDGE_CURVE('',#11205,#11206,#5651,.T.);
#13670=EDGE_CURVE('',#11206,#11207,#10648,.T.);
#13671=EDGE_CURVE('',#11207,#11208,#5652,.T.);
#13672=EDGE_CURVE('',#11208,#11209,#949,.T.);
#13673=EDGE_CURVE('',#11209,#11210,#10649,.T.);
#13674=EDGE_CURVE('',#11210,#11211,#950,.T.);
#13675=EDGE_CURVE('',#11211,#11212,#5653,.T.);
#13676=EDGE_CURVE('',#11212,#11213,#10650,.T.);
#13677=EDGE_CURVE('',#11213,#11214,#5654,.T.);
#13678=EDGE_CURVE('',#11214,#11215,#951,.T.);
#13679=EDGE_CURVE('',#11215,#11216,#10651,.T.);
#13680=EDGE_CURVE('',#11216,#11217,#952,.T.);
#13681=EDGE_CURVE('',#11217,#11218,#5655,.T.);
#13682=EDGE_CURVE('',#11218,#11219,#10652,.T.);
#13683=EDGE_CURVE('',#11219,#11220,#5656,.T.);
#13684=EDGE_CURVE('',#11220,#11221,#953,.T.);
#13685=EDGE_CURVE('',#11221,#11222,#10653,.T.);
#13686=EDGE_CURVE('',#11222,#11223,#954,.T.);
#13687=EDGE_CURVE('',#11223,#11224,#5657,.T.);
#13688=EDGE_CURVE('',#11224,#11225,#10654,.T.);
#13689=EDGE_CURVE('',#11225,#11226,#5658,.T.);
#13690=EDGE_CURVE('',#11226,#11227,#955,.T.);
#13691=EDGE_CURVE('',#11227,#11228,#10655,.T.);
#13692=EDGE_CURVE('',#11228,#11229,#956,.T.);
#13693=EDGE_CURVE('',#11229,#11230,#5659,.T.);
#13694=EDGE_CURVE('',#11230,#11231,#10656,.T.);
#13695=EDGE_CURVE('',#11231,#11232,#5660,.T.);
#13696=EDGE_CURVE('',#11232,#11233,#957,.T.);
#13697=EDGE_CURVE('',#11233,#11234,#10657,.T.);
#13698=EDGE_CURVE('',#11234,#11235,#958,.T.);
#13699=EDGE_CURVE('',#11235,#11236,#5661,.T.);
#13700=EDGE_CURVE('',#11236,#11237,#10658,.T.);
#13701=EDGE_CURVE('',#11237,#11238,#5662,.T.);
#13702=EDGE_CURVE('',#11238,#11239,#959,.T.);
#13703=EDGE_CURVE('',#11239,#11240,#10659,.T.);
#13704=EDGE_CURVE('',#11240,#11241,#960,.T.);
#13705=EDGE_CURVE('',#11241,#11242,#5663,.T.);
#13706=EDGE_CURVE('',#11242,#11243,#10660,.T.);
#13707=EDGE_CURVE('',#11243,#11244,#5664,.T.);
#13708=EDGE_CURVE('',#11244,#11245,#961,.T.);
#13709=EDGE_CURVE('',#11245,#11246,#10661,.T.);
#13710=EDGE_CURVE('',#11246,#11247,#962,.T.);
#13711=EDGE_CURVE('',#11247,#11248,#5665,.T.);
#13712=EDGE_CURVE('',#11248,#11249,#10662,.T.);
#13713=EDGE_CURVE('',#11249,#11142,#5666,.T.);
#13714=EDGE_CURVE('',#11250,#11250,#10663,.T.);
#13715=EDGE_CURVE('',#11250,#11140,#5667,.T.);
#13716=EDGE_CURVE('',#11251,#11251,#10664,.T.);
#13717=EDGE_CURVE('',#11251,#11252,#5668,.T.);
#13718=EDGE_CURVE('',#11252,#11253,#10665,.T.);
#13719=EDGE_CURVE('',#11253,#11252,#10666,.T.);
#13720=EDGE_CURVE('',#11254,#11255,#963,.T.);
#13721=EDGE_CURVE('',#11255,#11256,#5669,.T.);
#13722=EDGE_CURVE('',#11256,#11257,#10667,.T.);
#13723=EDGE_CURVE('',#11257,#11258,#5670,.T.);
#13724=EDGE_CURVE('',#11258,#11259,#964,.T.);
#13725=EDGE_CURVE('',#11259,#11260,#10668,.T.);
#13726=EDGE_CURVE('',#11260,#11261,#965,.T.);
#13727=EDGE_CURVE('',#11261,#11262,#5671,.T.);
#13728=EDGE_CURVE('',#11262,#11263,#10669,.T.);
#13729=EDGE_CURVE('',#11263,#11264,#5672,.T.);
#13730=EDGE_CURVE('',#11264,#11265,#966,.T.);
#13731=EDGE_CURVE('',#11265,#11266,#10670,.T.);
#13732=EDGE_CURVE('',#11266,#11267,#967,.T.);
#13733=EDGE_CURVE('',#11267,#11268,#5673,.T.);
#13734=EDGE_CURVE('',#11268,#11269,#10671,.T.);
#13735=EDGE_CURVE('',#11269,#11270,#5674,.T.);
#13736=EDGE_CURVE('',#11270,#11271,#968,.T.);
#13737=EDGE_CURVE('',#11271,#11272,#10672,.T.);
#13738=EDGE_CURVE('',#11272,#11273,#969,.T.);
#13739=EDGE_CURVE('',#11273,#11274,#5675,.T.);
#13740=EDGE_CURVE('',#11274,#11275,#10673,.T.);
#13741=EDGE_CURVE('',#11275,#11276,#5676,.T.);
#13742=EDGE_CURVE('',#11276,#11277,#970,.T.);
#13743=EDGE_CURVE('',#11277,#11278,#10674,.T.);
#13744=EDGE_CURVE('',#11278,#11279,#971,.T.);
#13745=EDGE_CURVE('',#11279,#11280,#5677,.T.);
#13746=EDGE_CURVE('',#11280,#11281,#10675,.T.);
#13747=EDGE_CURVE('',#11281,#11282,#5678,.T.);
#13748=EDGE_CURVE('',#11282,#11283,#972,.T.);
#13749=EDGE_CURVE('',#11283,#11284,#10676,.T.);
#13750=EDGE_CURVE('',#11284,#11285,#973,.T.);
#13751=EDGE_CURVE('',#11285,#11286,#5679,.T.);
#13752=EDGE_CURVE('',#11286,#11287,#10677,.T.);
#13753=EDGE_CURVE('',#11287,#11288,#5680,.T.);
#13754=EDGE_CURVE('',#11288,#11289,#974,.T.);
#13755=EDGE_CURVE('',#11289,#11290,#10678,.T.);
#13756=EDGE_CURVE('',#11290,#11291,#975,.T.);
#13757=EDGE_CURVE('',#11291,#11292,#5681,.T.);
#13758=EDGE_CURVE('',#11292,#11293,#10679,.T.);
#13759=EDGE_CURVE('',#11293,#11294,#5682,.T.);
#13760=EDGE_CURVE('',#11294,#11295,#976,.T.);
#13761=EDGE_CURVE('',#11295,#11296,#10680,.T.);
#13762=EDGE_CURVE('',#11296,#11297,#977,.T.);
#13763=EDGE_CURVE('',#11297,#11298,#5683,.T.);
#13764=EDGE_CURVE('',#11298,#11299,#10681,.T.);
#13765=EDGE_CURVE('',#11299,#11300,#5684,.T.);
#13766=EDGE_CURVE('',#11300,#11301,#978,.T.);
#13767=EDGE_CURVE('',#11301,#11302,#10682,.T.);
#13768=EDGE_CURVE('',#11302,#11303,#979,.T.);
#13769=EDGE_CURVE('',#11303,#11304,#5685,.T.);
#13770=EDGE_CURVE('',#11304,#11305,#10683,.T.);
#13771=EDGE_CURVE('',#11305,#11306,#5686,.T.);
#13772=EDGE_CURVE('',#11306,#11307,#980,.T.);
#13773=EDGE_CURVE('',#11307,#11308,#10684,.T.);
#13774=EDGE_CURVE('',#11308,#11309,#981,.T.);
#13775=EDGE_CURVE('',#11309,#11310,#5687,.T.);
#13776=EDGE_CURVE('',#11310,#11311,#10685,.T.);
#13777=EDGE_CURVE('',#11311,#11312,#5688,.T.);
#13778=EDGE_CURVE('',#11312,#11313,#982,.T.);
#13779=EDGE_CURVE('',#11313,#11314,#10686,.T.);
#13780=EDGE_CURVE('',#11314,#11315,#983,.T.);
#13781=EDGE_CURVE('',#11315,#11316,#5689,.T.);
#13782=EDGE_CURVE('',#11316,#11317,#10687,.T.);
#13783=EDGE_CURVE('',#11317,#11318,#5690,.T.);
#13784=EDGE_CURVE('',#11318,#11319,#984,.T.);
#13785=EDGE_CURVE('',#11319,#11320,#10688,.T.);
#13786=EDGE_CURVE('',#11320,#11321,#985,.T.);
#13787=EDGE_CURVE('',#11321,#11322,#5691,.T.);
#13788=EDGE_CURVE('',#11322,#11323,#10689,.T.);
#13789=EDGE_CURVE('',#11323,#11324,#5692,.T.);
#13790=EDGE_CURVE('',#11324,#11325,#986,.T.);
#13791=EDGE_CURVE('',#11325,#11326,#10690,.T.);
#13792=EDGE_CURVE('',#11326,#11327,#987,.T.);
#13793=EDGE_CURVE('',#11327,#11328,#5693,.T.);
#13794=EDGE_CURVE('',#11328,#11329,#10691,.T.);
#13795=EDGE_CURVE('',#11329,#11330,#5694,.T.);
#13796=EDGE_CURVE('',#11330,#11331,#988,.T.);
#13797=EDGE_CURVE('',#11331,#11332,#10692,.T.);
#13798=EDGE_CURVE('',#11332,#11333,#989,.T.);
#13799=EDGE_CURVE('',#11333,#11334,#5695,.T.);
#13800=EDGE_CURVE('',#11334,#11335,#10693,.T.);
#13801=EDGE_CURVE('',#11335,#11336,#5696,.T.);
#13802=EDGE_CURVE('',#11336,#11337,#990,.T.);
#13803=EDGE_CURVE('',#11337,#11338,#10694,.T.);
#13804=EDGE_CURVE('',#11338,#11339,#991,.T.);
#13805=EDGE_CURVE('',#11339,#11340,#5697,.T.);
#13806=EDGE_CURVE('',#11340,#11341,#10695,.T.);
#13807=EDGE_CURVE('',#11341,#11342,#5698,.T.);
#13808=EDGE_CURVE('',#11342,#11343,#992,.T.);
#13809=EDGE_CURVE('',#11343,#11344,#10696,.T.);
#13810=EDGE_CURVE('',#11344,#11345,#993,.T.);
#13811=EDGE_CURVE('',#11345,#11346,#5699,.T.);
#13812=EDGE_CURVE('',#11346,#11347,#10697,.T.);
#13813=EDGE_CURVE('',#11347,#11348,#5700,.T.);
#13814=EDGE_CURVE('',#11348,#11349,#994,.T.);
#13815=EDGE_CURVE('',#11349,#11350,#10698,.T.);
#13816=EDGE_CURVE('',#11350,#11351,#995,.T.);
#13817=EDGE_CURVE('',#11351,#11352,#5701,.T.);
#13818=EDGE_CURVE('',#11352,#11353,#10699,.T.);
#13819=EDGE_CURVE('',#11353,#11354,#5702,.T.);
#13820=EDGE_CURVE('',#11354,#11355,#996,.T.);
#13821=EDGE_CURVE('',#11355,#11356,#10700,.T.);
#13822=EDGE_CURVE('',#11356,#11357,#997,.T.);
#13823=EDGE_CURVE('',#11357,#11358,#5703,.T.);
#13824=EDGE_CURVE('',#11358,#11359,#10701,.T.);
#13825=EDGE_CURVE('',#11359,#11360,#5704,.T.);
#13826=EDGE_CURVE('',#11360,#11361,#998,.T.);
#13827=EDGE_CURVE('',#11361,#11254,#10702,.T.);
#13828=EDGE_CURVE('',#11253,#11362,#5705,.T.);
#13829=EDGE_CURVE('',#11362,#11362,#10703,.T.);
#13830=EDGE_CURVE('',#11363,#11363,#10704,.T.);
#13831=EDGE_CURVE('',#11364,#11364,#10705,.T.);
#13832=EDGE_CURVE('',#11364,#11363,#5706,.T.);
#13833=EDGE_CURVE('',#11365,#11365,#10706,.T.);
#13834=EDGE_CURVE('',#11365,#11364,#5707,.T.);
#13835=EDGE_CURVE('',#11366,#11366,#10707,.T.);
#13836=EDGE_CURVE('',#11362,#11366,#5708,.T.);
#13837=EDGE_CURVE('',#11367,#11367,#10708,.T.);
#13838=EDGE_CURVE('',#11367,#11250,#5709,.T.);
#13839=EDGE_CURVE('',#11368,#11368,#10709,.T.);
#13840=EDGE_CURVE('',#11369,#11369,#10710,.T.);
#13841=EDGE_CURVE('',#11369,#11368,#5710,.T.);
#13842=EDGE_CURVE('',#11370,#11370,#10711,.T.);
#13843=EDGE_CURVE('',#11370,#11369,#5711,.T.);
#13844=EDGE_CURVE('',#11241,#11264,#5712,.T.);
#13845=EDGE_CURVE('',#11265,#11240,#999,.T.);
#13846=EDGE_CURVE('',#11262,#11243,#5713,.T.);
#13847=EDGE_CURVE('',#11242,#11263,#5714,.T.);
#13848=EDGE_CURVE('',#11245,#11260,#1000,.T.);
#13849=EDGE_CURVE('',#11244,#11261,#5715,.T.);
#13850=EDGE_CURVE('',#11229,#11276,#5716,.T.);
#13851=EDGE_CURVE('',#11277,#11228,#1001,.T.);
#13852=EDGE_CURVE('',#11274,#11231,#5717,.T.);
#13853=EDGE_CURVE('',#11230,#11275,#5718,.T.);
#13854=EDGE_CURVE('',#11233,#11272,#1002,.T.);
#13855=EDGE_CURVE('',#11232,#11273,#5719,.T.);
#13856=EDGE_CURVE('',#11217,#11288,#5720,.T.);
#13857=EDGE_CURVE('',#11289,#11216,#1003,.T.);
#13858=EDGE_CURVE('',#11286,#11219,#5721,.T.);
#13859=EDGE_CURVE('',#11218,#11287,#5722,.T.);
#13860=EDGE_CURVE('',#11221,#11284,#1004,.T.);
#13861=EDGE_CURVE('',#11220,#11285,#5723,.T.);
#13862=EDGE_CURVE('',#11205,#11300,#5724,.T.);
#13863=EDGE_CURVE('',#11301,#11204,#1005,.T.);
#13864=EDGE_CURVE('',#11298,#11207,#5725,.T.);
#13865=EDGE_CURVE('',#11206,#11299,#5726,.T.);
#13866=EDGE_CURVE('',#11209,#11296,#1006,.T.);
#13867=EDGE_CURVE('',#11208,#11297,#5727,.T.);
#13868=EDGE_CURVE('',#11145,#11360,#5728,.T.);
#13869=EDGE_CURVE('',#11361,#11144,#1007,.T.);
#13870=EDGE_CURVE('',#11358,#11147,#5729,.T.);
#13871=EDGE_CURVE('',#11146,#11359,#5730,.T.);
#13872=EDGE_CURVE('',#11149,#11356,#1008,.T.);
#13873=EDGE_CURVE('',#11148,#11357,#5731,.T.);
#13874=EDGE_CURVE('',#11187,#11318,#5732,.T.);
#13875=EDGE_CURVE('',#11319,#11186,#1009,.T.);
#13876=EDGE_CURVE('',#11316,#11189,#5733,.T.);
#13877=EDGE_CURVE('',#11188,#11317,#5734,.T.);
#13878=EDGE_CURVE('',#11191,#11314,#1010,.T.);
#13879=EDGE_CURVE('',#11190,#11315,#5735,.T.);
#13880=EDGE_CURVE('',#11175,#11330,#5736,.T.);
#13881=EDGE_CURVE('',#11331,#11174,#1011,.T.);
#13882=EDGE_CURVE('',#11328,#11177,#5737,.T.);
#13883=EDGE_CURVE('',#11176,#11329,#5738,.T.);
#13884=EDGE_CURVE('',#11179,#11326,#1012,.T.);
#13885=EDGE_CURVE('',#11178,#11327,#5739,.T.);
#13886=EDGE_CURVE('',#11163,#11342,#5740,.T.);
#13887=EDGE_CURVE('',#11343,#11162,#1013,.T.);
#13888=EDGE_CURVE('',#11340,#11165,#5741,.T.);
#13889=EDGE_CURVE('',#11164,#11341,#5742,.T.);
#13890=EDGE_CURVE('',#11167,#11338,#1014,.T.);
#13891=EDGE_CURVE('',#11166,#11339,#5743,.T.);
#13892=EDGE_CURVE('',#11151,#11354,#5744,.T.);
#13893=EDGE_CURVE('',#11355,#11150,#1015,.T.);
#13894=EDGE_CURVE('',#11352,#11153,#5745,.T.);
#13895=EDGE_CURVE('',#11152,#11353,#5746,.T.);
#13896=EDGE_CURVE('',#11155,#11350,#1016,.T.);
#13897=EDGE_CURVE('',#11154,#11351,#5747,.T.);
#13898=EDGE_CURVE('',#11157,#11348,#5748,.T.);
#13899=EDGE_CURVE('',#11349,#11156,#1017,.T.);
#13900=EDGE_CURVE('',#11346,#11159,#5749,.T.);
#13901=EDGE_CURVE('',#11158,#11347,#5750,.T.);
#13902=EDGE_CURVE('',#11161,#11344,#1018,.T.);
#13903=EDGE_CURVE('',#11160,#11345,#5751,.T.);
#13904=EDGE_CURVE('',#11169,#11336,#5752,.T.);
#13905=EDGE_CURVE('',#11337,#11168,#1019,.T.);
#13906=EDGE_CURVE('',#11334,#11171,#5753,.T.);
#13907=EDGE_CURVE('',#11170,#11335,#5754,.T.);
#13908=EDGE_CURVE('',#11173,#11332,#1020,.T.);
#13909=EDGE_CURVE('',#11172,#11333,#5755,.T.);
#13910=EDGE_CURVE('',#11181,#11324,#5756,.T.);
#13911=EDGE_CURVE('',#11325,#11180,#1021,.T.);
#13912=EDGE_CURVE('',#11322,#11183,#5757,.T.);
#13913=EDGE_CURVE('',#11182,#11323,#5758,.T.);
#13914=EDGE_CURVE('',#11185,#11320,#1022,.T.);
#13915=EDGE_CURVE('',#11184,#11321,#5759,.T.);
#13916=EDGE_CURVE('',#11193,#11312,#5760,.T.);
#13917=EDGE_CURVE('',#11313,#11192,#1023,.T.);
#13918=EDGE_CURVE('',#11310,#11195,#5761,.T.);
#13919=EDGE_CURVE('',#11194,#11311,#5762,.T.);
#13920=EDGE_CURVE('',#11197,#11308,#1024,.T.);
#13921=EDGE_CURVE('',#11196,#11309,#5763,.T.);
#13922=EDGE_CURVE('',#11199,#11306,#5764,.T.);
#13923=EDGE_CURVE('',#11307,#11198,#1025,.T.);
#13924=EDGE_CURVE('',#11304,#11201,#5765,.T.);
#13925=EDGE_CURVE('',#11200,#11305,#5766,.T.);
#13926=EDGE_CURVE('',#11203,#11302,#1026,.T.);
#13927=EDGE_CURVE('',#11202,#11303,#5767,.T.);
#13928=EDGE_CURVE('',#11211,#11294,#5768,.T.);
#13929=EDGE_CURVE('',#11295,#11210,#1027,.T.);
#13930=EDGE_CURVE('',#11292,#11213,#5769,.T.);
#13931=EDGE_CURVE('',#11212,#11293,#5770,.T.);
#13932=EDGE_CURVE('',#11215,#11290,#1028,.T.);
#13933=EDGE_CURVE('',#11214,#11291,#5771,.T.);
#13934=EDGE_CURVE('',#11223,#11282,#5772,.T.);
#13935=EDGE_CURVE('',#11283,#11222,#1029,.T.);
#13936=EDGE_CURVE('',#11280,#11225,#5773,.T.);
#13937=EDGE_CURVE('',#11224,#11281,#5774,.T.);
#13938=EDGE_CURVE('',#11227,#11278,#1030,.T.);
#13939=EDGE_CURVE('',#11226,#11279,#5775,.T.);
#13940=EDGE_CURVE('',#11235,#11270,#5776,.T.);
#13941=EDGE_CURVE('',#11271,#11234,#1031,.T.);
#13942=EDGE_CURVE('',#11268,#11237,#5777,.T.);
#13943=EDGE_CURVE('',#11236,#11269,#5778,.T.);
#13944=EDGE_CURVE('',#11239,#11266,#1032,.T.);
#13945=EDGE_CURVE('',#11238,#11267,#5779,.T.);
#13946=EDGE_CURVE('',#11247,#11258,#5780,.T.);
#13947=EDGE_CURVE('',#11259,#11246,#1033,.T.);
#13948=EDGE_CURVE('',#11256,#11249,#5781,.T.);
#13949=EDGE_CURVE('',#11248,#11257,#5782,.T.);
#13950=EDGE_CURVE('',#11143,#11254,#1034,.T.);
#13951=EDGE_CURVE('',#11142,#11255,#5783,.T.);
#13952=EDGE_CURVE('',#11371,#11372,#5784,.T.);
#13953=EDGE_CURVE('',#11371,#11373,#1035,.T.);
#13954=EDGE_CURVE('',#11373,#11374,#10712,.F.);
#13955=EDGE_CURVE('',#11374,#11372,#1036,.T.);
#13956=EDGE_CURVE('',#11375,#11376,#5785,.T.);
#13957=EDGE_CURVE('',#11375,#11371,#1037,.T.);
#13958=EDGE_CURVE('',#11372,#11376,#1038,.T.);
#13959=EDGE_CURVE('',#11377,#11378,#5786,.T.);
#13960=EDGE_CURVE('',#11377,#11375,#1039,.T.);
#13961=EDGE_CURVE('',#11376,#11378,#1040,.T.);
#13962=EDGE_CURVE('',#11379,#11380,#5787,.T.);
#13963=EDGE_CURVE('',#11379,#11377,#1041,.T.);
#13964=EDGE_CURVE('',#11378,#11380,#1042,.T.);
#13965=EDGE_CURVE('',#11381,#11382,#5788,.T.);
#13966=EDGE_CURVE('',#11381,#11379,#1043,.T.);
#13967=EDGE_CURVE('',#11380,#11382,#1044,.T.);
#13968=EDGE_CURVE('',#11383,#11384,#5789,.T.);
#13969=EDGE_CURVE('',#11383,#11381,#1045,.T.);
#13970=EDGE_CURVE('',#11382,#11384,#1046,.T.);
#13971=EDGE_CURVE('',#11385,#11386,#5790,.T.);
#13972=EDGE_CURVE('',#11385,#11383,#1047,.T.);
#13973=EDGE_CURVE('',#11384,#11386,#1048,.T.);
#13974=EDGE_CURVE('',#11387,#11388,#5791,.T.);
#13975=EDGE_CURVE('',#11387,#11385,#1049,.T.);
#13976=EDGE_CURVE('',#11386,#11388,#1050,.T.);
#13977=EDGE_CURVE('',#11389,#11390,#5792,.T.);
#13978=EDGE_CURVE('',#11389,#11387,#1051,.T.);
#13979=EDGE_CURVE('',#11388,#11390,#1052,.T.);
#13980=EDGE_CURVE('',#11391,#11392,#5793,.T.);
#13981=EDGE_CURVE('',#11391,#11389,#1053,.T.);
#13982=EDGE_CURVE('',#11390,#11392,#1054,.T.);
#13983=EDGE_CURVE('',#11393,#11394,#5794,.T.);
#13984=EDGE_CURVE('',#11393,#11391,#1055,.T.);
#13985=EDGE_CURVE('',#11392,#11394,#1056,.T.);
#13986=EDGE_CURVE('',#11395,#11396,#5795,.T.);
#13987=EDGE_CURVE('',#11395,#11393,#1057,.T.);
#13988=EDGE_CURVE('',#11394,#11396,#1058,.T.);
#13989=EDGE_CURVE('',#11397,#11398,#5796,.T.);
#13990=EDGE_CURVE('',#11397,#11395,#1059,.T.);
#13991=EDGE_CURVE('',#11396,#11398,#1060,.T.);
#13992=EDGE_CURVE('',#11399,#11400,#5797,.T.);
#13993=EDGE_CURVE('',#11399,#11401,#1061,.T.);
#13994=EDGE_CURVE('',#11400,#11401,#10713,.T.);
#13995=EDGE_CURVE('',#11402,#11403,#5798,.T.);
#13996=EDGE_CURVE('',#11402,#11399,#1062,.T.);
#13997=EDGE_CURVE('',#11404,#11400,#10714,.T.);
#13998=EDGE_CURVE('',#11403,#11404,#1063,.T.);
#13999=EDGE_CURVE('',#11405,#11406,#5799,.T.);
#14000=EDGE_CURVE('',#11405,#11402,#1064,.T.);
#14001=EDGE_CURVE('',#11406,#11403,#1065,.T.);
#14002=EDGE_CURVE('',#11407,#11408,#5800,.T.);
#14003=EDGE_CURVE('',#11407,#11405,#1066,.T.);
#14004=EDGE_CURVE('',#11408,#11406,#1067,.T.);
#14005=EDGE_CURVE('',#11409,#11410,#5801,.T.);
#14006=EDGE_CURVE('',#11409,#11407,#1068,.T.);
#14007=EDGE_CURVE('',#11410,#11408,#1069,.T.);
#14008=EDGE_CURVE('',#11411,#11412,#5802,.T.);
#14009=EDGE_CURVE('',#11411,#11409,#1070,.T.);
#14010=EDGE_CURVE('',#11412,#11410,#1071,.T.);
#14011=EDGE_CURVE('',#11413,#11414,#5803,.T.);
#14012=EDGE_CURVE('',#11413,#11411,#1072,.T.);
#14013=EDGE_CURVE('',#11414,#11412,#1073,.T.);
#14014=EDGE_CURVE('',#11415,#11416,#5804,.T.);
#14015=EDGE_CURVE('',#11415,#11413,#1074,.T.);
#14016=EDGE_CURVE('',#11416,#11414,#1075,.T.);
#14017=EDGE_CURVE('',#11417,#11418,#5805,.T.);
#14018=EDGE_CURVE('',#11417,#11415,#1076,.T.);
#14019=EDGE_CURVE('',#11418,#11416,#1077,.T.);
#14020=EDGE_CURVE('',#11419,#11420,#5806,.T.);
#14021=EDGE_CURVE('',#11419,#11417,#1078,.T.);
#14022=EDGE_CURVE('',#11420,#11418,#1079,.T.);
#14023=EDGE_CURVE('',#11421,#11422,#5807,.T.);
#14024=EDGE_CURVE('',#11421,#11419,#1080,.T.);
#14025=EDGE_CURVE('',#11422,#11420,#1081,.T.);
#14026=EDGE_CURVE('',#11423,#11424,#5808,.T.);
#14027=EDGE_CURVE('',#11423,#11421,#1082,.T.);
#14028=EDGE_CURVE('',#11424,#11422,#1083,.T.);
#14029=EDGE_CURVE('',#11425,#11426,#5809,.T.);
#14030=EDGE_CURVE('',#11425,#11423,#1084,.T.);
#14031=EDGE_CURVE('',#11426,#11424,#1085,.T.);
#14032=EDGE_CURVE('',#11401,#11427,#1086,.T.);
#14033=EDGE_CURVE('',#11428,#11427,#10715,.F.);
#14034=EDGE_CURVE('',#11429,#11428,#10716,.F.);
#14035=EDGE_CURVE('',#11429,#11404,#1087,.T.);
#14036=EDGE_CURVE('',#11398,#11429,#1088,.T.);
#14037=EDGE_CURVE('',#11430,#11374,#1089,.T.);
#14038=EDGE_CURVE('',#11430,#11426,#1090,.T.);
#14039=EDGE_CURVE('',#11374,#11431,#10717,.F.);
#14040=EDGE_CURVE('',#11431,#11373,#10718,.F.);
#14041=EDGE_CURVE('',#11373,#11432,#1091,.T.);
#14042=EDGE_CURVE('',#11432,#11430,#10719,.T.);
#14043=EDGE_CURVE('',#11432,#11425,#1092,.T.);
#14044=EDGE_CURVE('',#11427,#11397,#1093,.T.);
#14045=EDGE_CURVE('',#11427,#11429,#10720,.F.);
#14046=EDGE_CURVE('',#11433,#11433,#10721,.T.);
#14047=EDGE_CURVE('',#11434,#11434,#10722,.T.);
#14048=EDGE_CURVE('',#11434,#11433,#5810,.T.);
#14049=EDGE_CURVE('',#11435,#11435,#10723,.T.);
#14050=EDGE_CURVE('',#11435,#11434,#5811,.T.);
#14051=EDGE_CURVE('',#11436,#11436,#10724,.T.);
#14052=EDGE_CURVE('',#11431,#11436,#5812,.T.);
#14053=EDGE_CURVE('',#11437,#11437,#10725,.T.);
#14054=EDGE_CURVE('',#11437,#11428,#5813,.T.);
#14055=EDGE_CURVE('',#11438,#11439,#171,.T.);
#14056=EDGE_CURVE('',#11439,#11440,#5814,.T.);
#14057=EDGE_CURVE('',#11440,#11441,#172,.T.);
#14058=EDGE_CURVE('',#11441,#11442,#5815,.T.);
#14059=EDGE_CURVE('',#11442,#11443,#5816,.T.);
#14060=EDGE_CURVE('',#11443,#11438,#5817,.T.);
#14061=EDGE_CURVE('',#11444,#11439,#10726,.T.);
#14062=EDGE_CURVE('',#11445,#11444,#5818,.T.);
#14063=EDGE_CURVE('',#11440,#11445,#10727,.T.);
#14064=EDGE_CURVE('',#11446,#11438,#173,.T.);
#14065=EDGE_CURVE('',#11447,#11446,#10728,.T.);
#14066=EDGE_CURVE('',#11448,#11447,#174,.T.);
#14067=EDGE_CURVE('',#11444,#11448,#175,.T.);
#14068=EDGE_CURVE('',#11443,#11449,#5819,.T.);
#14069=EDGE_CURVE('',#11449,#11450,#5820,.T.);
#14070=EDGE_CURVE('',#11450,#11451,#5821,.T.);
#14071=EDGE_CURVE('',#11446,#11451,#1094,.T.);
#14072=EDGE_CURVE('',#11452,#11453,#176,.T.);
#14073=EDGE_CURVE('',#11453,#11454,#5822,.T.);
#14074=EDGE_CURVE('',#11454,#11455,#177,.T.);
#14075=EDGE_CURVE('',#11455,#11456,#5823,.T.);
#14076=EDGE_CURVE('',#11456,#11457,#5824,.T.);
#14077=EDGE_CURVE('',#11457,#11452,#5825,.T.);
#14078=EDGE_CURVE('',#11457,#11458,#5826,.T.);
#14079=EDGE_CURVE('',#11458,#11459,#5827,.T.);
#14080=EDGE_CURVE('',#11459,#11460,#5828,.T.);
#14081=EDGE_CURVE('',#11460,#11452,#178,.T.);
#14082=EDGE_CURVE('',#11461,#11456,#5829,.T.);
#14083=EDGE_CURVE('',#11461,#11458,#5830,.T.);
#14084=EDGE_CURVE('',#11455,#11462,#179,.T.);
#14085=EDGE_CURVE('',#11463,#11462,#1095,.T.);
#14086=EDGE_CURVE('',#11463,#11464,#5831,.T.);
#14087=EDGE_CURVE('',#11461,#11464,#5832,.T.);
#14088=EDGE_CURVE('',#11465,#11466,#5833,.T.);
#14089=EDGE_CURVE('',#11466,#11459,#10729,.T.);
#14090=EDGE_CURVE('',#11458,#11465,#10730,.T.);
#14091=EDGE_CURVE('',#11441,#11467,#180,.T.);
#14092=EDGE_CURVE('',#11467,#11466,#5834,.T.);
#14093=EDGE_CURVE('',#11465,#11442,#5835,.T.);
#14094=EDGE_CURVE('',#11468,#11467,#10731,.T.);
#14095=EDGE_CURVE('',#11469,#11468,#5836,.T.);
#14096=EDGE_CURVE('',#11470,#11469,#10732,.T.);
#14097=EDGE_CURVE('',#11471,#11470,#5837,.T.);
#14098=EDGE_CURVE('',#11472,#11471,#10733,.T.);
#14099=EDGE_CURVE('',#11473,#11472,#5838,.T.);
#14100=EDGE_CURVE('',#11474,#11473,#10734,.T.);
#14101=EDGE_CURVE('',#11475,#11474,#5839,.T.);
#14102=EDGE_CURVE('',#11476,#11475,#10735,.T.);
#14103=EDGE_CURVE('',#11477,#11476,#5840,.T.);
#14104=EDGE_CURVE('',#11478,#11477,#10736,.T.);
#14105=EDGE_CURVE('',#11479,#11478,#5841,.T.);
#14106=EDGE_CURVE('',#11460,#11479,#10737,.T.);
#14107=EDGE_CURVE('',#11480,#11480,#10738,.T.);
#14108=EDGE_CURVE('',#11481,#11445,#181,.T.);
#14109=EDGE_CURVE('',#11468,#11481,#182,.T.);
#14110=EDGE_CURVE('',#11482,#11483,#183,.T.);
#14111=EDGE_CURVE('',#11483,#11484,#5842,.T.);
#14112=EDGE_CURVE('',#11484,#11485,#184,.T.);
#14113=EDGE_CURVE('',#11485,#11486,#5843,.T.);
#14114=EDGE_CURVE('',#11486,#11487,#5844,.T.);
#14115=EDGE_CURVE('',#11487,#11482,#5845,.T.);
#14116=EDGE_CURVE('',#11487,#11488,#5846,.T.);
#14117=EDGE_CURVE('',#11488,#11489,#5847,.T.);
#14118=EDGE_CURVE('',#11489,#11490,#5848,.T.);
#14119=EDGE_CURVE('',#11491,#11490,#1096,.T.);
#14120=EDGE_CURVE('',#11491,#11482,#185,.T.);
#14121=EDGE_CURVE('',#11492,#11486,#5849,.T.);
#14122=EDGE_CURVE('',#11488,#11492,#5850,.T.);
#14123=EDGE_CURVE('',#11485,#11471,#186,.T.);
#14124=EDGE_CURVE('',#11492,#11470,#5851,.T.);
#14125=EDGE_CURVE('',#11448,#11493,#5852,.T.);
#14126=EDGE_CURVE('',#11493,#11494,#5853,.T.);
#14127=EDGE_CURVE('',#11494,#11481,#5854,.T.);
#14128=EDGE_CURVE('',#11494,#11495,#5855,.T.);
#14129=EDGE_CURVE('',#11495,#11469,#5856,.T.);
#14130=EDGE_CURVE('',#11495,#11492,#10739,.T.);
#14131=EDGE_CURVE('',#11484,#11496,#10740,.T.);
#14132=EDGE_CURVE('',#11497,#11496,#187,.T.);
#14133=EDGE_CURVE('',#11472,#11497,#188,.T.);
#14134=EDGE_CURVE('',#11498,#11495,#5857,.T.);
#14135=EDGE_CURVE('',#11488,#11498,#10741,.T.);
#14136=EDGE_CURVE('',#11498,#11493,#5858,.T.);
#14137=EDGE_CURVE('',#11480,#11499,#5859,.T.);
#14138=EDGE_CURVE('',#11499,#11499,#10742,.T.);
#14139=EDGE_CURVE('',#11500,#11500,#10743,.T.);
#14140=EDGE_CURVE('',#11500,#11499,#5860,.T.);
#14141=EDGE_CURVE('',#11501,#11502,#189,.T.);
#14142=EDGE_CURVE('',#11502,#11503,#5861,.T.);
#14143=EDGE_CURVE('',#11503,#11504,#190,.T.);
#14144=EDGE_CURVE('',#11504,#11505,#5862,.T.);
#14145=EDGE_CURVE('',#11505,#11506,#5863,.T.);
#14146=EDGE_CURVE('',#11506,#11501,#5864,.T.);
#14147=EDGE_CURVE('',#11506,#11507,#5865,.T.);
#14148=EDGE_CURVE('',#11507,#11508,#5866,.T.);
#14149=EDGE_CURVE('',#11508,#11509,#5867,.T.);
#14150=EDGE_CURVE('',#11510,#11509,#1097,.T.);
#14151=EDGE_CURVE('',#11510,#11501,#191,.T.);
#14152=EDGE_CURVE('',#11511,#11505,#5868,.T.);
#14153=EDGE_CURVE('',#11507,#11511,#5869,.T.);
#14154=EDGE_CURVE('',#11504,#11479,#192,.T.);
#14155=EDGE_CURVE('',#11511,#11478,#5870,.T.);
#14156=EDGE_CURVE('',#11512,#11513,#193,.T.);
#14157=EDGE_CURVE('',#11513,#11514,#5871,.T.);
#14158=EDGE_CURVE('',#11514,#11515,#194,.T.);
#14159=EDGE_CURVE('',#11515,#11516,#5872,.T.);
#14160=EDGE_CURVE('',#11516,#11517,#5873,.T.);
#14161=EDGE_CURVE('',#11517,#11512,#5874,.T.);
#14162=EDGE_CURVE('',#11518,#11513,#10744,.T.);
#14163=EDGE_CURVE('',#11519,#11518,#5875,.T.);
#14164=EDGE_CURVE('',#11514,#11519,#10745,.T.);
#14165=EDGE_CURVE('',#11476,#11512,#195,.T.);
#14166=EDGE_CURVE('',#11520,#11475,#196,.T.);
#14167=EDGE_CURVE('',#11518,#11520,#197,.T.);
#14168=EDGE_CURVE('',#11517,#11521,#5876,.T.);
#14169=EDGE_CURVE('',#11521,#11477,#5877,.T.);
#14170=EDGE_CURVE('',#11521,#11511,#10746,.T.);
#14171=EDGE_CURVE('',#11522,#11521,#5878,.T.);
#14172=EDGE_CURVE('',#11507,#11522,#10747,.T.);
#14173=EDGE_CURVE('',#11522,#11516,#5879,.T.);
#14174=EDGE_CURVE('',#11523,#11519,#198,.T.);
#14175=EDGE_CURVE('',#11520,#11524,#5880,.T.);
#14176=EDGE_CURVE('',#11524,#11525,#5881,.T.);
#14177=EDGE_CURVE('',#11525,#11523,#5882,.T.);
#14178=EDGE_CURVE('',#11525,#11526,#5883,.T.);
#14179=EDGE_CURVE('',#11526,#11527,#5884,.T.);
#14180=EDGE_CURVE('',#11527,#11528,#5885,.T.);
#14181=EDGE_CURVE('',#11529,#11528,#1098,.T.);
#14182=EDGE_CURVE('',#11529,#11523,#199,.T.);
#14183=EDGE_CURVE('',#11530,#11524,#5886,.T.);
#14184=EDGE_CURVE('',#11526,#11530,#5887,.T.);
#14185=EDGE_CURVE('',#11530,#11474,#5888,.T.);
#14186=EDGE_CURVE('',#11496,#11531,#5889,.T.);
#14187=EDGE_CURVE('',#11531,#11532,#200,.T.);
#14188=EDGE_CURVE('',#11532,#11533,#5890,.T.);
#14189=EDGE_CURVE('',#11533,#11534,#5891,.T.);
#14190=EDGE_CURVE('',#11534,#11497,#5892,.T.);
#14191=EDGE_CURVE('',#11531,#11483,#10748,.T.);
#14192=EDGE_CURVE('',#11534,#11535,#5893,.T.);
#14193=EDGE_CURVE('',#11535,#11473,#5894,.T.);
#14194=EDGE_CURVE('',#11535,#11530,#10749,.T.);
#14195=EDGE_CURVE('',#11536,#11535,#5895,.T.);
#14196=EDGE_CURVE('',#11526,#11536,#10750,.T.);
#14197=EDGE_CURVE('',#11536,#11533,#5896,.T.);
#14198=EDGE_CURVE('',#11509,#11463,#10751,.T.);
#14199=EDGE_CURVE('',#11462,#11510,#10752,.T.);
#14200=EDGE_CURVE('',#11537,#11529,#10753,.T.);
#14201=EDGE_CURVE('',#11528,#11538,#10754,.T.);
#14202=EDGE_CURVE('',#11538,#11537,#1099,.T.);
#14203=EDGE_CURVE('',#11451,#11539,#10755,.T.);
#14204=EDGE_CURVE('',#11539,#11447,#1100,.T.);
#14205=EDGE_CURVE('',#11540,#11491,#10756,.T.);
#14206=EDGE_CURVE('',#11490,#11541,#10757,.T.);
#14207=EDGE_CURVE('',#11541,#11540,#1101,.T.);
#14208=EDGE_CURVE('',#11498,#11542,#5897,.T.);
#14209=EDGE_CURVE('',#11542,#11489,#10758,.T.);
#14210=EDGE_CURVE('',#11539,#11542,#5898,.T.);
#14211=EDGE_CURVE('',#11536,#11543,#5899,.T.);
#14212=EDGE_CURVE('',#11543,#11527,#10759,.T.);
#14213=EDGE_CURVE('',#11532,#11540,#201,.T.);
#14214=EDGE_CURVE('',#11541,#11543,#5900,.T.);
#14215=EDGE_CURVE('',#11464,#11450,#10760,.T.);
#14216=EDGE_CURVE('',#11449,#11461,#10761,.T.);
#14217=EDGE_CURVE('',#11522,#11544,#5901,.T.);
#14218=EDGE_CURVE('',#11544,#11508,#10762,.T.);
#14219=EDGE_CURVE('',#11515,#11537,#202,.T.);
#14220=EDGE_CURVE('',#11538,#11544,#5902,.T.);
#14221=EDGE_CURVE('',#11545,#11545,#10763,.T.);
#14222=EDGE_CURVE('',#11545,#11500,#5903,.T.);
#14223=EDGE_CURVE('',#11449,#11465,#5904,.T.);
#14224=EDGE_CURVE('',#11454,#11502,#10764,.T.);
#14225=EDGE_CURVE('',#11503,#11453,#10765,.T.);
#14226=EDGE_CURVE('',#11546,#11546,#10766,.T.);
#14227=EDGE_CURVE('',#11547,#11547,#10767,.T.);
#14228=EDGE_CURVE('',#11547,#11546,#5905,.T.);
#14229=EDGE_CURVE('',#11548,#11548,#10768,.T.);
#14230=EDGE_CURVE('',#11548,#11547,#5906,.T.);
#14231=EDGE_CURVE('',#11549,#11549,#10769,.T.);
#14232=EDGE_CURVE('',#11549,#11548,#5907,.T.);
#14233=EDGE_CURVE('',#11550,#11551,#5908,.T.);
#14234=EDGE_CURVE('',#11551,#11551,#1102,.T.);
#14235=EDGE_CURVE('',#11550,#11550,#1103,.T.);
#14236=EDGE_CURVE('',#11552,#11553,#1104,.T.);
#14237=EDGE_CURVE('',#11553,#11552,#1105,.T.);
#14238=EDGE_CURVE('',#11553,#11551,#5909,.T.);
#14239=EDGE_CURVE('',#11554,#11554,#10770,.T.);
#14240=EDGE_CURVE('',#11554,#11555,#5910,.T.);
#14241=EDGE_CURVE('',#11555,#11556,#1106,.T.);
#14242=EDGE_CURVE('',#11556,#11557,#5911,.T.);
#14243=EDGE_CURVE('',#11557,#11557,#10771,.T.);
#14244=EDGE_CURVE('',#11556,#11558,#1107,.T.);
#14245=EDGE_CURVE('',#11558,#11555,#1108,.T.);
#14246=EDGE_CURVE('',#11559,#11559,#1109,.T.);
#14247=EDGE_CURVE('',#11560,#11560,#1110,.T.);
#14248=EDGE_CURVE('',#11561,#11561,#1111,.T.);
#14249=EDGE_CURVE('',#11562,#11562,#1112,.T.);
#14250=EDGE_CURVE('',#11563,#11563,#1113,.T.);
#14251=EDGE_CURVE('',#11564,#11552,#5912,.T.);
#14252=EDGE_CURVE('',#11564,#11565,#1114,.T.);
#14253=EDGE_CURVE('',#11565,#11566,#1115,.T.);
#14254=EDGE_CURVE('',#11566,#11564,#1116,.T.);
#14255=EDGE_CURVE('',#11567,#11567,#10772,.T.);
#14256=EDGE_CURVE('',#11567,#11568,#5913,.T.);
#14257=EDGE_CURVE('',#11568,#11568,#10773,.T.);
#14258=EDGE_CURVE('',#11569,#11569,#10774,.T.);
#14259=EDGE_CURVE('',#11570,#11569,#10775,.T.);
#14260=EDGE_CURVE('',#11571,#11570,#1117,.T.);
#14261=EDGE_CURVE('',#11572,#11571,#10776,.T.);
#14262=EDGE_CURVE('',#11573,#11572,#1118,.T.);
#14263=EDGE_CURVE('',#11574,#11573,#10777,.T.);
#14264=EDGE_CURVE('',#11575,#11574,#1119,.T.);
#14265=EDGE_CURVE('',#11576,#11575,#10778,.T.);
#14266=EDGE_CURVE('',#11577,#11576,#1120,.T.);
#14267=EDGE_CURVE('',#11578,#11577,#10779,.T.);
#14268=EDGE_CURVE('',#11579,#11578,#1121,.T.);
#14269=EDGE_CURVE('',#11580,#11579,#10780,.T.);
#14270=EDGE_CURVE('',#11581,#11580,#1122,.T.);
#14271=EDGE_CURVE('',#11569,#11581,#10781,.T.);
#14272=EDGE_CURVE('',#11582,#11581,#1123,.T.);
#14273=EDGE_CURVE('',#11580,#11582,#1124,.T.);
#14274=EDGE_CURVE('',#11583,#11579,#1125,.T.);
#14275=EDGE_CURVE('',#11578,#11583,#1126,.T.);
#14276=EDGE_CURVE('',#11584,#11577,#1127,.T.);
#14277=EDGE_CURVE('',#11576,#11584,#1128,.T.);
#14278=EDGE_CURVE('',#11585,#11575,#1129,.T.);
#14279=EDGE_CURVE('',#11574,#11585,#1130,.T.);
#14280=EDGE_CURVE('',#11586,#11573,#1131,.T.);
#14281=EDGE_CURVE('',#11572,#11586,#1132,.T.);
#14282=EDGE_CURVE('',#11587,#11571,#1133,.T.);
#14283=EDGE_CURVE('',#11570,#11587,#1134,.T.);
#14284=EDGE_CURVE('',#11563,#11576,#5914,.T.);
#14285=EDGE_CURVE('',#11562,#11574,#5915,.T.);
#14286=EDGE_CURVE('',#11558,#11572,#5916,.T.);
#14287=EDGE_CURVE('',#11561,#11570,#5917,.T.);
#14288=EDGE_CURVE('',#11560,#11580,#5918,.T.);
#14289=EDGE_CURVE('',#11559,#11578,#5919,.T.);
#14290=EDGE_CURVE('',#11568,#11588,#5920,.T.);
#14291=EDGE_CURVE('',#11588,#11588,#10782,.T.);
#14292=EDGE_CURVE('',#11589,#11589,#10783,.T.);
#14293=EDGE_CURVE('',#11557,#11589,#5921,.T.);
#14294=EDGE_CURVE('',#11590,#11590,#10784,.T.);
#14295=EDGE_CURVE('',#11590,#11554,#5922,.T.);
#14296=EDGE_CURVE('',#11591,#11591,#10785,.T.);
#14297=EDGE_CURVE('',#11591,#11567,#5923,.T.);
#14298=EDGE_CURVE('',#11592,#11593,#5924,.T.);
#14299=EDGE_CURVE('',#11592,#11594,#1135,.T.);
#14300=EDGE_CURVE('',#11594,#11595,#10786,.T.);
#14301=EDGE_CURVE('',#11595,#11593,#1136,.T.);
#14302=EDGE_CURVE('',#11596,#11597,#5925,.T.);
#14303=EDGE_CURVE('',#11596,#11592,#1137,.T.);
#14304=EDGE_CURVE('',#11593,#11597,#1138,.T.);
#14305=EDGE_CURVE('',#11598,#11599,#5926,.T.);
#14306=EDGE_CURVE('',#11598,#11596,#1139,.T.);
#14307=EDGE_CURVE('',#11597,#11599,#1140,.T.);
#14308=EDGE_CURVE('',#11600,#11601,#5927,.T.);
#14309=EDGE_CURVE('',#11600,#11598,#1141,.T.);
#14310=EDGE_CURVE('',#11599,#11601,#1142,.T.);
#14311=EDGE_CURVE('',#11602,#11603,#5928,.T.);
#14312=EDGE_CURVE('',#11602,#11600,#1143,.T.);
#14313=EDGE_CURVE('',#11601,#11603,#1144,.T.);
#14314=EDGE_CURVE('',#11604,#11605,#5929,.T.);
#14315=EDGE_CURVE('',#11604,#11602,#1145,.T.);
#14316=EDGE_CURVE('',#11603,#11605,#1146,.T.);
#14317=EDGE_CURVE('',#11606,#11607,#5930,.T.);
#14318=EDGE_CURVE('',#11606,#11604,#1147,.T.);
#14319=EDGE_CURVE('',#11605,#11607,#1148,.T.);
#14320=EDGE_CURVE('',#11608,#11609,#5931,.T.);
#14321=EDGE_CURVE('',#11608,#11610,#1149,.T.);
#14322=EDGE_CURVE('',#11609,#11610,#10787,.T.);
#14323=EDGE_CURVE('',#11611,#11612,#5932,.T.);
#14324=EDGE_CURVE('',#11611,#11608,#1150,.T.);
#14325=EDGE_CURVE('',#11613,#11609,#10788,.T.);
#14326=EDGE_CURVE('',#11612,#11613,#1151,.T.);
#14327=EDGE_CURVE('',#11614,#11615,#5933,.T.);
#14328=EDGE_CURVE('',#11614,#11611,#1152,.T.);
#14329=EDGE_CURVE('',#11615,#11612,#1153,.T.);
#14330=EDGE_CURVE('',#11616,#11617,#5934,.T.);
#14331=EDGE_CURVE('',#11616,#11614,#1154,.T.);
#14332=EDGE_CURVE('',#11617,#11615,#1155,.T.);
#14333=EDGE_CURVE('',#11618,#11619,#5935,.T.);
#14334=EDGE_CURVE('',#11618,#11616,#1156,.T.);
#14335=EDGE_CURVE('',#11619,#11617,#1157,.T.);
#14336=EDGE_CURVE('',#11620,#11621,#5936,.T.);
#14337=EDGE_CURVE('',#11620,#11618,#1158,.T.);
#14338=EDGE_CURVE('',#11621,#11619,#1159,.T.);
#14339=EDGE_CURVE('',#11622,#11623,#5937,.T.);
#14340=EDGE_CURVE('',#11622,#11620,#1160,.T.);
#14341=EDGE_CURVE('',#11623,#11621,#1161,.T.);
#14342=EDGE_CURVE('',#11610,#11624,#1162,.T.);
#14343=EDGE_CURVE('',#11625,#11624,#10789,.F.);
#14344=EDGE_CURVE('',#11626,#11625,#10790,.F.);
#14345=EDGE_CURVE('',#11626,#11613,#1163,.T.);
#14346=EDGE_CURVE('',#11607,#11626,#1164,.T.);
#14347=EDGE_CURVE('',#11627,#11595,#1165,.T.);
#14348=EDGE_CURVE('',#11627,#11623,#1166,.T.);
#14349=EDGE_CURVE('',#11595,#11628,#10791,.T.);
#14350=EDGE_CURVE('',#11628,#11594,#10792,.T.);
#14351=EDGE_CURVE('',#11594,#11629,#1167,.T.);
#14352=EDGE_CURVE('',#11629,#11627,#10793,.T.);
#14353=EDGE_CURVE('',#11629,#11622,#1168,.T.);
#14354=EDGE_CURVE('',#11624,#11606,#1169,.T.);
#14355=EDGE_CURVE('',#11630,#11631,#5938,.T.);
#14356=EDGE_CURVE('',#11631,#11630,#10794,.T.);
#14357=EDGE_CURVE('',#11631,#11632,#5939,.T.);
#14358=EDGE_CURVE('',#11632,#11631,#10795,.T.);
#14359=EDGE_CURVE('',#11632,#11633,#5940,.T.);
#14360=EDGE_CURVE('',#11633,#11632,#10796,.T.);
#14361=EDGE_CURVE('',#11633,#11634,#5941,.T.);
#14362=EDGE_CURVE('',#11634,#11633,#10797,.T.);
#14363=EDGE_CURVE('',#11634,#11635,#5942,.T.);
#14364=EDGE_CURVE('',#11635,#11634,#10798,.T.);
#14365=EDGE_CURVE('',#11635,#11630,#5943,.T.);
#14366=EDGE_CURVE('',#11630,#11635,#10799,.T.);
#14367=EDGE_CURVE('',#11636,#11637,#5944,.T.);
#14368=EDGE_CURVE('',#11638,#11637,#10800,.T.);
#14369=EDGE_CURVE('',#11632,#11638,#203,.T.);
#14370=EDGE_CURVE('',#11639,#11631,#204,.T.);
#14371=EDGE_CURVE('',#11640,#11639,#10801,.T.);
#14372=EDGE_CURVE('',#11631,#11640,#205,.T.);
#14373=EDGE_CURVE('',#11641,#11630,#206,.T.);
#14374=EDGE_CURVE('',#11642,#11641,#10802,.T.);
#14375=EDGE_CURVE('',#11630,#11642,#207,.T.);
#14376=EDGE_CURVE('',#11643,#11635,#208,.T.);
#14377=EDGE_CURVE('',#11644,#11643,#10803,.T.);
#14378=EDGE_CURVE('',#11635,#11644,#209,.T.);
#14379=EDGE_CURVE('',#11645,#11634,#210,.T.);
#14380=EDGE_CURVE('',#11646,#11645,#10804,.T.);
#14381=EDGE_CURVE('',#11634,#11646,#211,.T.);
#14382=EDGE_CURVE('',#11647,#11633,#212,.T.);
#14383=EDGE_CURVE('',#11648,#11647,#10805,.T.);
#14384=EDGE_CURVE('',#11633,#11648,#213,.T.);
#14385=EDGE_CURVE('',#11649,#11632,#214,.T.);
#14386=EDGE_CURVE('',#11637,#11649,#10806,.T.);
#14387=EDGE_CURVE('',#11650,#11633,#5945,.T.);
#14388=EDGE_CURVE('',#11651,#11650,#5946,.T.);
#14389=EDGE_CURVE('',#11651,#11632,#5947,.T.);
#14390=EDGE_CURVE('',#11632,#11652,#5948,.T.);
#14391=EDGE_CURVE('',#11652,#11649,#5949,.T.);
#14392=EDGE_CURVE('',#11653,#11634,#5950,.T.);
#14393=EDGE_CURVE('',#11650,#11653,#5951,.T.);
#14394=EDGE_CURVE('',#11646,#11654,#5952,.T.);
#14395=EDGE_CURVE('',#11634,#11654,#5953,.T.);
#14396=EDGE_CURVE('',#11633,#11655,#5954,.T.);
#14397=EDGE_CURVE('',#11655,#11647,#5955,.T.);
#14398=EDGE_CURVE('',#11656,#11651,#5956,.T.);
#14399=EDGE_CURVE('',#11656,#11631,#5957,.T.);
#14400=EDGE_CURVE('',#11631,#11657,#5958,.T.);
#14401=EDGE_CURVE('',#11657,#11639,#5959,.T.);
#14402=EDGE_CURVE('',#11658,#11635,#5960,.T.);
#14403=EDGE_CURVE('',#11653,#11658,#5961,.T.);
#14404=EDGE_CURVE('',#11644,#11659,#5962,.T.);
#14405=EDGE_CURVE('',#11635,#11659,#5963,.T.);
#14406=EDGE_CURVE('',#11654,#11645,#5964,.T.);
#14407=EDGE_CURVE('',#11648,#11655,#5965,.T.);
#14408=EDGE_CURVE('',#11659,#11643,#5966,.T.);
#14409=EDGE_CURVE('',#11660,#11641,#5967,.T.);
#14410=EDGE_CURVE('',#11642,#11660,#5968,.T.);
#14411=EDGE_CURVE('',#11640,#11657,#5969,.T.);
#14412=EDGE_CURVE('',#11638,#11652,#5970,.T.);
#14413=EDGE_CURVE('',#11661,#11630,#5971,.T.);
#14414=EDGE_CURVE('',#11658,#11661,#5972,.T.);
#14415=EDGE_CURVE('',#11630,#11660,#5973,.T.);
#14416=EDGE_CURVE('',#11661,#11656,#5974,.T.);
#14417=EDGE_CURVE('',#11662,#11662,#10807,.T.);
#14418=EDGE_CURVE('',#11628,#11662,#5975,.T.);
#14419=EDGE_CURVE('',#11624,#11626,#10808,.F.);
#14420=EDGE_CURVE('',#11663,#11663,#10809,.T.);
#14421=EDGE_CURVE('',#11663,#11625,#5976,.T.);
#14422=EDGE_CURVE('',#11664,#11665,#5977,.T.);
#14423=EDGE_CURVE('',#11664,#11666,#5978,.T.);
#14424=EDGE_CURVE('',#11666,#11667,#5979,.T.);
#14425=EDGE_CURVE('',#11665,#11667,#5980,.T.);
#14426=EDGE_CURVE('',#11668,#11664,#5981,.T.);
#14427=EDGE_CURVE('',#11668,#11669,#5982,.T.);
#14428=EDGE_CURVE('',#11669,#11666,#5983,.T.);
#14429=EDGE_CURVE('',#11670,#11668,#5984,.T.);
#14430=EDGE_CURVE('',#11670,#11671,#5985,.T.);
#14431=EDGE_CURVE('',#11671,#11669,#5986,.T.);
#14432=EDGE_CURVE('',#11665,#11670,#5987,.T.);
#14433=EDGE_CURVE('',#11667,#11671,#5988,.T.);
#14434=EDGE_CURVE('',#11672,#11673,#5989,.T.);
#14435=EDGE_CURVE('',#11672,#11674,#5990,.T.);
#14436=EDGE_CURVE('',#11674,#11675,#5991,.T.);
#14437=EDGE_CURVE('',#11673,#11675,#5992,.T.);
#14438=EDGE_CURVE('',#11676,#11672,#5993,.T.);
#14439=EDGE_CURVE('',#11676,#11677,#5994,.T.);
#14440=EDGE_CURVE('',#11677,#11674,#5995,.T.);
#14441=EDGE_CURVE('',#11678,#11676,#5996,.T.);
#14442=EDGE_CURVE('',#11678,#11679,#5997,.T.);
#14443=EDGE_CURVE('',#11679,#11677,#5998,.T.);
#14444=EDGE_CURVE('',#11673,#11678,#5999,.T.);
#14445=EDGE_CURVE('',#11675,#11679,#6000,.T.);
#14446=EDGE_CURVE('',#11680,#11681,#6001,.T.);
#14447=EDGE_CURVE('',#11682,#11680,#6002,.T.);
#14448=EDGE_CURVE('',#11681,#11682,#6003,.T.);
#14449=EDGE_CURVE('',#11683,#11684,#6004,.T.);
#14450=EDGE_CURVE('',#11685,#11683,#6005,.T.);
#14451=EDGE_CURVE('',#11684,#11685,#6006,.T.);
#14452=EDGE_CURVE('',#11686,#11687,#6007,.T.);
#14453=EDGE_CURVE('',#11688,#11686,#6008,.T.);
#14454=EDGE_CURVE('',#11687,#11688,#6009,.T.);
#14455=EDGE_CURVE('',#11689,#11690,#6010,.T.);
#14456=EDGE_CURVE('',#11691,#11689,#6011,.T.);
#14457=EDGE_CURVE('',#11690,#11691,#6012,.T.);
#14458=EDGE_CURVE('',#11692,#11693,#6013,.T.);
#14459=EDGE_CURVE('',#11694,#11692,#6014,.T.);
#14460=EDGE_CURVE('',#11693,#11694,#6015,.T.);
#14461=EDGE_CURVE('',#11692,#11687,#6016,.T.);
#14462=EDGE_CURVE('',#11688,#11694,#6017,.T.);
#14463=EDGE_CURVE('',#11695,#11696,#6018,.T.);
#14464=EDGE_CURVE('',#11697,#11695,#6019,.T.);
#14465=EDGE_CURVE('',#11696,#11697,#6020,.T.);
#14466=EDGE_CURVE('',#11698,#11699,#6021,.T.);
#14467=EDGE_CURVE('',#11700,#11698,#6022,.T.);
#14468=EDGE_CURVE('',#11699,#11700,#6023,.T.);
#14469=EDGE_CURVE('',#11686,#11700,#6024,.T.);
#14470=EDGE_CURVE('',#11698,#11688,#6025,.T.);
#14471=EDGE_CURVE('',#11689,#11699,#6026,.T.);
#14472=EDGE_CURVE('',#11700,#11691,#6027,.T.);
#14473=EDGE_CURVE('',#11701,#11702,#6028,.T.);
#14474=EDGE_CURVE('',#11703,#11701,#6029,.T.);
#14475=EDGE_CURVE('',#11702,#11703,#6030,.T.);
#14476=EDGE_CURVE('',#11701,#11693,#6031,.T.);
#14477=EDGE_CURVE('',#11694,#11703,#6032,.T.);
#14478=EDGE_CURVE('',#11699,#11702,#6033,.T.);
#14479=EDGE_CURVE('',#11703,#11698,#6034,.T.);
#14480=EDGE_CURVE('',#11695,#11701,#6035,.T.);
#14481=EDGE_CURVE('',#11702,#11697,#6036,.T.);
#14482=EDGE_CURVE('',#11690,#11696,#6037,.T.);
#14483=EDGE_CURVE('',#11697,#11689,#6038,.T.);
#14484=EDGE_CURVE('',#11696,#11684,#6039,.T.);
#14485=EDGE_CURVE('',#11685,#11695,#6040,.T.);
#14486=EDGE_CURVE('',#11683,#11692,#6041,.T.);
#14487=EDGE_CURVE('',#11693,#11685,#6042,.T.);
#14488=EDGE_CURVE('',#11681,#11690,#6043,.T.);
#14489=EDGE_CURVE('',#11691,#11680,#6044,.T.);
#14490=EDGE_CURVE('',#11680,#11686,#6045,.T.);
#14491=EDGE_CURVE('',#11687,#11682,#6046,.T.);
#14492=EDGE_CURVE('',#11684,#11681,#6047,.T.);
#14493=EDGE_CURVE('',#11682,#11683,#6048,.T.);
#14494=EDGE_CURVE('',#11704,#11705,#6049,.T.);
#14495=EDGE_CURVE('',#11704,#11706,#1170,.T.);
#14496=EDGE_CURVE('',#11706,#11707,#10810,.T.);
#14497=EDGE_CURVE('',#11707,#11705,#1171,.T.);
#14498=EDGE_CURVE('',#11708,#11709,#6050,.T.);
#14499=EDGE_CURVE('',#11708,#11704,#1172,.T.);
#14500=EDGE_CURVE('',#11705,#11709,#1173,.T.);
#14501=EDGE_CURVE('',#11710,#11711,#6051,.T.);
#14502=EDGE_CURVE('',#11710,#11708,#1174,.T.);
#14503=EDGE_CURVE('',#11709,#11711,#1175,.T.);
#14504=EDGE_CURVE('',#11712,#11713,#6052,.T.);
#14505=EDGE_CURVE('',#11712,#11710,#1176,.T.);
#14506=EDGE_CURVE('',#11711,#11713,#1177,.T.);
#14507=EDGE_CURVE('',#11714,#11715,#6053,.T.);
#14508=EDGE_CURVE('',#11714,#11712,#1178,.T.);
#14509=EDGE_CURVE('',#11713,#11715,#1179,.T.);
#14510=EDGE_CURVE('',#11716,#11717,#6054,.T.);
#14511=EDGE_CURVE('',#11716,#11714,#1180,.T.);
#14512=EDGE_CURVE('',#11715,#11717,#1181,.T.);
#14513=EDGE_CURVE('',#11718,#11719,#6055,.T.);
#14514=EDGE_CURVE('',#11718,#11716,#1182,.T.);
#14515=EDGE_CURVE('',#11717,#11719,#1183,.T.);
#14516=EDGE_CURVE('',#11720,#11721,#6056,.T.);
#14517=EDGE_CURVE('',#11720,#11718,#1184,.T.);
#14518=EDGE_CURVE('',#11719,#11721,#1185,.T.);
#14519=EDGE_CURVE('',#11722,#11723,#6057,.T.);
#14520=EDGE_CURVE('',#11722,#11720,#1186,.T.);
#14521=EDGE_CURVE('',#11721,#11723,#1187,.T.);
#14522=EDGE_CURVE('',#11724,#11725,#6058,.T.);
#14523=EDGE_CURVE('',#11724,#11722,#1188,.T.);
#14524=EDGE_CURVE('',#11723,#11725,#1189,.T.);
#14525=EDGE_CURVE('',#11726,#11727,#6059,.T.);
#14526=EDGE_CURVE('',#11726,#11724,#1190,.T.);
#14527=EDGE_CURVE('',#11725,#11727,#1191,.T.);
#14528=EDGE_CURVE('',#11728,#11729,#6060,.T.);
#14529=EDGE_CURVE('',#11728,#11726,#1192,.T.);
#14530=EDGE_CURVE('',#11727,#11729,#1193,.T.);
#14531=EDGE_CURVE('',#11730,#11731,#6061,.T.);
#14532=EDGE_CURVE('',#11730,#11728,#1194,.T.);
#14533=EDGE_CURVE('',#11729,#11731,#1195,.T.);
#14534=EDGE_CURVE('',#11732,#11733,#6062,.T.);
#14535=EDGE_CURVE('',#11732,#11730,#1196,.T.);
#14536=EDGE_CURVE('',#11731,#11733,#1197,.T.);
#14537=EDGE_CURVE('',#11734,#11735,#6063,.T.);
#14538=EDGE_CURVE('',#11734,#11732,#1198,.T.);
#14539=EDGE_CURVE('',#11733,#11735,#1199,.T.);
#14540=EDGE_CURVE('',#11736,#11737,#6064,.T.);
#14541=EDGE_CURVE('',#11736,#11734,#1200,.T.);
#14542=EDGE_CURVE('',#11735,#11737,#1201,.T.);
#14543=EDGE_CURVE('',#11738,#11739,#6065,.T.);
#14544=EDGE_CURVE('',#11738,#11736,#1202,.T.);
#14545=EDGE_CURVE('',#11737,#11739,#1203,.T.);
#14546=EDGE_CURVE('',#11740,#11741,#6066,.T.);
#14547=EDGE_CURVE('',#11740,#11738,#1204,.T.);
#14548=EDGE_CURVE('',#11739,#11741,#1205,.T.);
#14549=EDGE_CURVE('',#11742,#11743,#6067,.T.);
#14550=EDGE_CURVE('',#11742,#11740,#1206,.T.);
#14551=EDGE_CURVE('',#11741,#11743,#1207,.T.);
#14552=EDGE_CURVE('',#11744,#11745,#6068,.T.);
#14553=EDGE_CURVE('',#11744,#11742,#1208,.T.);
#14554=EDGE_CURVE('',#11743,#11745,#1209,.T.);
#14555=EDGE_CURVE('',#11746,#11747,#6069,.T.);
#14556=EDGE_CURVE('',#11746,#11744,#1210,.T.);
#14557=EDGE_CURVE('',#11745,#11747,#1211,.T.);
#14558=EDGE_CURVE('',#11748,#11749,#6070,.T.);
#14559=EDGE_CURVE('',#11748,#11746,#1212,.T.);
#14560=EDGE_CURVE('',#11747,#11749,#1213,.T.);
#14561=EDGE_CURVE('',#11750,#11751,#6071,.T.);
#14562=EDGE_CURVE('',#11750,#11748,#1214,.T.);
#14563=EDGE_CURVE('',#11749,#11751,#1215,.T.);
#14564=EDGE_CURVE('',#11752,#11753,#6072,.T.);
#14565=EDGE_CURVE('',#11752,#11750,#1216,.T.);
#14566=EDGE_CURVE('',#11751,#11753,#1217,.T.);
#14567=EDGE_CURVE('',#11754,#11755,#6073,.T.);
#14568=EDGE_CURVE('',#11754,#11752,#1218,.T.);
#14569=EDGE_CURVE('',#11753,#11755,#1219,.T.);
#14570=EDGE_CURVE('',#11756,#11757,#6074,.T.);
#14571=EDGE_CURVE('',#11756,#11754,#1220,.T.);
#14572=EDGE_CURVE('',#11755,#11757,#1221,.T.);
#14573=EDGE_CURVE('',#11758,#11759,#6075,.T.);
#14574=EDGE_CURVE('',#11758,#11756,#1222,.T.);
#14575=EDGE_CURVE('',#11757,#11759,#1223,.T.);
#14576=EDGE_CURVE('',#11760,#11761,#6076,.T.);
#14577=EDGE_CURVE('',#11760,#11758,#1224,.T.);
#14578=EDGE_CURVE('',#11759,#11761,#1225,.T.);
#14579=EDGE_CURVE('',#11762,#11763,#6077,.T.);
#14580=EDGE_CURVE('',#11762,#11760,#1226,.T.);
#14581=EDGE_CURVE('',#11761,#11763,#1227,.T.);
#14582=EDGE_CURVE('',#11764,#11765,#6078,.T.);
#14583=EDGE_CURVE('',#11764,#11766,#1228,.T.);
#14584=EDGE_CURVE('',#11765,#11766,#10811,.T.);
#14585=EDGE_CURVE('',#11767,#11768,#6079,.T.);
#14586=EDGE_CURVE('',#11767,#11764,#1229,.T.);
#14587=EDGE_CURVE('',#11769,#11765,#10812,.T.);
#14588=EDGE_CURVE('',#11768,#11769,#1230,.T.);
#14589=EDGE_CURVE('',#11770,#11771,#6080,.T.);
#14590=EDGE_CURVE('',#11770,#11767,#1231,.T.);
#14591=EDGE_CURVE('',#11771,#11768,#1232,.T.);
#14592=EDGE_CURVE('',#11772,#11773,#6081,.T.);
#14593=EDGE_CURVE('',#11772,#11770,#1233,.T.);
#14594=EDGE_CURVE('',#11773,#11771,#1234,.T.);
#14595=EDGE_CURVE('',#11774,#11775,#6082,.T.);
#14596=EDGE_CURVE('',#11774,#11772,#1235,.T.);
#14597=EDGE_CURVE('',#11775,#11773,#1236,.T.);
#14598=EDGE_CURVE('',#11776,#11777,#6083,.T.);
#14599=EDGE_CURVE('',#11776,#11774,#1237,.T.);
#14600=EDGE_CURVE('',#11777,#11775,#1238,.T.);
#14601=EDGE_CURVE('',#11778,#11779,#6084,.T.);
#14602=EDGE_CURVE('',#11778,#11776,#1239,.T.);
#14603=EDGE_CURVE('',#11779,#11777,#1240,.T.);
#14604=EDGE_CURVE('',#11780,#11781,#6085,.T.);
#14605=EDGE_CURVE('',#11780,#11778,#1241,.T.);
#14606=EDGE_CURVE('',#11781,#11779,#1242,.T.);
#14607=EDGE_CURVE('',#11782,#11783,#6086,.T.);
#14608=EDGE_CURVE('',#11782,#11780,#1243,.T.);
#14609=EDGE_CURVE('',#11783,#11781,#1244,.T.);
#14610=EDGE_CURVE('',#11784,#11785,#6087,.T.);
#14611=EDGE_CURVE('',#11784,#11782,#1245,.T.);
#14612=EDGE_CURVE('',#11785,#11783,#1246,.T.);
#14613=EDGE_CURVE('',#11786,#11787,#6088,.T.);
#14614=EDGE_CURVE('',#11786,#11784,#1247,.T.);
#14615=EDGE_CURVE('',#11787,#11785,#1248,.T.);
#14616=EDGE_CURVE('',#11788,#11789,#6089,.T.);
#14617=EDGE_CURVE('',#11788,#11786,#1249,.T.);
#14618=EDGE_CURVE('',#11789,#11787,#1250,.T.);
#14619=EDGE_CURVE('',#11790,#11791,#6090,.T.);
#14620=EDGE_CURVE('',#11790,#11788,#1251,.T.);
#14621=EDGE_CURVE('',#11791,#11789,#1252,.T.);
#14622=EDGE_CURVE('',#11792,#11793,#6091,.T.);
#14623=EDGE_CURVE('',#11792,#11790,#1253,.T.);
#14624=EDGE_CURVE('',#11793,#11791,#1254,.T.);
#14625=EDGE_CURVE('',#11794,#11795,#6092,.T.);
#14626=EDGE_CURVE('',#11794,#11792,#1255,.T.);
#14627=EDGE_CURVE('',#11795,#11793,#1256,.T.);
#14628=EDGE_CURVE('',#11796,#11797,#6093,.T.);
#14629=EDGE_CURVE('',#11796,#11794,#1257,.T.);
#14630=EDGE_CURVE('',#11797,#11795,#1258,.T.);
#14631=EDGE_CURVE('',#11798,#11799,#6094,.T.);
#14632=EDGE_CURVE('',#11798,#11796,#1259,.T.);
#14633=EDGE_CURVE('',#11799,#11797,#1260,.T.);
#14634=EDGE_CURVE('',#11800,#11801,#6095,.T.);
#14635=EDGE_CURVE('',#11800,#11798,#1261,.T.);
#14636=EDGE_CURVE('',#11801,#11799,#1262,.T.);
#14637=EDGE_CURVE('',#11802,#11803,#6096,.T.);
#14638=EDGE_CURVE('',#11802,#11800,#1263,.T.);
#14639=EDGE_CURVE('',#11803,#11801,#1264,.T.);
#14640=EDGE_CURVE('',#11804,#11805,#6097,.T.);
#14641=EDGE_CURVE('',#11804,#11802,#1265,.T.);
#14642=EDGE_CURVE('',#11805,#11803,#1266,.T.);
#14643=EDGE_CURVE('',#11806,#11807,#6098,.T.);
#14644=EDGE_CURVE('',#11806,#11804,#1267,.T.);
#14645=EDGE_CURVE('',#11807,#11805,#1268,.T.);
#14646=EDGE_CURVE('',#11808,#11809,#6099,.T.);
#14647=EDGE_CURVE('',#11808,#11806,#1269,.T.);
#14648=EDGE_CURVE('',#11809,#11807,#1270,.T.);
#14649=EDGE_CURVE('',#11810,#11811,#6100,.T.);
#14650=EDGE_CURVE('',#11810,#11808,#1271,.T.);
#14651=EDGE_CURVE('',#11811,#11809,#1272,.T.);
#14652=EDGE_CURVE('',#11812,#11813,#6101,.T.);
#14653=EDGE_CURVE('',#11812,#11810,#1273,.T.);
#14654=EDGE_CURVE('',#11813,#11811,#1274,.T.);
#14655=EDGE_CURVE('',#11814,#11815,#6102,.T.);
#14656=EDGE_CURVE('',#11814,#11812,#1275,.T.);
#14657=EDGE_CURVE('',#11815,#11813,#1276,.T.);
#14658=EDGE_CURVE('',#11816,#11817,#6103,.T.);
#14659=EDGE_CURVE('',#11816,#11814,#1277,.T.);
#14660=EDGE_CURVE('',#11817,#11815,#1278,.T.);
#14661=EDGE_CURVE('',#11818,#11819,#6104,.T.);
#14662=EDGE_CURVE('',#11818,#11816,#1279,.T.);
#14663=EDGE_CURVE('',#11819,#11817,#1280,.T.);
#14664=EDGE_CURVE('',#11820,#11821,#6105,.T.);
#14665=EDGE_CURVE('',#11820,#11818,#1281,.T.);
#14666=EDGE_CURVE('',#11821,#11819,#1282,.T.);
#14667=EDGE_CURVE('',#11822,#11823,#6106,.T.);
#14668=EDGE_CURVE('',#11822,#11820,#1283,.T.);
#14669=EDGE_CURVE('',#11823,#11821,#1284,.T.);
#14670=EDGE_CURVE('',#11766,#11824,#1285,.T.);
#14671=EDGE_CURVE('',#11825,#11824,#10813,.F.);
#14672=EDGE_CURVE('',#11826,#11825,#10814,.F.);
#14673=EDGE_CURVE('',#11826,#11769,#1286,.T.);
#14674=EDGE_CURVE('',#11763,#11826,#1287,.T.);
#14675=EDGE_CURVE('',#11827,#11707,#1288,.T.);
#14676=EDGE_CURVE('',#11827,#11823,#1289,.T.);
#14677=EDGE_CURVE('',#11707,#11828,#10815,.T.);
#14678=EDGE_CURVE('',#11828,#11706,#10816,.T.);
#14679=EDGE_CURVE('',#11706,#11829,#1290,.T.);
#14680=EDGE_CURVE('',#11829,#11827,#10817,.T.);
#14681=EDGE_CURVE('',#11829,#11822,#1291,.T.);
#14682=EDGE_CURVE('',#11824,#11762,#1292,.T.);
#14683=EDGE_CURVE('',#11830,#11831,#6107,.T.);
#14684=EDGE_CURVE('',#11831,#11830,#10818,.T.);
#14685=EDGE_CURVE('',#11831,#11832,#6108,.T.);
#14686=EDGE_CURVE('',#11832,#11831,#10819,.T.);
#14687=EDGE_CURVE('',#11832,#11833,#6109,.T.);
#14688=EDGE_CURVE('',#11833,#11832,#10820,.T.);
#14689=EDGE_CURVE('',#11833,#11834,#6110,.T.);
#14690=EDGE_CURVE('',#11834,#11833,#10821,.T.);
#14691=EDGE_CURVE('',#11834,#11835,#6111,.T.);
#14692=EDGE_CURVE('',#11835,#11834,#10822,.T.);
#14693=EDGE_CURVE('',#11835,#11830,#6112,.T.);
#14694=EDGE_CURVE('',#11830,#11835,#10823,.T.);
#14695=EDGE_CURVE('',#11836,#11837,#6113,.T.);
#14696=EDGE_CURVE('',#11838,#11837,#10824,.T.);
#14697=EDGE_CURVE('',#11832,#11838,#215,.T.);
#14698=EDGE_CURVE('',#11839,#11831,#216,.T.);
#14699=EDGE_CURVE('',#11840,#11839,#10825,.T.);
#14700=EDGE_CURVE('',#11831,#11840,#217,.T.);
#14701=EDGE_CURVE('',#11841,#11830,#218,.T.);
#14702=EDGE_CURVE('',#11842,#11841,#10826,.T.);
#14703=EDGE_CURVE('',#11830,#11842,#219,.T.);
#14704=EDGE_CURVE('',#11843,#11835,#220,.T.);
#14705=EDGE_CURVE('',#11844,#11843,#10827,.T.);
#14706=EDGE_CURVE('',#11835,#11844,#221,.T.);
#14707=EDGE_CURVE('',#11845,#11834,#222,.T.);
#14708=EDGE_CURVE('',#11846,#11845,#10828,.T.);
#14709=EDGE_CURVE('',#11834,#11846,#223,.T.);
#14710=EDGE_CURVE('',#11847,#11833,#224,.T.);
#14711=EDGE_CURVE('',#11848,#11847,#10829,.T.);
#14712=EDGE_CURVE('',#11833,#11848,#225,.T.);
#14713=EDGE_CURVE('',#11849,#11832,#226,.T.);
#14714=EDGE_CURVE('',#11837,#11849,#10830,.T.);
#14715=EDGE_CURVE('',#11850,#11833,#6114,.T.);
#14716=EDGE_CURVE('',#11851,#11850,#6115,.T.);
#14717=EDGE_CURVE('',#11851,#11832,#6116,.T.);
#14718=EDGE_CURVE('',#11832,#11852,#6117,.T.);
#14719=EDGE_CURVE('',#11852,#11849,#6118,.T.);
#14720=EDGE_CURVE('',#11853,#11834,#6119,.T.);
#14721=EDGE_CURVE('',#11850,#11853,#6120,.T.);
#14722=EDGE_CURVE('',#11846,#11854,#6121,.T.);
#14723=EDGE_CURVE('',#11834,#11854,#6122,.T.);
#14724=EDGE_CURVE('',#11833,#11855,#6123,.T.);
#14725=EDGE_CURVE('',#11855,#11847,#6124,.T.);
#14726=EDGE_CURVE('',#11856,#11851,#6125,.T.);
#14727=EDGE_CURVE('',#11856,#11831,#6126,.T.);
#14728=EDGE_CURVE('',#11831,#11857,#6127,.T.);
#14729=EDGE_CURVE('',#11857,#11839,#6128,.T.);
#14730=EDGE_CURVE('',#11858,#11835,#6129,.T.);
#14731=EDGE_CURVE('',#11853,#11858,#6130,.T.);
#14732=EDGE_CURVE('',#11844,#11859,#6131,.T.);
#14733=EDGE_CURVE('',#11835,#11859,#6132,.T.);
#14734=EDGE_CURVE('',#11854,#11845,#6133,.T.);
#14735=EDGE_CURVE('',#11848,#11855,#6134,.T.);
#14736=EDGE_CURVE('',#11859,#11843,#6135,.T.);
#14737=EDGE_CURVE('',#11860,#11841,#6136,.T.);
#14738=EDGE_CURVE('',#11842,#11860,#6137,.T.);
#14739=EDGE_CURVE('',#11840,#11857,#6138,.T.);
#14740=EDGE_CURVE('',#11838,#11852,#6139,.T.);
#14741=EDGE_CURVE('',#11861,#11830,#6140,.T.);
#14742=EDGE_CURVE('',#11858,#11861,#6141,.T.);
#14743=EDGE_CURVE('',#11830,#11860,#6142,.T.);
#14744=EDGE_CURVE('',#11861,#11856,#6143,.T.);
#14745=EDGE_CURVE('',#11862,#11862,#10831,.T.);
#14746=EDGE_CURVE('',#11828,#11862,#6144,.T.);
#14747=EDGE_CURVE('',#11824,#11826,#10832,.F.);
#14748=EDGE_CURVE('',#11863,#11863,#10833,.T.);
#14749=EDGE_CURVE('',#11863,#11825,#6145,.T.);
#14750=EDGE_CURVE('',#11864,#11864,#10834,.T.);
#14751=EDGE_CURVE('',#11864,#11865,#6146,.T.);
#14752=EDGE_CURVE('',#11865,#11865,#10835,.T.);
#14753=EDGE_CURVE('',#11866,#11866,#10836,.T.);
#14754=EDGE_CURVE('',#11866,#11864,#6147,.T.);
#14755=EDGE_CURVE('',#11867,#11867,#10837,.T.);
#14756=EDGE_CURVE('',#11868,#11868,#10838,.T.);
#14757=EDGE_CURVE('',#11868,#11866,#6148,.T.);
#14758=EDGE_CURVE('',#11869,#11869,#10839,.T.);
#14759=EDGE_CURVE('',#11867,#11870,#6149,.T.);
#14760=EDGE_CURVE('',#11871,#11870,#227,.T.);
#14761=EDGE_CURVE('',#11872,#11871,#228,.T.);
#14762=EDGE_CURVE('',#11873,#11872,#229,.T.);
#14763=EDGE_CURVE('',#11874,#11873,#230,.T.);
#14764=EDGE_CURVE('',#11875,#11874,#231,.T.);
#14765=EDGE_CURVE('',#11876,#11875,#232,.T.);
#14766=EDGE_CURVE('',#11870,#11876,#233,.T.);
#14767=EDGE_CURVE('',#11874,#11877,#6150,.T.);
#14768=EDGE_CURVE('',#11877,#11878,#234,.T.);
#14769=EDGE_CURVE('',#11875,#11878,#6151,.T.);
#14770=EDGE_CURVE('',#11873,#11879,#6152,.T.);
#14771=EDGE_CURVE('',#11879,#11877,#235,.T.);
#14772=EDGE_CURVE('',#11872,#11880,#6153,.T.);
#14773=EDGE_CURVE('',#11880,#11879,#236,.T.);
#14774=EDGE_CURVE('',#11881,#11880,#237,.T.);
#14775=EDGE_CURVE('',#11882,#11881,#238,.T.);
#14776=EDGE_CURVE('',#11882,#11869,#6154,.T.);
#14777=EDGE_CURVE('',#11883,#11882,#239,.T.);
#14778=EDGE_CURVE('',#11878,#11883,#240,.T.);
#14779=EDGE_CURVE('',#11871,#11881,#6155,.T.);
#14780=EDGE_CURVE('',#11876,#11883,#6156,.T.);
#14781=EDGE_CURVE('',#11884,#11885,#6157,.T.);
#14782=EDGE_CURVE('',#11884,#11886,#1293,.T.);
#14783=EDGE_CURVE('',#11886,#11887,#10840,.T.);
#14784=EDGE_CURVE('',#11887,#11885,#1294,.T.);
#14785=EDGE_CURVE('',#11888,#11889,#6158,.T.);
#14786=EDGE_CURVE('',#11888,#11884,#1295,.T.);
#14787=EDGE_CURVE('',#11885,#11889,#1296,.T.);
#14788=EDGE_CURVE('',#11890,#11891,#6159,.T.);
#14789=EDGE_CURVE('',#11890,#11888,#1297,.T.);
#14790=EDGE_CURVE('',#11889,#11891,#1298,.T.);
#14791=EDGE_CURVE('',#11892,#11893,#6160,.T.);
#14792=EDGE_CURVE('',#11892,#11890,#1299,.T.);
#14793=EDGE_CURVE('',#11891,#11893,#1300,.T.);
#14794=EDGE_CURVE('',#11894,#11895,#6161,.T.);
#14795=EDGE_CURVE('',#11894,#11892,#1301,.T.);
#14796=EDGE_CURVE('',#11893,#11895,#1302,.T.);
#14797=EDGE_CURVE('',#11896,#11897,#6162,.T.);
#14798=EDGE_CURVE('',#11896,#11894,#1303,.T.);
#14799=EDGE_CURVE('',#11895,#11897,#1304,.T.);
#14800=EDGE_CURVE('',#11898,#11899,#6163,.T.);
#14801=EDGE_CURVE('',#11898,#11896,#1305,.T.);
#14802=EDGE_CURVE('',#11897,#11899,#1306,.T.);
#14803=EDGE_CURVE('',#11900,#11901,#6164,.T.);
#14804=EDGE_CURVE('',#11900,#11898,#1307,.T.);
#14805=EDGE_CURVE('',#11899,#11901,#1308,.T.);
#14806=EDGE_CURVE('',#11902,#11903,#6165,.T.);
#14807=EDGE_CURVE('',#11902,#11900,#1309,.T.);
#14808=EDGE_CURVE('',#11901,#11903,#1310,.T.);
#14809=EDGE_CURVE('',#11904,#11905,#6166,.T.);
#14810=EDGE_CURVE('',#11904,#11902,#1311,.T.);
#14811=EDGE_CURVE('',#11903,#11905,#1312,.T.);
#14812=EDGE_CURVE('',#11906,#11907,#6167,.T.);
#14813=EDGE_CURVE('',#11906,#11904,#1313,.T.);
#14814=EDGE_CURVE('',#11905,#11907,#1314,.T.);
#14815=EDGE_CURVE('',#11908,#11909,#6168,.T.);
#14816=EDGE_CURVE('',#11908,#11906,#1315,.T.);
#14817=EDGE_CURVE('',#11907,#11909,#1316,.T.);
#14818=EDGE_CURVE('',#11910,#11911,#6169,.T.);
#14819=EDGE_CURVE('',#11910,#11908,#1317,.T.);
#14820=EDGE_CURVE('',#11909,#11911,#1318,.T.);
#14821=EDGE_CURVE('',#11912,#11913,#6170,.T.);
#14822=EDGE_CURVE('',#11912,#11910,#1319,.T.);
#14823=EDGE_CURVE('',#11911,#11913,#1320,.T.);
#14824=EDGE_CURVE('',#11914,#11915,#6171,.T.);
#14825=EDGE_CURVE('',#11914,#11912,#1321,.T.);
#14826=EDGE_CURVE('',#11913,#11915,#1322,.T.);
#14827=EDGE_CURVE('',#11916,#11917,#6172,.T.);
#14828=EDGE_CURVE('',#11916,#11914,#1323,.T.);
#14829=EDGE_CURVE('',#11915,#11917,#1324,.T.);
#14830=EDGE_CURVE('',#11918,#11919,#6173,.T.);
#14831=EDGE_CURVE('',#11918,#11916,#1325,.T.);
#14832=EDGE_CURVE('',#11917,#11919,#1326,.T.);
#14833=EDGE_CURVE('',#11920,#11921,#6174,.T.);
#14834=EDGE_CURVE('',#11920,#11918,#1327,.T.);
#14835=EDGE_CURVE('',#11919,#11921,#1328,.T.);
#14836=EDGE_CURVE('',#11922,#11923,#6175,.T.);
#14837=EDGE_CURVE('',#11922,#11920,#1329,.T.);
#14838=EDGE_CURVE('',#11921,#11923,#1330,.T.);
#14839=EDGE_CURVE('',#11924,#11925,#6176,.T.);
#14840=EDGE_CURVE('',#11924,#11926,#1331,.T.);
#14841=EDGE_CURVE('',#11925,#11926,#10841,.T.);
#14842=EDGE_CURVE('',#11927,#11928,#6177,.T.);
#14843=EDGE_CURVE('',#11927,#11924,#1332,.T.);
#14844=EDGE_CURVE('',#11929,#11925,#10842,.T.);
#14845=EDGE_CURVE('',#11928,#11929,#1333,.T.);
#14846=EDGE_CURVE('',#11930,#11931,#6178,.T.);
#14847=EDGE_CURVE('',#11930,#11927,#1334,.T.);
#14848=EDGE_CURVE('',#11931,#11928,#1335,.T.);
#14849=EDGE_CURVE('',#11932,#11933,#6179,.T.);
#14850=EDGE_CURVE('',#11932,#11930,#1336,.T.);
#14851=EDGE_CURVE('',#11933,#11931,#1337,.T.);
#14852=EDGE_CURVE('',#11934,#11935,#6180,.T.);
#14853=EDGE_CURVE('',#11934,#11932,#1338,.T.);
#14854=EDGE_CURVE('',#11935,#11933,#1339,.T.);
#14855=EDGE_CURVE('',#11936,#11937,#6181,.T.);
#14856=EDGE_CURVE('',#11936,#11934,#1340,.T.);
#14857=EDGE_CURVE('',#11937,#11935,#1341,.T.);
#14858=EDGE_CURVE('',#11938,#11939,#6182,.T.);
#14859=EDGE_CURVE('',#11938,#11936,#1342,.T.);
#14860=EDGE_CURVE('',#11939,#11937,#1343,.T.);
#14861=EDGE_CURVE('',#11940,#11941,#6183,.T.);
#14862=EDGE_CURVE('',#11940,#11938,#1344,.T.);
#14863=EDGE_CURVE('',#11941,#11939,#1345,.T.);
#14864=EDGE_CURVE('',#11942,#11943,#6184,.T.);
#14865=EDGE_CURVE('',#11942,#11940,#1346,.T.);
#14866=EDGE_CURVE('',#11943,#11941,#1347,.T.);
#14867=EDGE_CURVE('',#11944,#11945,#6185,.T.);
#14868=EDGE_CURVE('',#11944,#11942,#1348,.T.);
#14869=EDGE_CURVE('',#11945,#11943,#1349,.T.);
#14870=EDGE_CURVE('',#11946,#11947,#6186,.T.);
#14871=EDGE_CURVE('',#11946,#11944,#1350,.T.);
#14872=EDGE_CURVE('',#11947,#11945,#1351,.T.);
#14873=EDGE_CURVE('',#11948,#11949,#6187,.T.);
#14874=EDGE_CURVE('',#11948,#11946,#1352,.T.);
#14875=EDGE_CURVE('',#11949,#11947,#1353,.T.);
#14876=EDGE_CURVE('',#11950,#11951,#6188,.T.);
#14877=EDGE_CURVE('',#11950,#11948,#1354,.T.);
#14878=EDGE_CURVE('',#11951,#11949,#1355,.T.);
#14879=EDGE_CURVE('',#11952,#11953,#6189,.T.);
#14880=EDGE_CURVE('',#11952,#11950,#1356,.T.);
#14881=EDGE_CURVE('',#11953,#11951,#1357,.T.);
#14882=EDGE_CURVE('',#11954,#11955,#6190,.T.);
#14883=EDGE_CURVE('',#11954,#11952,#1358,.T.);
#14884=EDGE_CURVE('',#11955,#11953,#1359,.T.);
#14885=EDGE_CURVE('',#11956,#11957,#6191,.T.);
#14886=EDGE_CURVE('',#11956,#11954,#1360,.T.);
#14887=EDGE_CURVE('',#11957,#11955,#1361,.T.);
#14888=EDGE_CURVE('',#11958,#11959,#6192,.T.);
#14889=EDGE_CURVE('',#11958,#11956,#1362,.T.);
#14890=EDGE_CURVE('',#11959,#11957,#1363,.T.);
#14891=EDGE_CURVE('',#11960,#11961,#6193,.T.);
#14892=EDGE_CURVE('',#11960,#11958,#1364,.T.);
#14893=EDGE_CURVE('',#11961,#11959,#1365,.T.);
#14894=EDGE_CURVE('',#11962,#11963,#6194,.T.);
#14895=EDGE_CURVE('',#11962,#11960,#1366,.T.);
#14896=EDGE_CURVE('',#11963,#11961,#1367,.T.);
#14897=EDGE_CURVE('',#11926,#11964,#1368,.T.);
#14898=EDGE_CURVE('',#11965,#11964,#10843,.F.);
#14899=EDGE_CURVE('',#11966,#11965,#10844,.F.);
#14900=EDGE_CURVE('',#11966,#11929,#1369,.T.);
#14901=EDGE_CURVE('',#11923,#11966,#1370,.T.);
#14902=EDGE_CURVE('',#11967,#11887,#1371,.T.);
#14903=EDGE_CURVE('',#11967,#11963,#1372,.T.);
#14904=EDGE_CURVE('',#11887,#11968,#10845,.T.);
#14905=EDGE_CURVE('',#11968,#11886,#10846,.T.);
#14906=EDGE_CURVE('',#11886,#11969,#1373,.T.);
#14907=EDGE_CURVE('',#11969,#11967,#10847,.T.);
#14908=EDGE_CURVE('',#11969,#11962,#1374,.T.);
#14909=EDGE_CURVE('',#11964,#11922,#1375,.T.);
#14910=EDGE_CURVE('',#11970,#11971,#6195,.T.);
#14911=EDGE_CURVE('',#11971,#11970,#10848,.T.);
#14912=EDGE_CURVE('',#11971,#11972,#6196,.T.);
#14913=EDGE_CURVE('',#11972,#11971,#10849,.T.);
#14914=EDGE_CURVE('',#11972,#11973,#6197,.T.);
#14915=EDGE_CURVE('',#11973,#11972,#10850,.T.);
#14916=EDGE_CURVE('',#11973,#11974,#6198,.T.);
#14917=EDGE_CURVE('',#11974,#11973,#10851,.T.);
#14918=EDGE_CURVE('',#11974,#11975,#6199,.T.);
#14919=EDGE_CURVE('',#11975,#11974,#10852,.T.);
#14920=EDGE_CURVE('',#11975,#11970,#6200,.T.);
#14921=EDGE_CURVE('',#11970,#11975,#10853,.T.);
#14922=EDGE_CURVE('',#11976,#11977,#6201,.T.);
#14923=EDGE_CURVE('',#11978,#11977,#10854,.T.);
#14924=EDGE_CURVE('',#11972,#11978,#241,.T.);
#14925=EDGE_CURVE('',#11979,#11971,#242,.T.);
#14926=EDGE_CURVE('',#11980,#11979,#10855,.T.);
#14927=EDGE_CURVE('',#11971,#11980,#243,.T.);
#14928=EDGE_CURVE('',#11981,#11970,#244,.T.);
#14929=EDGE_CURVE('',#11982,#11981,#10856,.T.);
#14930=EDGE_CURVE('',#11970,#11982,#245,.T.);
#14931=EDGE_CURVE('',#11983,#11975,#246,.T.);
#14932=EDGE_CURVE('',#11984,#11983,#10857,.T.);
#14933=EDGE_CURVE('',#11975,#11984,#247,.T.);
#14934=EDGE_CURVE('',#11985,#11974,#248,.T.);
#14935=EDGE_CURVE('',#11986,#11985,#10858,.T.);
#14936=EDGE_CURVE('',#11974,#11986,#249,.T.);
#14937=EDGE_CURVE('',#11987,#11973,#250,.T.);
#14938=EDGE_CURVE('',#11988,#11987,#10859,.T.);
#14939=EDGE_CURVE('',#11973,#11988,#251,.T.);
#14940=EDGE_CURVE('',#11989,#11972,#252,.T.);
#14941=EDGE_CURVE('',#11977,#11989,#10860,.T.);
#14942=EDGE_CURVE('',#11990,#11973,#6202,.T.);
#14943=EDGE_CURVE('',#11991,#11990,#6203,.T.);
#14944=EDGE_CURVE('',#11991,#11972,#6204,.T.);
#14945=EDGE_CURVE('',#11972,#11992,#6205,.T.);
#14946=EDGE_CURVE('',#11992,#11989,#6206,.T.);
#14947=EDGE_CURVE('',#11993,#11974,#6207,.T.);
#14948=EDGE_CURVE('',#11990,#11993,#6208,.T.);
#14949=EDGE_CURVE('',#11986,#11994,#6209,.T.);
#14950=EDGE_CURVE('',#11974,#11994,#6210,.T.);
#14951=EDGE_CURVE('',#11973,#11995,#6211,.T.);
#14952=EDGE_CURVE('',#11995,#11987,#6212,.T.);
#14953=EDGE_CURVE('',#11996,#11991,#6213,.T.);
#14954=EDGE_CURVE('',#11996,#11971,#6214,.T.);
#14955=EDGE_CURVE('',#11971,#11997,#6215,.T.);
#14956=EDGE_CURVE('',#11997,#11979,#6216,.T.);
#14957=EDGE_CURVE('',#11998,#11975,#6217,.T.);
#14958=EDGE_CURVE('',#11993,#11998,#6218,.T.);
#14959=EDGE_CURVE('',#11984,#11999,#6219,.T.);
#14960=EDGE_CURVE('',#11975,#11999,#6220,.T.);
#14961=EDGE_CURVE('',#11994,#11985,#6221,.T.);
#14962=EDGE_CURVE('',#11988,#11995,#6222,.T.);
#14963=EDGE_CURVE('',#11999,#11983,#6223,.T.);
#14964=EDGE_CURVE('',#12000,#11981,#6224,.T.);
#14965=EDGE_CURVE('',#11982,#12000,#6225,.T.);
#14966=EDGE_CURVE('',#11980,#11997,#6226,.T.);
#14967=EDGE_CURVE('',#11978,#11992,#6227,.T.);
#14968=EDGE_CURVE('',#12001,#11970,#6228,.T.);
#14969=EDGE_CURVE('',#11998,#12001,#6229,.T.);
#14970=EDGE_CURVE('',#11970,#12000,#6230,.T.);
#14971=EDGE_CURVE('',#12001,#11996,#6231,.T.);
#14972=EDGE_CURVE('',#12002,#12002,#10861,.T.);
#14973=EDGE_CURVE('',#11968,#12002,#6232,.T.);
#14974=EDGE_CURVE('',#11964,#11966,#10862,.F.);
#14975=EDGE_CURVE('',#12003,#12003,#10863,.T.);
#14976=EDGE_CURVE('',#12003,#11965,#6233,.T.);
#14977=EDGE_CURVE('',#12004,#12005,#6234,.T.);
#14978=EDGE_CURVE('',#12005,#12005,#1376,.T.);
#14979=EDGE_CURVE('',#12004,#12004,#1377,.T.);
#14980=EDGE_CURVE('',#12006,#12006,#10864,.T.);
#14981=EDGE_CURVE('',#12006,#12007,#6235,.T.);
#14982=EDGE_CURVE('',#12007,#12007,#10865,.T.);
#14983=EDGE_CURVE('',#12008,#12008,#1378,.T.);
#14984=EDGE_CURVE('',#12009,#12009,#1379,.T.);
#14985=EDGE_CURVE('',#12005,#12010,#6236,.T.);
#14986=EDGE_CURVE('',#12010,#12010,#1380,.T.);
#14987=EDGE_CURVE('',#12011,#12012,#6237,.T.);
#14988=EDGE_CURVE('',#12013,#12012,#1381,.T.);
#14989=EDGE_CURVE('',#12013,#12014,#6238,.T.);
#14990=EDGE_CURVE('',#12011,#12014,#1382,.T.);
#14991=EDGE_CURVE('',#12008,#12010,#6239,.T.);
#14992=EDGE_CURVE('',#12015,#12015,#10866,.T.);
#14993=EDGE_CURVE('',#12015,#12016,#6240,.T.);
#14994=EDGE_CURVE('',#12016,#12016,#10867,.T.);
#14995=EDGE_CURVE('',#12017,#12018,#1383,.T.);
#14996=EDGE_CURVE('',#12019,#12017,#10868,.T.);
#14997=EDGE_CURVE('',#12020,#12019,#1384,.T.);
#14998=EDGE_CURVE('',#12021,#12020,#10869,.T.);
#14999=EDGE_CURVE('',#12021,#12016,#6241,.T.);
#15000=EDGE_CURVE('',#12018,#12021,#10870,.T.);
#15001=EDGE_CURVE('',#12022,#12022,#10871,.T.);
#15002=EDGE_CURVE('',#12014,#12017,#1385,.F.);
#15003=EDGE_CURVE('',#12018,#12011,#1386,.F.);
#15004=EDGE_CURVE('',#12012,#12020,#1387,.F.);
#15005=EDGE_CURVE('',#12019,#12013,#1388,.F.);
#15006=EDGE_CURVE('',#12023,#12024,#6242,.T.);
#15007=EDGE_CURVE('',#12024,#12025,#1389,.T.);
#15008=EDGE_CURVE('',#12025,#12024,#1390,.T.);
#15009=EDGE_CURVE('',#12023,#12026,#1391,.T.);
#15010=EDGE_CURVE('',#12026,#12027,#1392,.T.);
#15011=EDGE_CURVE('',#12027,#12023,#1393,.T.);
#15012=EDGE_CURVE('',#12028,#12028,#1394,.T.);
#15013=EDGE_CURVE('',#12028,#12025,#6243,.T.);
#15014=EDGE_CURVE('',#12029,#12029,#10872,.T.);
#15015=EDGE_CURVE('',#12029,#12030,#6244,.T.);
#15016=EDGE_CURVE('',#12030,#12030,#10873,.T.);
#15017=EDGE_CURVE('',#12009,#12028,#6245,.T.);
#15018=EDGE_CURVE('',#12030,#12031,#6246,.T.);
#15019=EDGE_CURVE('',#12031,#12031,#10874,.T.);
#15020=EDGE_CURVE('',#12032,#12032,#10875,.T.);
#15021=EDGE_CURVE('',#12007,#12032,#6247,.T.);
#15022=EDGE_CURVE('',#12022,#12006,#6248,.T.);
#15023=EDGE_CURVE('',#12033,#12034,#6249,.T.);
#15024=EDGE_CURVE('',#12034,#12035,#6250,.T.);
#15025=EDGE_CURVE('',#12035,#12036,#6251,.T.);
#15026=EDGE_CURVE('',#12036,#12037,#6252,.T.);
#15027=EDGE_CURVE('',#12037,#12038,#6253,.T.);
#15028=EDGE_CURVE('',#12038,#12033,#6254,.T.);
#15029=EDGE_CURVE('',#12038,#12039,#6255,.T.);
#15030=EDGE_CURVE('',#12040,#12039,#6256,.F.);
#15031=EDGE_CURVE('',#12040,#12041,#6257,.T.);
#15032=EDGE_CURVE('',#12041,#12033,#6258,.T.);
#15033=EDGE_CURVE('',#12042,#12037,#6259,.T.);
#15034=EDGE_CURVE('',#12042,#12039,#6260,.T.);
#15035=EDGE_CURVE('',#12036,#12043,#6261,.T.);
#15036=EDGE_CURVE('',#12043,#12044,#6262,.T.);
#15037=EDGE_CURVE('',#12044,#12042,#6263,.T.);
#15038=EDGE_CURVE('',#12045,#12046,#6264,.T.);
#15039=EDGE_CURVE('',#12046,#12047,#6265,.T.);
#15040=EDGE_CURVE('',#12047,#12048,#6266,.T.);
#15041=EDGE_CURVE('',#12048,#12049,#6267,.T.);
#15042=EDGE_CURVE('',#12049,#12050,#6268,.T.);
#15043=EDGE_CURVE('',#12050,#12045,#6269,.T.);
#15044=EDGE_CURVE('',#12050,#12051,#6270,.T.);
#15045=EDGE_CURVE('',#12052,#12051,#6271,.F.);
#15046=EDGE_CURVE('',#12052,#12053,#6272,.T.);
#15047=EDGE_CURVE('',#12053,#12045,#6273,.T.);
#15048=EDGE_CURVE('',#12054,#12049,#6274,.T.);
#15049=EDGE_CURVE('',#12054,#12051,#6275,.T.);
#15050=EDGE_CURVE('',#12048,#12055,#6276,.T.);
#15051=EDGE_CURVE('',#12055,#12056,#6277,.T.);
#15052=EDGE_CURVE('',#12056,#12054,#6278,.T.);
#15053=EDGE_CURVE('',#12057,#12058,#6279,.T.);
#15054=EDGE_CURVE('',#12058,#12059,#6280,.T.);
#15055=EDGE_CURVE('',#12059,#12060,#6281,.T.);
#15056=EDGE_CURVE('',#12060,#12061,#6282,.T.);
#15057=EDGE_CURVE('',#12061,#12062,#6283,.T.);
#15058=EDGE_CURVE('',#12062,#12057,#6284,.T.);
#15059=EDGE_CURVE('',#12063,#12061,#6285,.T.);
#15060=EDGE_CURVE('',#12063,#12064,#6286,.T.);
#15061=EDGE_CURVE('',#12062,#12064,#6287,.T.);
#15062=EDGE_CURVE('',#12060,#12065,#6288,.T.);
#15063=EDGE_CURVE('',#12065,#12066,#6289,.T.);
#15064=EDGE_CURVE('',#12066,#12063,#6290,.T.);
#15065=EDGE_CURVE('',#12059,#12067,#6291,.T.);
#15066=EDGE_CURVE('',#12068,#12067,#6292,.T.);
#15067=EDGE_CURVE('',#12069,#12068,#6293,.T.);
#15068=EDGE_CURVE('',#12069,#12065,#6294,.T.);
#15069=EDGE_CURVE('',#12070,#12071,#6295,.T.);
#15070=EDGE_CURVE('',#12071,#12072,#6296,.T.);
#15071=EDGE_CURVE('',#12072,#12073,#6297,.T.);
#15072=EDGE_CURVE('',#12073,#12074,#6298,.T.);
#15073=EDGE_CURVE('',#12074,#12075,#6299,.T.);
#15074=EDGE_CURVE('',#12075,#12070,#6300,.T.);
#15075=EDGE_CURVE('',#12075,#12076,#6301,.T.);
#15076=EDGE_CURVE('',#12077,#12076,#6302,.F.);
#15077=EDGE_CURVE('',#12077,#12078,#6303,.T.);
#15078=EDGE_CURVE('',#12078,#12070,#6304,.T.);
#15079=EDGE_CURVE('',#12079,#12074,#6305,.T.);
#15080=EDGE_CURVE('',#12079,#12076,#6306,.T.);
#15081=EDGE_CURVE('',#12073,#12080,#6307,.T.);
#15082=EDGE_CURVE('',#12080,#12081,#6308,.T.);
#15083=EDGE_CURVE('',#12081,#12079,#6309,.T.);
#15084=EDGE_CURVE('',#12082,#12083,#6310,.T.);
#15085=EDGE_CURVE('',#12083,#12084,#6311,.T.);
#15086=EDGE_CURVE('',#12084,#12085,#6312,.T.);
#15087=EDGE_CURVE('',#12085,#12086,#6313,.T.);
#15088=EDGE_CURVE('',#12086,#12087,#6314,.T.);
#15089=EDGE_CURVE('',#12087,#12082,#6315,.T.);
#15090=EDGE_CURVE('',#12088,#12083,#6316,.T.);
#15091=EDGE_CURVE('',#12089,#12088,#6317,.T.);
#15092=EDGE_CURVE('',#12084,#12089,#6318,.T.);
#15093=EDGE_CURVE('',#12090,#12082,#6319,.T.);
#15094=EDGE_CURVE('',#12090,#12091,#6320,.T.);
#15095=EDGE_CURVE('',#12092,#12091,#6321,.T.);
#15096=EDGE_CURVE('',#12088,#12092,#6322,.T.);
#15097=EDGE_CURVE('',#12087,#12093,#6323,.T.);
#15098=EDGE_CURVE('',#12093,#12094,#6324,.T.);
#15099=EDGE_CURVE('',#12094,#12090,#6325,.T.);
#15100=EDGE_CURVE('',#12095,#12096,#6326,.T.);
#15101=EDGE_CURVE('',#12096,#12097,#6327,.T.);
#15102=EDGE_CURVE('',#12097,#12098,#6328,.T.);
#15103=EDGE_CURVE('',#12098,#12099,#6329,.T.);
#15104=EDGE_CURVE('',#12099,#12100,#6330,.T.);
#15105=EDGE_CURVE('',#12100,#12095,#6331,.T.);
#15106=EDGE_CURVE('',#12098,#12101,#6332,.T.);
#15107=EDGE_CURVE('',#12101,#12102,#6333,.T.);
#15108=EDGE_CURVE('',#12103,#12102,#6334,.T.);
#15109=EDGE_CURVE('',#12103,#12099,#6335,.T.);
#15110=EDGE_CURVE('',#12097,#12104,#6336,.T.);
#15111=EDGE_CURVE('',#12105,#12104,#6337,.T.);
#15112=EDGE_CURVE('',#12106,#12105,#6338,.T.);
#15113=EDGE_CURVE('',#12106,#12101,#6339,.T.);
#15114=EDGE_CURVE('',#12107,#12096,#6340,.T.);
#15115=EDGE_CURVE('',#12104,#12107,#6341,.T.);
#15116=EDGE_CURVE('',#12107,#12108,#6342,.T.);
#15117=EDGE_CURVE('',#12108,#12109,#6343,.T.);
#15118=EDGE_CURVE('',#12109,#12110,#6344,.T.);
#15119=EDGE_CURVE('',#12110,#12105,#6345,.T.);
#15120=EDGE_CURVE('',#12110,#12111,#6346,.T.);
#15121=EDGE_CURVE('',#12111,#12112,#6347,.T.);
#15122=EDGE_CURVE('',#12112,#12106,#6348,.T.);
#15123=EDGE_CURVE('',#12113,#12114,#6349,.T.);
#15124=EDGE_CURVE('',#12114,#12115,#6350,.T.);
#15125=EDGE_CURVE('',#12115,#12116,#6351,.T.);
#15126=EDGE_CURVE('',#12116,#12117,#6352,.T.);
#15127=EDGE_CURVE('',#12117,#12118,#6353,.T.);
#15128=EDGE_CURVE('',#12118,#12113,#6354,.T.);
#15129=EDGE_CURVE('',#12119,#12117,#6355,.T.);
#15130=EDGE_CURVE('',#12120,#12119,#6356,.T.);
#15131=EDGE_CURVE('',#12118,#12120,#6357,.T.);
#15132=EDGE_CURVE('',#12116,#12121,#6358,.T.);
#15133=EDGE_CURVE('',#12121,#12122,#6359,.T.);
#15134=EDGE_CURVE('',#12119,#12122,#6360,.T.);
#15135=EDGE_CURVE('',#12053,#12121,#6361,.T.);
#15136=EDGE_CURVE('',#12115,#12046,#6362,.T.);
#15137=EDGE_CURVE('',#12123,#12124,#6363,.T.);
#15138=EDGE_CURVE('',#12124,#12125,#6364,.T.);
#15139=EDGE_CURVE('',#12125,#12126,#6365,.T.);
#15140=EDGE_CURVE('',#12126,#12127,#6366,.T.);
#15141=EDGE_CURVE('',#12127,#12128,#6367,.T.);
#15142=EDGE_CURVE('',#12128,#12123,#6368,.T.);
#15143=EDGE_CURVE('',#12129,#12124,#6369,.T.);
#15144=EDGE_CURVE('',#12130,#12129,#6370,.T.);
#15145=EDGE_CURVE('',#12125,#12130,#6371,.T.);
#15146=EDGE_CURVE('',#12131,#12123,#6372,.T.);
#15147=EDGE_CURVE('',#12131,#12132,#6373,.T.);
#15148=EDGE_CURVE('',#12133,#12132,#6374,.T.);
#15149=EDGE_CURVE('',#12129,#12133,#6375,.T.);
#15150=EDGE_CURVE('',#12128,#12134,#6376,.T.);
#15151=EDGE_CURVE('',#12134,#12135,#6377,.T.);
#15152=EDGE_CURVE('',#12135,#12131,#6378,.T.);
#15153=EDGE_CURVE('',#12136,#12137,#6379,.T.);
#15154=EDGE_CURVE('',#12137,#12138,#6380,.T.);
#15155=EDGE_CURVE('',#12138,#12139,#6381,.T.);
#15156=EDGE_CURVE('',#12139,#12140,#6382,.T.);
#15157=EDGE_CURVE('',#12140,#12141,#6383,.T.);
#15158=EDGE_CURVE('',#12141,#12136,#6384,.T.);
#15159=EDGE_CURVE('',#12139,#12142,#6385,.T.);
#15160=EDGE_CURVE('',#12142,#12143,#6386,.T.);
#15161=EDGE_CURVE('',#12144,#12143,#6387,.T.);
#15162=EDGE_CURVE('',#12144,#12140,#6388,.T.);
#15163=EDGE_CURVE('',#12138,#12145,#6389,.T.);
#15164=EDGE_CURVE('',#12146,#12145,#6390,.T.);
#15165=EDGE_CURVE('',#12147,#12146,#6391,.T.);
#15166=EDGE_CURVE('',#12147,#12142,#6392,.T.);
#15167=EDGE_CURVE('',#12148,#12137,#6393,.T.);
#15168=EDGE_CURVE('',#12145,#12148,#6394,.T.);
#15169=EDGE_CURVE('',#12148,#12149,#6395,.T.);
#15170=EDGE_CURVE('',#12149,#12150,#6396,.T.);
#15171=EDGE_CURVE('',#12150,#12151,#6397,.T.);
#15172=EDGE_CURVE('',#12151,#12146,#6398,.T.);
#15173=EDGE_CURVE('',#12151,#12152,#6399,.T.);
#15174=EDGE_CURVE('',#12152,#12153,#6400,.T.);
#15175=EDGE_CURVE('',#12153,#12147,#6401,.T.);
#15176=EDGE_CURVE('',#12154,#12155,#6402,.T.);
#15177=EDGE_CURVE('',#12155,#12156,#6403,.T.);
#15178=EDGE_CURVE('',#12156,#12157,#6404,.T.);
#15179=EDGE_CURVE('',#12157,#12158,#6405,.T.);
#15180=EDGE_CURVE('',#12158,#12159,#6406,.T.);
#15181=EDGE_CURVE('',#12159,#12154,#6407,.T.);
#15182=EDGE_CURVE('',#12160,#12158,#6408,.T.);
#15183=EDGE_CURVE('',#12161,#12160,#6409,.T.);
#15184=EDGE_CURVE('',#12159,#12161,#6410,.T.);
#15185=EDGE_CURVE('',#12157,#12162,#6411,.T.);
#15186=EDGE_CURVE('',#12162,#12163,#6412,.T.);
#15187=EDGE_CURVE('',#12160,#12163,#6413,.T.);
#15188=EDGE_CURVE('',#12041,#12162,#6414,.T.);
#15189=EDGE_CURVE('',#12156,#12034,#6415,.T.);
#15190=EDGE_CURVE('',#12164,#12165,#6416,.T.);
#15191=EDGE_CURVE('',#12165,#12166,#6417,.T.);
#15192=EDGE_CURVE('',#12166,#12167,#6418,.T.);
#15193=EDGE_CURVE('',#12167,#12168,#6419,.T.);
#15194=EDGE_CURVE('',#12168,#12169,#6420,.T.);
#15195=EDGE_CURVE('',#12169,#12164,#6421,.T.);
#15196=EDGE_CURVE('',#12167,#12170,#6422,.T.);
#15197=EDGE_CURVE('',#12170,#12171,#6423,.T.);
#15198=EDGE_CURVE('',#12172,#12171,#6424,.T.);
#15199=EDGE_CURVE('',#12172,#12168,#6425,.T.);
#15200=EDGE_CURVE('',#12166,#12173,#6426,.T.);
#15201=EDGE_CURVE('',#12174,#12173,#6427,.T.);
#15202=EDGE_CURVE('',#12175,#12174,#6428,.T.);
#15203=EDGE_CURVE('',#12175,#12170,#6429,.T.);
#15204=EDGE_CURVE('',#12176,#12165,#6430,.T.);
#15205=EDGE_CURVE('',#12173,#12176,#6431,.T.);
#15206=EDGE_CURVE('',#12176,#12177,#6432,.T.);
#15207=EDGE_CURVE('',#12177,#12178,#6433,.T.);
#15208=EDGE_CURVE('',#12178,#12179,#6434,.T.);
#15209=EDGE_CURVE('',#12179,#12174,#6435,.T.);
#15210=EDGE_CURVE('',#12179,#12180,#6436,.T.);
#15211=EDGE_CURVE('',#12180,#12181,#6437,.T.);
#15212=EDGE_CURVE('',#12181,#12175,#6438,.T.);
#15213=EDGE_CURVE('',#12182,#12183,#6439,.T.);
#15214=EDGE_CURVE('',#12183,#12184,#6440,.T.);
#15215=EDGE_CURVE('',#12184,#12185,#6441,.T.);
#15216=EDGE_CURVE('',#12185,#12186,#6442,.T.);
#15217=EDGE_CURVE('',#12186,#12187,#6443,.T.);
#15218=EDGE_CURVE('',#12187,#12182,#6444,.T.);
#15219=EDGE_CURVE('',#12188,#12186,#6445,.T.);
#15220=EDGE_CURVE('',#12189,#12188,#6446,.T.);
#15221=EDGE_CURVE('',#12187,#12189,#6447,.T.);
#15222=EDGE_CURVE('',#12185,#12190,#6448,.T.);
#15223=EDGE_CURVE('',#12190,#12191,#6449,.T.);
#15224=EDGE_CURVE('',#12188,#12191,#6450,.T.);
#15225=EDGE_CURVE('',#12184,#12192,#6451,.T.);
#15226=EDGE_CURVE('',#12193,#12192,#6452,.T.);
#15227=EDGE_CURVE('',#12194,#12193,#6453,.T.);
#15228=EDGE_CURVE('',#12194,#12190,#6454,.T.);
#15229=EDGE_CURVE('',#12192,#12195,#6455,.T.);
#15230=EDGE_CURVE('',#12195,#12196,#6456,.T.);
#15231=EDGE_CURVE('',#12196,#12197,#6457,.T.);
#15232=EDGE_CURVE('',#12197,#12198,#6458,.T.);
#15233=EDGE_CURVE('',#12198,#12193,#6459,.T.);
#15234=EDGE_CURVE('',#12199,#12197,#6460,.T.);
#15235=EDGE_CURVE('',#12199,#12200,#6461,.T.);
#15236=EDGE_CURVE('',#12198,#12200,#6462,.T.);
#15237=EDGE_CURVE('',#12196,#12201,#6463,.T.);
#15238=EDGE_CURVE('',#12201,#12202,#6464,.T.);
#15239=EDGE_CURVE('',#12202,#12199,#6465,.T.);
#15240=EDGE_CURVE('',#12203,#12182,#6466,.T.);
#15241=EDGE_CURVE('',#12203,#12201,#6467,.T.);
#15242=EDGE_CURVE('',#12195,#12183,#6468,.T.);
#15243=EDGE_CURVE('',#12204,#12205,#6469,.T.);
#15244=EDGE_CURVE('',#12205,#12206,#6470,.T.);
#15245=EDGE_CURVE('',#12206,#12207,#6471,.T.);
#15246=EDGE_CURVE('',#12207,#12208,#6472,.T.);
#15247=EDGE_CURVE('',#12208,#12209,#6473,.T.);
#15248=EDGE_CURVE('',#12209,#12204,#6474,.T.);
#15249=EDGE_CURVE('',#12207,#12210,#6475,.T.);
#15250=EDGE_CURVE('',#12210,#12211,#6476,.T.);
#15251=EDGE_CURVE('',#12212,#12211,#6477,.T.);
#15252=EDGE_CURVE('',#12212,#12208,#6478,.T.);
#15253=EDGE_CURVE('',#12206,#12213,#6479,.T.);
#15254=EDGE_CURVE('',#12214,#12213,#6480,.T.);
#15255=EDGE_CURVE('',#12215,#12214,#6481,.T.);
#15256=EDGE_CURVE('',#12215,#12210,#6482,.T.);
#15257=EDGE_CURVE('',#12216,#12205,#6483,.T.);
#15258=EDGE_CURVE('',#12213,#12216,#6484,.T.);
#15259=EDGE_CURVE('',#12216,#12217,#6485,.T.);
#15260=EDGE_CURVE('',#12217,#12218,#6486,.T.);
#15261=EDGE_CURVE('',#12218,#12219,#6487,.T.);
#15262=EDGE_CURVE('',#12219,#12214,#6488,.T.);
#15263=EDGE_CURVE('',#12219,#12220,#6489,.T.);
#15264=EDGE_CURVE('',#12220,#12221,#6490,.T.);
#15265=EDGE_CURVE('',#12221,#12215,#6491,.T.);
#15266=EDGE_CURVE('',#12222,#12223,#6492,.T.);
#15267=EDGE_CURVE('',#12223,#12224,#6493,.T.);
#15268=EDGE_CURVE('',#12224,#12225,#6494,.T.);
#15269=EDGE_CURVE('',#12225,#12226,#6495,.T.);
#15270=EDGE_CURVE('',#12226,#12227,#6496,.T.);
#15271=EDGE_CURVE('',#12227,#12222,#6497,.T.);
#15272=EDGE_CURVE('',#12225,#12228,#6498,.T.);
#15273=EDGE_CURVE('',#12228,#12229,#6499,.T.);
#15274=EDGE_CURVE('',#12230,#12229,#6500,.T.);
#15275=EDGE_CURVE('',#12230,#12226,#6501,.T.);
#15276=EDGE_CURVE('',#12224,#12231,#6502,.T.);
#15277=EDGE_CURVE('',#12232,#12231,#6503,.T.);
#15278=EDGE_CURVE('',#12233,#12232,#6504,.T.);
#15279=EDGE_CURVE('',#12233,#12228,#6505,.T.);
#15280=EDGE_CURVE('',#12234,#12223,#6506,.T.);
#15281=EDGE_CURVE('',#12231,#12234,#6507,.T.);
#15282=EDGE_CURVE('',#12234,#12235,#6508,.T.);
#15283=EDGE_CURVE('',#12235,#12236,#6509,.T.);
#15284=EDGE_CURVE('',#12236,#12237,#6510,.T.);
#15285=EDGE_CURVE('',#12237,#12232,#6511,.T.);
#15286=EDGE_CURVE('',#12237,#12238,#6512,.T.);
#15287=EDGE_CURVE('',#12238,#12239,#6513,.T.);
#15288=EDGE_CURVE('',#12239,#12233,#6514,.T.);
#15289=EDGE_CURVE('',#12240,#12241,#6515,.T.);
#15290=EDGE_CURVE('',#12241,#12242,#6516,.T.);
#15291=EDGE_CURVE('',#12242,#12243,#6517,.T.);
#15292=EDGE_CURVE('',#12243,#12244,#6518,.T.);
#15293=EDGE_CURVE('',#12244,#12245,#6519,.T.);
#15294=EDGE_CURVE('',#12245,#12240,#6520,.T.);
#15295=EDGE_CURVE('',#12245,#12246,#6521,.T.);
#15296=EDGE_CURVE('',#12247,#12246,#6522,.T.);
#15297=EDGE_CURVE('',#12247,#12248,#6523,.T.);
#15298=EDGE_CURVE('',#12248,#12240,#6524,.T.);
#15299=EDGE_CURVE('',#12249,#12244,#6525,.T.);
#15300=EDGE_CURVE('',#12246,#12249,#6526,.T.);
#15301=EDGE_CURVE('',#12243,#12250,#6527,.T.);
#15302=EDGE_CURVE('',#12250,#12251,#6528,.T.);
#15303=EDGE_CURVE('',#12249,#12251,#6529,.T.);
#15304=EDGE_CURVE('',#12252,#12253,#6530,.T.);
#15305=EDGE_CURVE('',#12253,#12254,#6531,.T.);
#15306=EDGE_CURVE('',#12254,#12255,#6532,.T.);
#15307=EDGE_CURVE('',#12255,#12256,#6533,.T.);
#15308=EDGE_CURVE('',#12256,#12257,#6534,.T.);
#15309=EDGE_CURVE('',#12257,#12252,#6535,.T.);
#15310=EDGE_CURVE('',#12255,#12258,#6536,.T.);
#15311=EDGE_CURVE('',#12258,#12259,#6537,.T.);
#15312=EDGE_CURVE('',#12260,#12259,#6538,.T.);
#15313=EDGE_CURVE('',#12260,#12256,#6539,.T.);
#15314=EDGE_CURVE('',#12254,#12261,#6540,.T.);
#15315=EDGE_CURVE('',#12262,#12261,#6541,.T.);
#15316=EDGE_CURVE('',#12263,#12262,#6542,.T.);
#15317=EDGE_CURVE('',#12263,#12258,#6543,.T.);
#15318=EDGE_CURVE('',#12264,#12253,#6544,.T.);
#15319=EDGE_CURVE('',#12261,#12264,#6545,.T.);
#15320=EDGE_CURVE('',#12264,#12265,#6546,.T.);
#15321=EDGE_CURVE('',#12265,#12266,#6547,.T.);
#15322=EDGE_CURVE('',#12266,#12267,#6548,.T.);
#15323=EDGE_CURVE('',#12267,#12262,#6549,.T.);
#15324=EDGE_CURVE('',#12267,#12268,#6550,.T.);
#15325=EDGE_CURVE('',#12268,#12269,#6551,.T.);
#15326=EDGE_CURVE('',#12269,#12263,#6552,.T.);
#15327=EDGE_CURVE('',#12270,#12271,#6553,.T.);
#15328=EDGE_CURVE('',#12271,#12272,#6554,.T.);
#15329=EDGE_CURVE('',#12272,#12273,#6555,.T.);
#15330=EDGE_CURVE('',#12273,#12274,#6556,.T.);
#15331=EDGE_CURVE('',#12274,#12275,#6557,.T.);
#15332=EDGE_CURVE('',#12275,#12270,#6558,.T.);
#15333=EDGE_CURVE('',#12273,#12276,#6559,.T.);
#15334=EDGE_CURVE('',#12276,#12277,#6560,.T.);
#15335=EDGE_CURVE('',#12278,#12277,#6561,.T.);
#15336=EDGE_CURVE('',#12278,#12274,#6562,.T.);
#15337=EDGE_CURVE('',#12272,#12279,#6563,.T.);
#15338=EDGE_CURVE('',#12280,#12279,#6564,.T.);
#15339=EDGE_CURVE('',#12281,#12280,#6565,.T.);
#15340=EDGE_CURVE('',#12281,#12276,#6566,.T.);
#15341=EDGE_CURVE('',#12282,#12271,#6567,.T.);
#15342=EDGE_CURVE('',#12279,#12282,#6568,.T.);
#15343=EDGE_CURVE('',#12282,#12283,#6569,.T.);
#15344=EDGE_CURVE('',#12283,#12284,#6570,.T.);
#15345=EDGE_CURVE('',#12284,#12285,#6571,.T.);
#15346=EDGE_CURVE('',#12285,#12280,#6572,.T.);
#15347=EDGE_CURVE('',#12285,#12286,#6573,.T.);
#15348=EDGE_CURVE('',#12286,#12287,#6574,.T.);
#15349=EDGE_CURVE('',#12287,#12281,#6575,.T.);
#15350=EDGE_CURVE('',#12067,#12288,#6576,.T.);
#15351=EDGE_CURVE('',#12288,#12289,#6577,.T.);
#15352=EDGE_CURVE('',#12289,#12290,#6578,.T.);
#15353=EDGE_CURVE('',#12290,#12291,#6579,.T.);
#15354=EDGE_CURVE('',#12291,#12068,#6580,.T.);
#15355=EDGE_CURVE('',#12291,#12292,#6581,.T.);
#15356=EDGE_CURVE('',#12293,#12292,#6582,.T.);
#15357=EDGE_CURVE('',#12293,#12069,#6583,.T.);
#15358=EDGE_CURVE('',#12294,#12290,#6584,.T.);
#15359=EDGE_CURVE('',#12292,#12294,#6585,.T.);
#15360=EDGE_CURVE('',#12289,#12295,#6586,.T.);
#15361=EDGE_CURVE('',#12295,#12296,#6587,.T.);
#15362=EDGE_CURVE('',#12294,#12296,#6588,.T.);
#15363=EDGE_CURVE('',#12297,#12298,#6589,.T.);
#15364=EDGE_CURVE('',#12298,#12299,#6590,.T.);
#15365=EDGE_CURVE('',#12299,#12300,#6591,.T.);
#15366=EDGE_CURVE('',#12300,#12297,#6592,.T.);
#15367=EDGE_CURVE('',#12301,#12300,#6593,.T.);
#15368=EDGE_CURVE('',#12302,#12301,#6594,.T.);
#15369=EDGE_CURVE('',#12297,#12302,#6595,.T.);
#15370=EDGE_CURVE('',#12303,#12303,#10876,.T.);
#15371=EDGE_CURVE('',#12299,#12304,#6596,.T.);
#15372=EDGE_CURVE('',#12305,#12304,#6597,.T.);
#15373=EDGE_CURVE('',#12306,#12305,#6598,.T.);
#15374=EDGE_CURVE('',#12301,#12306,#6599,.T.);
#15375=EDGE_CURVE('',#12307,#12308,#6600,.T.);
#15376=EDGE_CURVE('',#12308,#12305,#6601,.T.);
#15377=EDGE_CURVE('',#12305,#12309,#6602,.T.);
#15378=EDGE_CURVE('',#12309,#12310,#6603,.T.);
#15379=EDGE_CURVE('',#12310,#12311,#6604,.T.);
#15380=EDGE_CURVE('',#12311,#12307,#6605,.T.);
#15381=EDGE_CURVE('',#12308,#12312,#6606,.T.);
#15382=EDGE_CURVE('',#12306,#12312,#6607,.T.);
#15383=EDGE_CURVE('',#12307,#12313,#6608,.T.);
#15384=EDGE_CURVE('',#12313,#12314,#6609,.T.);
#15385=EDGE_CURVE('',#12314,#12315,#6610,.T.);
#15386=EDGE_CURVE('',#12315,#12316,#6611,.T.);
#15387=EDGE_CURVE('',#12316,#12308,#6612,.T.);
#15388=EDGE_CURVE('',#12311,#12317,#6613,.T.);
#15389=EDGE_CURVE('',#12318,#12317,#6614,.T.);
#15390=EDGE_CURVE('',#12319,#12318,#6615,.T.);
#15391=EDGE_CURVE('',#12319,#12313,#6616,.T.);
#15392=EDGE_CURVE('',#12312,#12302,#6617,.T.);
#15393=EDGE_CURVE('',#12320,#12321,#6618,.T.);
#15394=EDGE_CURVE('',#12321,#12322,#6619,.T.);
#15395=EDGE_CURVE('',#12322,#12323,#6620,.T.);
#15396=EDGE_CURVE('',#12323,#12324,#6621,.T.);
#15397=EDGE_CURVE('',#12324,#12325,#6622,.T.);
#15398=EDGE_CURVE('',#12325,#12320,#6623,.T.);
#15399=EDGE_CURVE('',#12320,#12326,#6624,.T.);
#15400=EDGE_CURVE('',#12326,#12319,#6625,.T.);
#15401=EDGE_CURVE('',#12327,#12318,#6626,.T.);
#15402=EDGE_CURVE('',#12327,#12321,#6627,.T.);
#15403=EDGE_CURVE('',#12325,#12328,#6628,.T.);
#15404=EDGE_CURVE('',#12329,#12328,#6629,.T.);
#15405=EDGE_CURVE('',#12330,#12329,#6630,.T.);
#15406=EDGE_CURVE('',#12330,#12326,#6631,.T.);
#15407=EDGE_CURVE('',#12331,#12324,#6632,.T.);
#15408=EDGE_CURVE('',#12328,#12331,#6633,.T.);
#15409=EDGE_CURVE('',#12332,#12333,#6634,.T.);
#15410=EDGE_CURVE('',#12333,#12334,#6635,.T.);
#15411=EDGE_CURVE('',#12334,#12335,#6636,.T.);
#15412=EDGE_CURVE('',#12335,#12336,#6637,.T.);
#15413=EDGE_CURVE('',#12336,#12337,#6638,.T.);
#15414=EDGE_CURVE('',#12337,#12332,#6639,.T.);
#15415=EDGE_CURVE('',#12335,#12338,#6640,.T.);
#15416=EDGE_CURVE('',#12338,#12339,#6641,.T.);
#15417=EDGE_CURVE('',#12340,#12339,#6642,.T.);
#15418=EDGE_CURVE('',#12340,#12336,#6643,.T.);
#15419=EDGE_CURVE('',#12334,#12341,#6644,.T.);
#15420=EDGE_CURVE('',#12342,#12341,#6645,.T.);
#15421=EDGE_CURVE('',#12343,#12342,#6646,.T.);
#15422=EDGE_CURVE('',#12343,#12338,#6647,.T.);
#15423=EDGE_CURVE('',#12344,#12333,#6648,.T.);
#15424=EDGE_CURVE('',#12341,#12344,#6649,.T.);
#15425=EDGE_CURVE('',#12344,#12345,#6650,.T.);
#15426=EDGE_CURVE('',#12345,#12346,#6651,.T.);
#15427=EDGE_CURVE('',#12346,#12347,#6652,.T.);
#15428=EDGE_CURVE('',#12347,#12342,#6653,.T.);
#15429=EDGE_CURVE('',#12347,#12348,#6654,.T.);
#15430=EDGE_CURVE('',#12348,#12349,#6655,.T.);
#15431=EDGE_CURVE('',#12349,#12343,#6656,.T.);
#15432=EDGE_CURVE('',#12350,#12351,#6657,.T.);
#15433=EDGE_CURVE('',#12351,#12352,#6658,.T.);
#15434=EDGE_CURVE('',#12352,#12353,#6659,.T.);
#15435=EDGE_CURVE('',#12353,#12354,#6660,.T.);
#15436=EDGE_CURVE('',#12354,#12355,#6661,.T.);
#15437=EDGE_CURVE('',#12355,#12350,#6662,.T.);
#15438=EDGE_CURVE('',#12353,#12356,#6663,.T.);
#15439=EDGE_CURVE('',#12356,#12357,#6664,.T.);
#15440=EDGE_CURVE('',#12358,#12357,#6665,.T.);
#15441=EDGE_CURVE('',#12358,#12354,#6666,.T.);
#15442=EDGE_CURVE('',#12352,#12359,#6667,.T.);
#15443=EDGE_CURVE('',#12360,#12359,#6668,.T.);
#15444=EDGE_CURVE('',#12361,#12360,#6669,.T.);
#15445=EDGE_CURVE('',#12361,#12356,#6670,.T.);
#15446=EDGE_CURVE('',#12362,#12351,#6671,.T.);
#15447=EDGE_CURVE('',#12359,#12362,#6672,.T.);
#15448=EDGE_CURVE('',#12362,#12363,#6673,.T.);
#15449=EDGE_CURVE('',#12363,#12364,#6674,.T.);
#15450=EDGE_CURVE('',#12364,#12365,#6675,.T.);
#15451=EDGE_CURVE('',#12365,#12360,#6676,.T.);
#15452=EDGE_CURVE('',#12365,#12366,#6677,.T.);
#15453=EDGE_CURVE('',#12366,#12367,#6678,.T.);
#15454=EDGE_CURVE('',#12367,#12361,#6679,.T.);
#15455=EDGE_CURVE('',#12368,#12369,#6680,.T.);
#15456=EDGE_CURVE('',#12369,#12370,#6681,.T.);
#15457=EDGE_CURVE('',#12370,#12371,#6682,.T.);
#15458=EDGE_CURVE('',#12371,#12372,#6683,.T.);
#15459=EDGE_CURVE('',#12372,#12373,#6684,.T.);
#15460=EDGE_CURVE('',#12373,#12368,#6685,.T.);
#15461=EDGE_CURVE('',#12371,#12374,#6686,.T.);
#15462=EDGE_CURVE('',#12374,#12375,#6687,.T.);
#15463=EDGE_CURVE('',#12376,#12375,#6688,.T.);
#15464=EDGE_CURVE('',#12376,#12372,#6689,.T.);
#15465=EDGE_CURVE('',#12370,#12377,#6690,.T.);
#15466=EDGE_CURVE('',#12378,#12377,#6691,.T.);
#15467=EDGE_CURVE('',#12379,#12378,#6692,.T.);
#15468=EDGE_CURVE('',#12379,#12374,#6693,.T.);
#15469=EDGE_CURVE('',#12380,#12369,#6694,.T.);
#15470=EDGE_CURVE('',#12377,#12380,#6695,.T.);
#15471=EDGE_CURVE('',#12380,#12381,#6696,.T.);
#15472=EDGE_CURVE('',#12381,#12382,#6697,.T.);
#15473=EDGE_CURVE('',#12382,#12383,#6698,.T.);
#15474=EDGE_CURVE('',#12383,#12378,#6699,.T.);
#15475=EDGE_CURVE('',#12383,#12384,#6700,.T.);
#15476=EDGE_CURVE('',#12384,#12385,#6701,.T.);
#15477=EDGE_CURVE('',#12385,#12379,#6702,.T.);
#15478=EDGE_CURVE('',#12386,#12387,#6703,.T.);
#15479=EDGE_CURVE('',#12387,#12388,#6704,.T.);
#15480=EDGE_CURVE('',#12388,#12389,#6705,.T.);
#15481=EDGE_CURVE('',#12389,#12390,#6706,.T.);
#15482=EDGE_CURVE('',#12390,#12391,#6707,.T.);
#15483=EDGE_CURVE('',#12391,#12386,#6708,.T.);
#15484=EDGE_CURVE('',#12389,#12392,#6709,.T.);
#15485=EDGE_CURVE('',#12392,#12393,#6710,.T.);
#15486=EDGE_CURVE('',#12394,#12393,#6711,.T.);
#15487=EDGE_CURVE('',#12394,#12390,#6712,.T.);
#15488=EDGE_CURVE('',#12388,#12395,#6713,.T.);
#15489=EDGE_CURVE('',#12396,#12395,#6714,.T.);
#15490=EDGE_CURVE('',#12397,#12396,#6715,.T.);
#15491=EDGE_CURVE('',#12397,#12392,#6716,.T.);
#15492=EDGE_CURVE('',#12398,#12387,#6717,.T.);
#15493=EDGE_CURVE('',#12395,#12398,#6718,.T.);
#15494=EDGE_CURVE('',#12398,#12399,#6719,.T.);
#15495=EDGE_CURVE('',#12399,#12400,#6720,.T.);
#15496=EDGE_CURVE('',#12400,#12401,#6721,.T.);
#15497=EDGE_CURVE('',#12401,#12396,#6722,.T.);
#15498=EDGE_CURVE('',#12401,#12402,#6723,.T.);
#15499=EDGE_CURVE('',#12402,#12403,#6724,.T.);
#15500=EDGE_CURVE('',#12403,#12397,#6725,.T.);
#15501=EDGE_CURVE('',#12404,#12405,#6726,.T.);
#15502=EDGE_CURVE('',#12405,#12406,#6727,.T.);
#15503=EDGE_CURVE('',#12406,#12407,#6728,.T.);
#15504=EDGE_CURVE('',#12407,#12408,#6729,.T.);
#15505=EDGE_CURVE('',#12408,#12409,#6730,.T.);
#15506=EDGE_CURVE('',#12409,#12404,#6731,.T.);
#15507=EDGE_CURVE('',#12410,#12408,#6732,.T.);
#15508=EDGE_CURVE('',#12411,#12410,#6733,.T.);
#15509=EDGE_CURVE('',#12409,#12411,#6734,.T.);
#15510=EDGE_CURVE('',#12407,#12412,#6735,.T.);
#15511=EDGE_CURVE('',#12412,#12413,#6736,.T.);
#15512=EDGE_CURVE('',#12410,#12413,#6737,.T.);
#15513=EDGE_CURVE('',#12078,#12412,#6738,.T.);
#15514=EDGE_CURVE('',#12406,#12071,#6739,.T.);
#15515=EDGE_CURVE('',#12296,#12287,#6740,.T.);
#15516=EDGE_CURVE('',#12286,#12294,#6741,.T.);
#15517=EDGE_CURVE('',#12414,#12286,#6742,.T.);
#15518=EDGE_CURVE('',#12292,#12414,#6743,.T.);
#15519=EDGE_CURVE('',#12414,#12284,#6744,.T.);
#15520=EDGE_CURVE('',#12277,#12269,#6745,.T.);
#15521=EDGE_CURVE('',#12268,#12278,#6746,.T.);
#15522=EDGE_CURVE('',#12415,#12278,#6747,.T.);
#15523=EDGE_CURVE('',#12275,#12415,#6748,.T.);
#15524=EDGE_CURVE('',#12416,#12268,#6749,.T.);
#15525=EDGE_CURVE('',#12415,#12416,#6750,.T.);
#15526=EDGE_CURVE('',#12416,#12266,#6751,.T.);
#15527=EDGE_CURVE('',#12259,#12077,#6752,.T.);
#15528=EDGE_CURVE('',#12076,#12260,#6753,.T.);
#15529=EDGE_CURVE('',#12417,#12260,#6754,.T.);
#15530=EDGE_CURVE('',#12257,#12417,#6755,.T.);
#15531=EDGE_CURVE('',#12417,#12079,#6756,.T.);
#15532=EDGE_CURVE('',#12418,#12295,#6757,.T.);
#15533=EDGE_CURVE('',#12419,#12418,#6758,.T.);
#15534=EDGE_CURVE('',#12420,#12419,#6759,.T.);
#15535=EDGE_CURVE('',#12421,#12420,#6760,.T.);
#15536=EDGE_CURVE('',#12422,#12421,#6761,.T.);
#15537=EDGE_CURVE('',#12423,#12422,#6762,.T.);
#15538=EDGE_CURVE('',#12424,#12423,#6763,.T.);
#15539=EDGE_CURVE('',#12425,#12424,#6764,.T.);
#15540=EDGE_CURVE('',#12426,#12425,#6765,.T.);
#15541=EDGE_CURVE('',#12427,#12426,#6766,.T.);
#15542=EDGE_CURVE('',#12428,#12427,#6767,.T.);
#15543=EDGE_CURVE('',#12429,#12428,#6768,.T.);
#15544=EDGE_CURVE('',#12430,#12429,#6769,.T.);
#15545=EDGE_CURVE('',#12431,#12430,#6770,.T.);
#15546=EDGE_CURVE('',#12432,#12431,#6771,.T.);
#15547=EDGE_CURVE('',#12433,#12432,#6772,.T.);
#15548=EDGE_CURVE('',#12434,#12433,#6773,.T.);
#15549=EDGE_CURVE('',#12435,#12434,#6774,.T.);
#15550=EDGE_CURVE('',#12436,#12435,#6775,.T.);
#15551=EDGE_CURVE('',#12437,#12436,#6776,.T.);
#15552=EDGE_CURVE('',#12438,#12437,#6777,.T.);
#15553=EDGE_CURVE('',#12439,#12438,#6778,.T.);
#15554=EDGE_CURVE('',#12440,#12439,#6779,.T.);
#15555=EDGE_CURVE('',#12441,#12440,#6780,.T.);
#15556=EDGE_CURVE('',#12442,#12441,#6781,.T.);
#15557=EDGE_CURVE('',#12443,#12442,#6782,.T.);
#15558=EDGE_CURVE('',#12444,#12443,#6783,.T.);
#15559=EDGE_CURVE('',#12091,#12444,#6784,.T.);
#15560=EDGE_CURVE('',#12102,#12094,#6785,.T.);
#15561=EDGE_CURVE('',#12122,#12112,#6786,.T.);
#15562=EDGE_CURVE('',#12445,#12052,#6787,.T.);
#15563=EDGE_CURVE('',#12446,#12445,#6788,.T.);
#15564=EDGE_CURVE('',#12447,#12446,#6789,.T.);
#15565=EDGE_CURVE('',#12448,#12447,#6790,.T.);
#15566=EDGE_CURVE('',#12449,#12448,#6791,.T.);
#15567=EDGE_CURVE('',#12450,#12449,#6792,.T.);
#15568=EDGE_CURVE('',#12451,#12450,#6793,.T.);
#15569=EDGE_CURVE('',#12452,#12451,#6794,.T.);
#15570=EDGE_CURVE('',#12453,#12452,#6795,.T.);
#15571=EDGE_CURVE('',#12454,#12453,#6796,.T.);
#15572=EDGE_CURVE('',#12455,#12454,#6797,.T.);
#15573=EDGE_CURVE('',#12456,#12455,#6798,.T.);
#15574=EDGE_CURVE('',#12457,#12456,#6799,.T.);
#15575=EDGE_CURVE('',#12458,#12457,#6800,.T.);
#15576=EDGE_CURVE('',#12459,#12458,#6801,.T.);
#15577=EDGE_CURVE('',#12460,#12459,#6802,.T.);
#15578=EDGE_CURVE('',#12461,#12460,#6803,.T.);
#15579=EDGE_CURVE('',#12462,#12461,#6804,.T.);
#15580=EDGE_CURVE('',#12463,#12462,#6805,.T.);
#15581=EDGE_CURVE('',#12464,#12463,#6806,.T.);
#15582=EDGE_CURVE('',#12465,#12464,#6807,.T.);
#15583=EDGE_CURVE('',#12466,#12465,#6808,.T.);
#15584=EDGE_CURVE('',#12467,#12466,#6809,.T.);
#15585=EDGE_CURVE('',#12468,#12467,#6810,.T.);
#15586=EDGE_CURVE('',#12469,#12468,#6811,.T.);
#15587=EDGE_CURVE('',#12132,#12469,#6812,.T.);
#15588=EDGE_CURVE('',#12143,#12135,#6813,.T.);
#15589=EDGE_CURVE('',#12163,#12153,#6814,.T.);
#15590=EDGE_CURVE('',#12171,#12040,#6815,.T.);
#15591=EDGE_CURVE('',#12191,#12181,#6816,.T.);
#15592=EDGE_CURVE('',#12470,#12194,#6817,.T.);
#15593=EDGE_CURVE('',#12211,#12470,#6818,.T.);
#15594=EDGE_CURVE('',#12229,#12221,#6819,.T.);
#15595=EDGE_CURVE('',#12251,#12239,#6820,.T.);
#15596=EDGE_CURVE('',#12314,#12250,#6821,.T.);
#15597=EDGE_CURVE('',#12471,#12330,#6822,.T.);
#15598=EDGE_CURVE('',#12472,#12471,#6823,.T.);
#15599=EDGE_CURVE('',#12473,#12472,#6824,.T.);
#15600=EDGE_CURVE('',#12474,#12473,#6825,.T.);
#15601=EDGE_CURVE('',#12475,#12474,#6826,.T.);
#15602=EDGE_CURVE('',#12339,#12475,#6827,.T.);
#15603=EDGE_CURVE('',#12357,#12349,#6828,.T.);
#15604=EDGE_CURVE('',#12375,#12367,#6829,.T.);
#15605=EDGE_CURVE('',#12393,#12385,#6830,.T.);
#15606=EDGE_CURVE('',#12413,#12403,#6831,.T.);
#15607=EDGE_CURVE('',#12402,#12410,#6832,.T.);
#15608=EDGE_CURVE('',#12476,#12402,#6833,.T.);
#15609=EDGE_CURVE('',#12411,#12476,#6834,.T.);
#15610=EDGE_CURVE('',#12476,#12400,#6835,.T.);
#15611=EDGE_CURVE('',#12384,#12394,#6836,.T.);
#15612=EDGE_CURVE('',#12477,#12394,#6837,.T.);
#15613=EDGE_CURVE('',#12391,#12477,#6838,.T.);
#15614=EDGE_CURVE('',#12478,#12384,#6839,.T.);
#15615=EDGE_CURVE('',#12477,#12478,#6840,.T.);
#15616=EDGE_CURVE('',#12478,#12382,#6841,.T.);
#15617=EDGE_CURVE('',#12366,#12376,#6842,.T.);
#15618=EDGE_CURVE('',#12479,#12376,#6843,.T.);
#15619=EDGE_CURVE('',#12373,#12479,#6844,.T.);
#15620=EDGE_CURVE('',#12480,#12366,#6845,.T.);
#15621=EDGE_CURVE('',#12479,#12480,#6846,.T.);
#15622=EDGE_CURVE('',#12480,#12364,#6847,.T.);
#15623=EDGE_CURVE('',#12348,#12358,#6848,.T.);
#15624=EDGE_CURVE('',#12481,#12358,#6849,.T.);
#15625=EDGE_CURVE('',#12355,#12481,#6850,.T.);
#15626=EDGE_CURVE('',#12482,#12348,#6851,.T.);
#15627=EDGE_CURVE('',#12481,#12482,#6852,.T.);
#15628=EDGE_CURVE('',#12482,#12346,#6853,.T.);
#15629=EDGE_CURVE('',#12475,#12483,#6854,.F.);
#15630=EDGE_CURVE('',#12483,#12340,#6855,.T.);
#15631=EDGE_CURVE('',#12484,#12340,#6856,.T.);
#15632=EDGE_CURVE('',#12337,#12484,#6857,.T.);
#15633=EDGE_CURVE('',#12485,#12483,#6858,.T.);
#15634=EDGE_CURVE('',#12484,#12485,#6859,.T.);
#15635=EDGE_CURVE('',#12486,#12487,#6860,.T.);
#15636=EDGE_CURVE('',#12487,#12488,#6861,.T.);
#15637=EDGE_CURVE('',#12488,#12489,#6862,.T.);
#15638=EDGE_CURVE('',#12489,#12486,#6863,.T.);
#15639=EDGE_CURVE('',#12488,#12490,#6864,.T.);
#15640=EDGE_CURVE('',#12322,#12490,#6865,.T.);
#15641=EDGE_CURVE('',#12491,#12322,#6866,.T.);
#15642=EDGE_CURVE('',#12491,#12489,#6867,.T.);
#15643=EDGE_CURVE('',#12487,#12327,#6868,.T.);
#15644=EDGE_CURVE('',#12490,#12327,#6869,.T.);
#15645=EDGE_CURVE('',#12492,#12490,#6870,.T.);
#15646=EDGE_CURVE('',#12317,#12493,#6871,.T.);
#15647=EDGE_CURVE('',#12493,#12492,#6872,.T.);
#15648=EDGE_CURVE('',#12492,#12494,#6873,.T.);
#15649=EDGE_CURVE('',#12494,#12495,#6874,.T.);
#15650=EDGE_CURVE('',#12495,#12323,#6875,.T.);
#15651=EDGE_CURVE('',#12496,#12309,#6876,.T.);
#15652=EDGE_CURVE('',#12496,#12494,#6877,.T.);
#15653=EDGE_CURVE('',#12493,#12310,#6878,.T.);
#15654=EDGE_CURVE('',#12331,#12497,#6879,.T.);
#15655=EDGE_CURVE('',#12497,#12498,#6880,.T.);
#15656=EDGE_CURVE('',#12498,#12499,#6881,.T.);
#15657=EDGE_CURVE('',#12499,#12329,#6882,.T.);
#15658=EDGE_CURVE('',#12499,#12500,#6883,.T.);
#15659=EDGE_CURVE('',#12500,#12471,#6884,.T.);
#15660=EDGE_CURVE('',#12501,#12502,#6885,.T.);
#15661=EDGE_CURVE('',#12502,#12503,#6886,.T.);
#15662=EDGE_CURVE('',#12503,#12504,#6887,.T.);
#15663=EDGE_CURVE('',#12504,#12505,#6888,.T.);
#15664=EDGE_CURVE('',#12505,#12506,#6889,.T.);
#15665=EDGE_CURVE('',#12506,#12501,#6890,.T.);
#15666=EDGE_CURVE('',#12504,#12473,#6891,.T.);
#15667=EDGE_CURVE('',#12507,#12472,#6892,.T.);
#15668=EDGE_CURVE('',#12507,#12505,#6893,.T.);
#15669=EDGE_CURVE('',#12503,#12508,#6894,.T.);
#15670=EDGE_CURVE('',#12509,#12508,#6895,.T.);
#15671=EDGE_CURVE('',#12474,#12509,#6896,.T.);
#15672=EDGE_CURVE('',#12510,#12502,#6897,.T.);
#15673=EDGE_CURVE('',#12508,#12510,#6898,.T.);
#15674=EDGE_CURVE('',#12510,#12511,#6899,.T.);
#15675=EDGE_CURVE('',#12511,#12512,#6900,.T.);
#15676=EDGE_CURVE('',#12512,#12513,#6901,.T.);
#15677=EDGE_CURVE('',#12513,#12509,#6902,.T.);
#15678=EDGE_CURVE('',#12513,#12483,#6903,.T.);
#15679=EDGE_CURVE('',#12485,#12512,#6904,.T.);
#15680=EDGE_CURVE('',#12500,#12507,#6905,.T.);
#15681=EDGE_CURVE('',#12514,#12507,#6906,.T.);
#15682=EDGE_CURVE('',#12506,#12514,#6907,.T.);
#15683=EDGE_CURVE('',#12515,#12500,#6908,.T.);
#15684=EDGE_CURVE('',#12514,#12515,#6909,.T.);
#15685=EDGE_CURVE('',#12515,#12498,#6910,.T.);
#15686=EDGE_CURVE('',#12238,#12249,#6911,.T.);
#15687=EDGE_CURVE('',#12516,#12238,#6912,.T.);
#15688=EDGE_CURVE('',#12246,#12516,#6913,.T.);
#15689=EDGE_CURVE('',#12516,#12236,#6914,.T.);
#15690=EDGE_CURVE('',#12220,#12230,#6915,.T.);
#15691=EDGE_CURVE('',#12517,#12230,#6916,.T.);
#15692=EDGE_CURVE('',#12227,#12517,#6917,.T.);
#15693=EDGE_CURVE('',#12518,#12220,#6918,.T.);
#15694=EDGE_CURVE('',#12517,#12518,#6919,.T.);
#15695=EDGE_CURVE('',#12518,#12218,#6920,.T.);
#15696=EDGE_CURVE('',#12200,#12470,#6921,.T.);
#15697=EDGE_CURVE('',#12200,#12212,#6922,.T.);
#15698=EDGE_CURVE('',#12519,#12212,#6923,.T.);
#15699=EDGE_CURVE('',#12209,#12519,#6924,.T.);
#15700=EDGE_CURVE('',#12519,#12199,#6925,.T.);
#15701=EDGE_CURVE('',#12180,#12188,#6926,.T.);
#15702=EDGE_CURVE('',#12520,#12180,#6927,.T.);
#15703=EDGE_CURVE('',#12189,#12520,#6928,.T.);
#15704=EDGE_CURVE('',#12520,#12178,#6929,.T.);
#15705=EDGE_CURVE('',#12039,#12172,#6930,.T.);
#15706=EDGE_CURVE('',#12521,#12172,#6931,.T.);
#15707=EDGE_CURVE('',#12169,#12521,#6932,.T.);
#15708=EDGE_CURVE('',#12521,#12042,#6933,.T.);
#15709=EDGE_CURVE('',#12152,#12160,#6934,.T.);
#15710=EDGE_CURVE('',#12522,#12152,#6935,.T.);
#15711=EDGE_CURVE('',#12161,#12522,#6936,.T.);
#15712=EDGE_CURVE('',#12522,#12150,#6937,.T.);
#15713=EDGE_CURVE('',#12134,#12144,#6938,.T.);
#15714=EDGE_CURVE('',#12523,#12144,#6939,.T.);
#15715=EDGE_CURVE('',#12141,#12523,#6940,.T.);
#15716=EDGE_CURVE('',#12524,#12134,#6941,.T.);
#15717=EDGE_CURVE('',#12523,#12524,#6942,.T.);
#15718=EDGE_CURVE('',#12524,#12127,#6943,.T.);
#15719=EDGE_CURVE('',#12525,#12526,#6944,.T.);
#15720=EDGE_CURVE('',#12526,#12527,#6945,.T.);
#15721=EDGE_CURVE('',#12527,#12528,#6946,.T.);
#15722=EDGE_CURVE('',#12528,#12529,#6947,.T.);
#15723=EDGE_CURVE('',#12529,#12530,#6948,.T.);
#15724=EDGE_CURVE('',#12530,#12525,#6949,.T.);
#15725=EDGE_CURVE('',#12528,#12446,#6950,.T.);
#15726=EDGE_CURVE('',#12531,#12445,#6951,.T.);
#15727=EDGE_CURVE('',#12531,#12529,#6952,.T.);
#15728=EDGE_CURVE('',#12527,#12532,#6953,.T.);
#15729=EDGE_CURVE('',#12533,#12532,#6954,.T.);
#15730=EDGE_CURVE('',#12447,#12533,#6955,.T.);
#15731=EDGE_CURVE('',#12534,#12526,#6956,.T.);
#15732=EDGE_CURVE('',#12532,#12534,#6957,.T.);
#15733=EDGE_CURVE('',#12534,#12535,#6958,.T.);
#15734=EDGE_CURVE('',#12535,#12536,#6959,.T.);
#15735=EDGE_CURVE('',#12536,#12537,#6960,.T.);
#15736=EDGE_CURVE('',#12537,#12533,#6961,.T.);
#15737=EDGE_CURVE('',#12537,#12538,#6962,.T.);
#15738=EDGE_CURVE('',#12538,#12448,#6963,.T.);
#15739=EDGE_CURVE('',#12539,#12540,#6964,.T.);
#15740=EDGE_CURVE('',#12540,#12541,#6965,.T.);
#15741=EDGE_CURVE('',#12541,#12542,#6966,.T.);
#15742=EDGE_CURVE('',#12542,#12543,#6967,.T.);
#15743=EDGE_CURVE('',#12543,#12544,#6968,.T.);
#15744=EDGE_CURVE('',#12544,#12539,#6969,.T.);
#15745=EDGE_CURVE('',#12542,#12450,#6970,.T.);
#15746=EDGE_CURVE('',#12545,#12449,#6971,.T.);
#15747=EDGE_CURVE('',#12545,#12543,#6972,.T.);
#15748=EDGE_CURVE('',#12541,#12546,#6973,.T.);
#15749=EDGE_CURVE('',#12547,#12546,#6974,.T.);
#15750=EDGE_CURVE('',#12451,#12547,#6975,.T.);
#15751=EDGE_CURVE('',#12548,#12540,#6976,.T.);
#15752=EDGE_CURVE('',#12546,#12548,#6977,.T.);
#15753=EDGE_CURVE('',#12548,#12549,#6978,.T.);
#15754=EDGE_CURVE('',#12549,#12550,#6979,.T.);
#15755=EDGE_CURVE('',#12550,#12551,#6980,.T.);
#15756=EDGE_CURVE('',#12551,#12547,#6981,.T.);
#15757=EDGE_CURVE('',#12551,#12552,#6982,.T.);
#15758=EDGE_CURVE('',#12552,#12452,#6983,.T.);
#15759=EDGE_CURVE('',#12553,#12554,#6984,.T.);
#15760=EDGE_CURVE('',#12554,#12555,#6985,.T.);
#15761=EDGE_CURVE('',#12555,#12556,#6986,.T.);
#15762=EDGE_CURVE('',#12556,#12557,#6987,.T.);
#15763=EDGE_CURVE('',#12557,#12558,#6988,.T.);
#15764=EDGE_CURVE('',#12558,#12553,#6989,.T.);
#15765=EDGE_CURVE('',#12556,#12454,#6990,.T.);
#15766=EDGE_CURVE('',#12559,#12453,#6991,.T.);
#15767=EDGE_CURVE('',#12559,#12557,#6992,.T.);
#15768=EDGE_CURVE('',#12555,#12560,#6993,.T.);
#15769=EDGE_CURVE('',#12561,#12560,#6994,.T.);
#15770=EDGE_CURVE('',#12455,#12561,#6995,.T.);
#15771=EDGE_CURVE('',#12562,#12554,#6996,.T.);
#15772=EDGE_CURVE('',#12560,#12562,#6997,.T.);
#15773=EDGE_CURVE('',#12562,#12563,#6998,.T.);
#15774=EDGE_CURVE('',#12563,#12564,#6999,.T.);
#15775=EDGE_CURVE('',#12564,#12565,#7000,.T.);
#15776=EDGE_CURVE('',#12565,#12561,#7001,.T.);
#15777=EDGE_CURVE('',#12565,#12566,#7002,.T.);
#15778=EDGE_CURVE('',#12566,#12456,#7003,.T.);
#15779=EDGE_CURVE('',#12567,#12568,#7004,.T.);
#15780=EDGE_CURVE('',#12568,#12569,#7005,.T.);
#15781=EDGE_CURVE('',#12569,#12570,#7006,.T.);
#15782=EDGE_CURVE('',#12570,#12571,#7007,.T.);
#15783=EDGE_CURVE('',#12571,#12572,#7008,.T.);
#15784=EDGE_CURVE('',#12572,#12567,#7009,.T.);
#15785=EDGE_CURVE('',#12573,#12571,#7010,.T.);
#15786=EDGE_CURVE('',#12574,#12573,#7011,.T.);
#15787=EDGE_CURVE('',#12572,#12574,#7012,.T.);
#15788=EDGE_CURVE('',#12570,#12458,#7013,.T.);
#15789=EDGE_CURVE('',#12573,#12457,#7014,.T.);
#15790=EDGE_CURVE('',#12569,#12575,#7015,.T.);
#15791=EDGE_CURVE('',#12576,#12575,#7016,.T.);
#15792=EDGE_CURVE('',#12459,#12576,#7017,.T.);
#15793=EDGE_CURVE('',#12575,#12577,#7018,.T.);
#15794=EDGE_CURVE('',#12577,#12578,#7019,.T.);
#15795=EDGE_CURVE('',#12578,#12579,#7020,.T.);
#15796=EDGE_CURVE('',#12579,#12580,#7021,.T.);
#15797=EDGE_CURVE('',#12580,#12576,#7022,.T.);
#15798=EDGE_CURVE('',#12581,#12579,#7023,.T.);
#15799=EDGE_CURVE('',#12581,#12582,#7024,.T.);
#15800=EDGE_CURVE('',#12580,#12582,#7025,.T.);
#15801=EDGE_CURVE('',#12578,#12583,#7026,.T.);
#15802=EDGE_CURVE('',#12583,#12584,#7027,.T.);
#15803=EDGE_CURVE('',#12584,#12581,#7028,.T.);
#15804=EDGE_CURVE('',#12585,#12567,#7029,.T.);
#15805=EDGE_CURVE('',#12585,#12583,#7030,.T.);
#15806=EDGE_CURVE('',#12577,#12568,#7031,.T.);
#15807=EDGE_CURVE('',#12586,#12587,#7032,.T.);
#15808=EDGE_CURVE('',#12587,#12588,#7033,.T.);
#15809=EDGE_CURVE('',#12588,#12589,#7034,.T.);
#15810=EDGE_CURVE('',#12589,#12590,#7035,.T.);
#15811=EDGE_CURVE('',#12590,#12591,#7036,.T.);
#15812=EDGE_CURVE('',#12591,#12586,#7037,.T.);
#15813=EDGE_CURVE('',#12589,#12462,#7038,.T.);
#15814=EDGE_CURVE('',#12592,#12461,#7039,.T.);
#15815=EDGE_CURVE('',#12592,#12590,#7040,.T.);
#15816=EDGE_CURVE('',#12588,#12593,#7041,.T.);
#15817=EDGE_CURVE('',#12594,#12593,#7042,.T.);
#15818=EDGE_CURVE('',#12463,#12594,#7043,.T.);
#15819=EDGE_CURVE('',#12595,#12587,#7044,.T.);
#15820=EDGE_CURVE('',#12593,#12595,#7045,.T.);
#15821=EDGE_CURVE('',#12595,#12596,#7046,.T.);
#15822=EDGE_CURVE('',#12596,#12597,#7047,.T.);
#15823=EDGE_CURVE('',#12597,#12598,#7048,.T.);
#15824=EDGE_CURVE('',#12598,#12594,#7049,.T.);
#15825=EDGE_CURVE('',#12598,#12599,#7050,.T.);
#15826=EDGE_CURVE('',#12599,#12464,#7051,.T.);
#15827=EDGE_CURVE('',#12600,#12601,#7052,.T.);
#15828=EDGE_CURVE('',#12601,#12602,#7053,.T.);
#15829=EDGE_CURVE('',#12602,#12603,#7054,.T.);
#15830=EDGE_CURVE('',#12603,#12604,#7055,.T.);
#15831=EDGE_CURVE('',#12604,#12605,#7056,.T.);
#15832=EDGE_CURVE('',#12605,#12600,#7057,.T.);
#15833=EDGE_CURVE('',#12603,#12466,#7058,.T.);
#15834=EDGE_CURVE('',#12606,#12465,#7059,.T.);
#15835=EDGE_CURVE('',#12606,#12604,#7060,.T.);
#15836=EDGE_CURVE('',#12602,#12607,#7061,.T.);
#15837=EDGE_CURVE('',#12608,#12607,#7062,.T.);
#15838=EDGE_CURVE('',#12467,#12608,#7063,.T.);
#15839=EDGE_CURVE('',#12609,#12601,#7064,.T.);
#15840=EDGE_CURVE('',#12607,#12609,#7065,.T.);
#15841=EDGE_CURVE('',#12609,#12610,#7066,.T.);
#15842=EDGE_CURVE('',#12610,#12611,#7067,.T.);
#15843=EDGE_CURVE('',#12611,#12612,#7068,.T.);
#15844=EDGE_CURVE('',#12612,#12608,#7069,.T.);
#15845=EDGE_CURVE('',#12612,#12613,#7070,.T.);
#15846=EDGE_CURVE('',#12613,#12468,#7071,.T.);
#15847=EDGE_CURVE('',#12614,#12130,#7072,.T.);
#15848=EDGE_CURVE('',#12133,#12615,#7073,.T.);
#15849=EDGE_CURVE('',#12615,#12616,#7074,.T.);
#15850=EDGE_CURVE('',#12616,#12614,#7075,.T.);
#15851=EDGE_CURVE('',#12616,#12617,#7076,.T.);
#15852=EDGE_CURVE('',#12618,#12617,#7077,.T.);
#15853=EDGE_CURVE('',#12618,#12619,#7078,.T.);
#15854=EDGE_CURVE('',#12619,#12614,#7079,.T.);
#15855=EDGE_CURVE('',#12620,#12615,#7080,.T.);
#15856=EDGE_CURVE('',#12617,#12620,#7081,.T.);
#15857=EDGE_CURVE('',#12620,#12469,#7082,.T.);
#15858=EDGE_CURVE('',#12613,#12620,#7083,.T.);
#15859=EDGE_CURVE('',#12621,#12613,#7084,.T.);
#15860=EDGE_CURVE('',#12617,#12621,#7085,.T.);
#15861=EDGE_CURVE('',#12621,#12611,#7086,.T.);
#15862=EDGE_CURVE('',#12599,#12606,#7087,.T.);
#15863=EDGE_CURVE('',#12622,#12606,#7088,.T.);
#15864=EDGE_CURVE('',#12605,#12622,#7089,.T.);
#15865=EDGE_CURVE('',#12623,#12599,#7090,.T.);
#15866=EDGE_CURVE('',#12622,#12623,#7091,.T.);
#15867=EDGE_CURVE('',#12623,#12597,#7092,.T.);
#15868=EDGE_CURVE('',#12582,#12460,#7093,.T.);
#15869=EDGE_CURVE('',#12582,#12592,#7094,.T.);
#15870=EDGE_CURVE('',#12624,#12592,#7095,.T.);
#15871=EDGE_CURVE('',#12591,#12624,#7096,.T.);
#15872=EDGE_CURVE('',#12624,#12581,#7097,.T.);
#15873=EDGE_CURVE('',#12566,#12573,#7098,.T.);
#15874=EDGE_CURVE('',#12625,#12566,#7099,.T.);
#15875=EDGE_CURVE('',#12574,#12625,#7100,.T.);
#15876=EDGE_CURVE('',#12625,#12564,#7101,.T.);
#15877=EDGE_CURVE('',#12552,#12559,#7102,.T.);
#15878=EDGE_CURVE('',#12626,#12559,#7103,.T.);
#15879=EDGE_CURVE('',#12558,#12626,#7104,.T.);
#15880=EDGE_CURVE('',#12627,#12552,#7105,.T.);
#15881=EDGE_CURVE('',#12626,#12627,#7106,.T.);
#15882=EDGE_CURVE('',#12627,#12550,#7107,.T.);
#15883=EDGE_CURVE('',#12538,#12545,#7108,.T.);
#15884=EDGE_CURVE('',#12628,#12545,#7109,.T.);
#15885=EDGE_CURVE('',#12544,#12628,#7110,.T.);
#15886=EDGE_CURVE('',#12629,#12538,#7111,.T.);
#15887=EDGE_CURVE('',#12628,#12629,#7112,.T.);
#15888=EDGE_CURVE('',#12629,#12536,#7113,.T.);
#15889=EDGE_CURVE('',#12051,#12531,#7114,.T.);
#15890=EDGE_CURVE('',#12630,#12531,#7115,.T.);
#15891=EDGE_CURVE('',#12530,#12630,#7116,.T.);
#15892=EDGE_CURVE('',#12630,#12054,#7117,.T.);
#15893=EDGE_CURVE('',#12111,#12119,#7118,.T.);
#15894=EDGE_CURVE('',#12631,#12111,#7119,.T.);
#15895=EDGE_CURVE('',#12120,#12631,#7120,.T.);
#15896=EDGE_CURVE('',#12631,#12109,#7121,.T.);
#15897=EDGE_CURVE('',#12093,#12103,#7122,.T.);
#15898=EDGE_CURVE('',#12632,#12103,#7123,.T.);
#15899=EDGE_CURVE('',#12100,#12632,#7124,.T.);
#15900=EDGE_CURVE('',#12633,#12093,#7125,.T.);
#15901=EDGE_CURVE('',#12632,#12633,#7126,.T.);
#15902=EDGE_CURVE('',#12633,#12086,#7127,.T.);
#15903=EDGE_CURVE('',#12634,#12635,#7128,.T.);
#15904=EDGE_CURVE('',#12635,#12636,#7129,.T.);
#15905=EDGE_CURVE('',#12636,#12637,#7130,.T.);
#15906=EDGE_CURVE('',#12637,#12638,#7131,.T.);
#15907=EDGE_CURVE('',#12638,#12639,#7132,.T.);
#15908=EDGE_CURVE('',#12639,#12634,#7133,.T.);
#15909=EDGE_CURVE('',#12637,#12421,#7134,.T.);
#15910=EDGE_CURVE('',#12640,#12420,#7135,.T.);
#15911=EDGE_CURVE('',#12640,#12638,#7136,.T.);
#15912=EDGE_CURVE('',#12636,#12641,#7137,.T.);
#15913=EDGE_CURVE('',#12642,#12641,#7138,.T.);
#15914=EDGE_CURVE('',#12422,#12642,#7139,.T.);
#15915=EDGE_CURVE('',#12643,#12635,#7140,.T.);
#15916=EDGE_CURVE('',#12641,#12643,#7141,.T.);
#15917=EDGE_CURVE('',#12643,#12644,#7142,.T.);
#15918=EDGE_CURVE('',#12644,#12645,#7143,.T.);
#15919=EDGE_CURVE('',#12645,#12646,#7144,.T.);
#15920=EDGE_CURVE('',#12646,#12642,#7145,.T.);
#15921=EDGE_CURVE('',#12646,#12647,#7146,.T.);
#15922=EDGE_CURVE('',#12647,#12423,#7147,.T.);
#15923=EDGE_CURVE('',#12648,#12649,#7148,.T.);
#15924=EDGE_CURVE('',#12649,#12650,#7149,.T.);
#15925=EDGE_CURVE('',#12650,#12651,#7150,.T.);
#15926=EDGE_CURVE('',#12651,#12652,#7151,.T.);
#15927=EDGE_CURVE('',#12652,#12653,#7152,.T.);
#15928=EDGE_CURVE('',#12653,#12648,#7153,.T.);
#15929=EDGE_CURVE('',#12651,#12425,#7154,.T.);
#15930=EDGE_CURVE('',#12654,#12424,#7155,.T.);
#15931=EDGE_CURVE('',#12654,#12652,#7156,.T.);
#15932=EDGE_CURVE('',#12650,#12655,#7157,.T.);
#15933=EDGE_CURVE('',#12656,#12655,#7158,.T.);
#15934=EDGE_CURVE('',#12426,#12656,#7159,.T.);
#15935=EDGE_CURVE('',#12657,#12649,#7160,.T.);
#15936=EDGE_CURVE('',#12655,#12657,#7161,.T.);
#15937=EDGE_CURVE('',#12657,#12658,#7162,.T.);
#15938=EDGE_CURVE('',#12658,#12659,#7163,.T.);
#15939=EDGE_CURVE('',#12659,#12660,#7164,.T.);
#15940=EDGE_CURVE('',#12660,#12656,#7165,.T.);
#15941=EDGE_CURVE('',#12660,#12661,#7166,.T.);
#15942=EDGE_CURVE('',#12661,#12427,#7167,.T.);
#15943=EDGE_CURVE('',#12662,#12663,#7168,.T.);
#15944=EDGE_CURVE('',#12663,#12664,#7169,.T.);
#15945=EDGE_CURVE('',#12664,#12665,#7170,.T.);
#15946=EDGE_CURVE('',#12665,#12666,#7171,.T.);
#15947=EDGE_CURVE('',#12666,#12667,#7172,.T.);
#15948=EDGE_CURVE('',#12667,#12662,#7173,.T.);
#15949=EDGE_CURVE('',#12665,#12429,#7174,.T.);
#15950=EDGE_CURVE('',#12668,#12428,#7175,.T.);
#15951=EDGE_CURVE('',#12668,#12666,#7176,.T.);
#15952=EDGE_CURVE('',#12664,#12669,#7177,.T.);
#15953=EDGE_CURVE('',#12670,#12669,#7178,.T.);
#15954=EDGE_CURVE('',#12430,#12670,#7179,.T.);
#15955=EDGE_CURVE('',#12671,#12663,#7180,.T.);
#15956=EDGE_CURVE('',#12669,#12671,#7181,.T.);
#15957=EDGE_CURVE('',#12671,#12672,#7182,.T.);
#15958=EDGE_CURVE('',#12672,#12673,#7183,.T.);
#15959=EDGE_CURVE('',#12673,#12674,#7184,.T.);
#15960=EDGE_CURVE('',#12674,#12670,#7185,.T.);
#15961=EDGE_CURVE('',#12674,#12675,#7186,.T.);
#15962=EDGE_CURVE('',#12675,#12431,#7187,.T.);
#15963=EDGE_CURVE('',#12676,#12677,#7188,.T.);
#15964=EDGE_CURVE('',#12677,#12678,#7189,.T.);
#15965=EDGE_CURVE('',#12678,#12679,#7190,.T.);
#15966=EDGE_CURVE('',#12679,#12680,#7191,.T.);
#15967=EDGE_CURVE('',#12680,#12681,#7192,.T.);
#15968=EDGE_CURVE('',#12681,#12676,#7193,.T.);
#15969=EDGE_CURVE('',#12679,#12433,#7194,.T.);
#15970=EDGE_CURVE('',#12682,#12432,#7195,.T.);
#15971=EDGE_CURVE('',#12682,#12680,#7196,.T.);
#15972=EDGE_CURVE('',#12678,#12683,#7197,.T.);
#15973=EDGE_CURVE('',#12684,#12683,#7198,.T.);
#15974=EDGE_CURVE('',#12434,#12684,#7199,.T.);
#15975=EDGE_CURVE('',#12685,#12677,#7200,.T.);
#15976=EDGE_CURVE('',#12683,#12685,#7201,.T.);
#15977=EDGE_CURVE('',#12685,#12686,#7202,.T.);
#15978=EDGE_CURVE('',#12686,#12687,#7203,.T.);
#15979=EDGE_CURVE('',#12687,#12688,#7204,.T.);
#15980=EDGE_CURVE('',#12688,#12684,#7205,.T.);
#15981=EDGE_CURVE('',#12688,#12689,#7206,.T.);
#15982=EDGE_CURVE('',#12689,#12435,#7207,.T.);
#15983=EDGE_CURVE('',#12690,#12691,#7208,.T.);
#15984=EDGE_CURVE('',#12691,#12692,#7209,.T.);
#15985=EDGE_CURVE('',#12692,#12693,#7210,.T.);
#15986=EDGE_CURVE('',#12693,#12694,#7211,.T.);
#15987=EDGE_CURVE('',#12694,#12695,#7212,.T.);
#15988=EDGE_CURVE('',#12695,#12690,#7213,.T.);
#15989=EDGE_CURVE('',#12693,#12437,#7214,.T.);
#15990=EDGE_CURVE('',#12696,#12436,#7215,.T.);
#15991=EDGE_CURVE('',#12696,#12694,#7216,.T.);
#15992=EDGE_CURVE('',#12692,#12697,#7217,.T.);
#15993=EDGE_CURVE('',#12698,#12697,#7218,.T.);
#15994=EDGE_CURVE('',#12438,#12698,#7219,.T.);
#15995=EDGE_CURVE('',#12699,#12691,#7220,.T.);
#15996=EDGE_CURVE('',#12697,#12699,#7221,.T.);
#15997=EDGE_CURVE('',#12699,#12700,#7222,.T.);
#15998=EDGE_CURVE('',#12700,#12701,#7223,.T.);
#15999=EDGE_CURVE('',#12701,#12702,#7224,.T.);
#16000=EDGE_CURVE('',#12702,#12698,#7225,.T.);
#16001=EDGE_CURVE('',#12702,#12703,#7226,.T.);
#16002=EDGE_CURVE('',#12703,#12439,#7227,.T.);
#16003=EDGE_CURVE('',#12704,#12705,#7228,.T.);
#16004=EDGE_CURVE('',#12705,#12706,#7229,.T.);
#16005=EDGE_CURVE('',#12706,#12707,#7230,.T.);
#16006=EDGE_CURVE('',#12707,#12708,#7231,.T.);
#16007=EDGE_CURVE('',#12708,#12709,#7232,.T.);
#16008=EDGE_CURVE('',#12709,#12704,#7233,.T.);
#16009=EDGE_CURVE('',#12707,#12441,#7234,.T.);
#16010=EDGE_CURVE('',#12710,#12440,#7235,.T.);
#16011=EDGE_CURVE('',#12710,#12708,#7236,.T.);
#16012=EDGE_CURVE('',#12706,#12711,#7237,.T.);
#16013=EDGE_CURVE('',#12712,#12711,#7238,.T.);
#16014=EDGE_CURVE('',#12442,#12712,#7239,.T.);
#16015=EDGE_CURVE('',#12713,#12705,#7240,.T.);
#16016=EDGE_CURVE('',#12711,#12713,#7241,.T.);
#16017=EDGE_CURVE('',#12713,#12714,#7242,.T.);
#16018=EDGE_CURVE('',#12714,#12715,#7243,.T.);
#16019=EDGE_CURVE('',#12715,#12716,#7244,.T.);
#16020=EDGE_CURVE('',#12716,#12712,#7245,.T.);
#16021=EDGE_CURVE('',#12716,#12717,#7246,.T.);
#16022=EDGE_CURVE('',#12717,#12443,#7247,.T.);
#16023=EDGE_CURVE('',#12718,#12089,#7248,.T.);
#16024=EDGE_CURVE('',#12092,#12719,#7249,.T.);
#16025=EDGE_CURVE('',#12719,#12720,#7250,.T.);
#16026=EDGE_CURVE('',#12720,#12718,#7251,.T.);
#16027=EDGE_CURVE('',#12720,#12721,#7252,.T.);
#16028=EDGE_CURVE('',#12722,#12721,#7253,.T.);
#16029=EDGE_CURVE('',#12722,#12723,#7254,.T.);
#16030=EDGE_CURVE('',#12723,#12718,#7255,.T.);
#16031=EDGE_CURVE('',#12724,#12719,#7256,.T.);
#16032=EDGE_CURVE('',#12721,#12724,#7257,.T.);
#16033=EDGE_CURVE('',#12724,#12444,#7258,.T.);
#16034=EDGE_CURVE('',#12717,#12724,#7259,.T.);
#16035=EDGE_CURVE('',#12725,#12717,#7260,.T.);
#16036=EDGE_CURVE('',#12721,#12725,#7261,.T.);
#16037=EDGE_CURVE('',#12725,#12715,#7262,.T.);
#16038=EDGE_CURVE('',#12703,#12710,#7263,.T.);
#16039=EDGE_CURVE('',#12726,#12710,#7264,.T.);
#16040=EDGE_CURVE('',#12709,#12726,#7265,.T.);
#16041=EDGE_CURVE('',#12727,#12703,#7266,.T.);
#16042=EDGE_CURVE('',#12726,#12727,#7267,.T.);
#16043=EDGE_CURVE('',#12727,#12701,#7268,.T.);
#16044=EDGE_CURVE('',#12689,#12696,#7269,.T.);
#16045=EDGE_CURVE('',#12728,#12696,#7270,.T.);
#16046=EDGE_CURVE('',#12695,#12728,#7271,.T.);
#16047=EDGE_CURVE('',#12729,#12689,#7272,.T.);
#16048=EDGE_CURVE('',#12728,#12729,#7273,.T.);
#16049=EDGE_CURVE('',#12729,#12687,#7274,.T.);
#16050=EDGE_CURVE('',#12675,#12682,#7275,.T.);
#16051=EDGE_CURVE('',#12730,#12682,#7276,.T.);
#16052=EDGE_CURVE('',#12681,#12730,#7277,.T.);
#16053=EDGE_CURVE('',#12731,#12675,#7278,.T.);
#16054=EDGE_CURVE('',#12730,#12731,#7279,.T.);
#16055=EDGE_CURVE('',#12731,#12673,#7280,.T.);
#16056=EDGE_CURVE('',#12661,#12668,#7281,.T.);
#16057=EDGE_CURVE('',#12732,#12668,#7282,.T.);
#16058=EDGE_CURVE('',#12667,#12732,#7283,.T.);
#16059=EDGE_CURVE('',#12733,#12661,#7284,.T.);
#16060=EDGE_CURVE('',#12732,#12733,#7285,.T.);
#16061=EDGE_CURVE('',#12733,#12659,#7286,.T.);
#16062=EDGE_CURVE('',#12647,#12654,#7287,.T.);
#16063=EDGE_CURVE('',#12734,#12654,#7288,.T.);
#16064=EDGE_CURVE('',#12653,#12734,#7289,.T.);
#16065=EDGE_CURVE('',#12735,#12647,#7290,.T.);
#16066=EDGE_CURVE('',#12734,#12735,#7291,.T.);
#16067=EDGE_CURVE('',#12735,#12645,#7292,.T.);
#16068=EDGE_CURVE('',#12419,#12064,#7293,.F.);
#16069=EDGE_CURVE('',#12064,#12640,#7294,.T.);
#16070=EDGE_CURVE('',#12736,#12640,#7295,.T.);
#16071=EDGE_CURVE('',#12639,#12736,#7296,.T.);
#16072=EDGE_CURVE('',#12736,#12063,#7297,.T.);
#16073=EDGE_CURVE('',#12418,#12057,#7298,.T.);
#16074=EDGE_CURVE('',#12345,#12737,#7299,.T.);
#16075=EDGE_CURVE('',#12737,#12738,#7300,.T.);
#16076=EDGE_CURVE('',#12738,#12482,#7301,.T.);
#16077=EDGE_CURVE('',#12738,#12739,#7302,.T.);
#16078=EDGE_CURVE('',#12739,#12481,#7303,.T.);
#16079=EDGE_CURVE('',#12739,#12740,#7304,.T.);
#16080=EDGE_CURVE('',#12740,#12350,#7305,.T.);
#16081=EDGE_CURVE('',#12741,#12737,#7306,.T.);
#16082=EDGE_CURVE('',#12742,#12741,#7307,.T.);
#16083=EDGE_CURVE('',#12743,#12742,#7308,.T.);
#16084=EDGE_CURVE('',#12744,#12743,#7309,.T.);
#16085=EDGE_CURVE('',#12745,#12744,#7310,.T.);
#16086=EDGE_CURVE('',#12746,#12745,#7311,.T.);
#16087=EDGE_CURVE('',#12747,#12746,#7312,.T.);
#16088=EDGE_CURVE('',#12748,#12747,#7313,.T.);
#16089=EDGE_CURVE('',#12495,#12748,#7314,.T.);
#16090=EDGE_CURVE('',#12749,#12496,#7315,.T.);
#16091=EDGE_CURVE('',#12248,#12749,#7316,.T.);
#16092=EDGE_CURVE('',#12750,#12247,#7317,.T.);
#16093=EDGE_CURVE('',#12751,#12750,#7318,.T.);
#16094=EDGE_CURVE('',#12752,#12751,#7319,.T.);
#16095=EDGE_CURVE('',#12753,#12752,#7320,.T.);
#16096=EDGE_CURVE('',#12754,#12753,#7321,.T.);
#16097=EDGE_CURVE('',#12755,#12754,#7322,.T.);
#16098=EDGE_CURVE('',#12756,#12755,#7323,.T.);
#16099=EDGE_CURVE('',#12757,#12756,#7324,.T.);
#16100=EDGE_CURVE('',#12202,#12757,#7325,.T.);
#16101=EDGE_CURVE('',#12758,#12203,#7326,.T.);
#16102=EDGE_CURVE('',#12759,#12758,#7327,.T.);
#16103=EDGE_CURVE('',#12760,#12759,#7328,.T.);
#16104=EDGE_CURVE('',#12761,#12760,#7329,.T.);
#16105=EDGE_CURVE('',#12762,#12761,#7330,.T.);
#16106=EDGE_CURVE('',#12044,#12762,#7331,.T.);
#16107=EDGE_CURVE('',#12763,#12043,#7332,.T.);
#16108=EDGE_CURVE('',#12764,#12763,#7333,.T.);
#16109=EDGE_CURVE('',#12765,#12764,#7334,.T.);
#16110=EDGE_CURVE('',#12766,#12765,#7335,.T.);
#16111=EDGE_CURVE('',#12767,#12766,#7336,.T.);
#16112=EDGE_CURVE('',#12768,#12767,#7337,.T.);
#16113=EDGE_CURVE('',#12769,#12768,#7338,.T.);
#16114=EDGE_CURVE('',#12770,#12769,#7339,.T.);
#16115=EDGE_CURVE('',#12619,#12770,#7340,.T.);
#16116=EDGE_CURVE('',#12771,#12618,#7341,.T.);
#16117=EDGE_CURVE('',#12772,#12771,#7342,.T.);
#16118=EDGE_CURVE('',#12773,#12772,#7343,.T.);
#16119=EDGE_CURVE('',#12774,#12773,#7344,.T.);
#16120=EDGE_CURVE('',#12775,#12774,#7345,.T.);
#16121=EDGE_CURVE('',#12776,#12775,#7346,.T.);
#16122=EDGE_CURVE('',#12777,#12776,#7347,.T.);
#16123=EDGE_CURVE('',#12778,#12777,#7348,.T.);
#16124=EDGE_CURVE('',#12584,#12778,#7349,.T.);
#16125=EDGE_CURVE('',#12779,#12585,#7350,.T.);
#16126=EDGE_CURVE('',#12780,#12779,#7351,.T.);
#16127=EDGE_CURVE('',#12781,#12780,#7352,.T.);
#16128=EDGE_CURVE('',#12782,#12781,#7353,.T.);
#16129=EDGE_CURVE('',#12783,#12782,#7354,.T.);
#16130=EDGE_CURVE('',#12784,#12783,#7355,.T.);
#16131=EDGE_CURVE('',#12785,#12784,#7356,.T.);
#16132=EDGE_CURVE('',#12786,#12785,#7357,.T.);
#16133=EDGE_CURVE('',#12787,#12786,#7358,.T.);
#16134=EDGE_CURVE('',#12788,#12787,#7359,.T.);
#16135=EDGE_CURVE('',#12789,#12788,#7360,.T.);
#16136=EDGE_CURVE('',#12790,#12789,#7361,.T.);
#16137=EDGE_CURVE('',#12791,#12790,#7362,.T.);
#16138=EDGE_CURVE('',#12056,#12791,#7363,.T.);
#16139=EDGE_CURVE('',#12792,#12055,#7364,.T.);
#16140=EDGE_CURVE('',#12793,#12792,#7365,.T.);
#16141=EDGE_CURVE('',#12794,#12793,#7366,.T.);
#16142=EDGE_CURVE('',#12795,#12794,#7367,.T.);
#16143=EDGE_CURVE('',#12796,#12795,#7368,.T.);
#16144=EDGE_CURVE('',#12797,#12796,#7369,.T.);
#16145=EDGE_CURVE('',#12798,#12797,#7370,.T.);
#16146=EDGE_CURVE('',#12799,#12798,#7371,.T.);
#16147=EDGE_CURVE('',#12723,#12799,#7372,.T.);
#16148=EDGE_CURVE('',#12800,#12722,#7373,.T.);
#16149=EDGE_CURVE('',#12801,#12800,#7374,.T.);
#16150=EDGE_CURVE('',#12802,#12801,#7375,.T.);
#16151=EDGE_CURVE('',#12803,#12802,#7376,.T.);
#16152=EDGE_CURVE('',#12804,#12803,#7377,.T.);
#16153=EDGE_CURVE('',#12805,#12804,#7378,.T.);
#16154=EDGE_CURVE('',#12806,#12805,#7379,.T.);
#16155=EDGE_CURVE('',#12807,#12806,#7380,.T.);
#16156=EDGE_CURVE('',#12808,#12807,#7381,.T.);
#16157=EDGE_CURVE('',#12809,#12808,#7382,.T.);
#16158=EDGE_CURVE('',#12810,#12809,#7383,.T.);
#16159=EDGE_CURVE('',#12811,#12810,#7384,.T.);
#16160=EDGE_CURVE('',#12812,#12811,#7385,.T.);
#16161=EDGE_CURVE('',#12813,#12812,#7386,.T.);
#16162=EDGE_CURVE('',#12814,#12813,#7387,.T.);
#16163=EDGE_CURVE('',#12815,#12814,#7388,.T.);
#16164=EDGE_CURVE('',#12816,#12815,#7389,.T.);
#16165=EDGE_CURVE('',#12817,#12816,#7390,.T.);
#16166=EDGE_CURVE('',#12818,#12817,#7391,.T.);
#16167=EDGE_CURVE('',#12819,#12818,#7392,.T.);
#16168=EDGE_CURVE('',#12820,#12819,#7393,.T.);
#16169=EDGE_CURVE('',#12821,#12820,#7394,.T.);
#16170=EDGE_CURVE('',#12822,#12821,#7395,.T.);
#16171=EDGE_CURVE('',#12823,#12822,#7396,.T.);
#16172=EDGE_CURVE('',#12066,#12823,#7397,.T.);
#16173=EDGE_CURVE('',#12824,#12293,#7398,.T.);
#16174=EDGE_CURVE('',#12825,#12824,#7399,.T.);
#16175=EDGE_CURVE('',#12826,#12825,#7400,.T.);
#16176=EDGE_CURVE('',#12827,#12826,#7401,.T.);
#16177=EDGE_CURVE('',#12828,#12827,#7402,.T.);
#16178=EDGE_CURVE('',#12829,#12828,#7403,.T.);
#16179=EDGE_CURVE('',#12830,#12829,#7404,.T.);
#16180=EDGE_CURVE('',#12831,#12830,#7405,.T.);
#16181=EDGE_CURVE('',#12081,#12831,#7406,.T.);
#16182=EDGE_CURVE('',#12832,#12080,#7407,.T.);
#16183=EDGE_CURVE('',#12833,#12832,#7408,.T.);
#16184=EDGE_CURVE('',#12834,#12833,#7409,.T.);
#16185=EDGE_CURVE('',#12835,#12834,#7410,.T.);
#16186=EDGE_CURVE('',#12836,#12835,#7411,.T.);
#16187=EDGE_CURVE('',#12837,#12836,#7412,.T.);
#16188=EDGE_CURVE('',#12838,#12837,#7413,.T.);
#16189=EDGE_CURVE('',#12839,#12838,#7414,.T.);
#16190=EDGE_CURVE('',#12840,#12839,#7415,.T.);
#16191=EDGE_CURVE('',#12841,#12840,#7416,.T.);
#16192=EDGE_CURVE('',#12842,#12841,#7417,.T.);
#16193=EDGE_CURVE('',#12843,#12842,#7418,.T.);
#16194=EDGE_CURVE('',#12740,#12843,#7419,.T.);
#16195=EDGE_CURVE('',#12844,#12844,#10877,.T.);
#16196=EDGE_CURVE('',#12741,#12332,#7420,.T.);
#16197=EDGE_CURVE('',#12363,#12843,#7421,.T.);
#16198=EDGE_CURVE('',#12842,#12480,#7422,.T.);
#16199=EDGE_CURVE('',#12841,#12479,#7423,.T.);
#16200=EDGE_CURVE('',#12840,#12368,#7424,.T.);
#16201=EDGE_CURVE('',#12381,#12839,#7425,.T.);
#16202=EDGE_CURVE('',#12838,#12478,#7426,.T.);
#16203=EDGE_CURVE('',#12837,#12477,#7427,.T.);
#16204=EDGE_CURVE('',#12836,#12386,#7428,.T.);
#16205=EDGE_CURVE('',#12399,#12835,#7429,.T.);
#16206=EDGE_CURVE('',#12834,#12476,#7430,.T.);
#16207=EDGE_CURVE('',#12833,#12411,#7431,.T.);
#16208=EDGE_CURVE('',#12832,#12404,#7432,.T.);
#16209=EDGE_CURVE('',#12831,#12417,#7433,.T.);
#16210=EDGE_CURVE('',#12830,#12252,#7434,.T.);
#16211=EDGE_CURVE('',#12072,#12405,#7435,.T.);
#16212=EDGE_CURVE('',#12265,#12829,#7436,.T.);
#16213=EDGE_CURVE('',#12828,#12416,#7437,.T.);
#16214=EDGE_CURVE('',#12827,#12415,#7438,.T.);
#16215=EDGE_CURVE('',#12826,#12270,#7439,.T.);
#16216=EDGE_CURVE('',#12283,#12825,#7440,.T.);
#16217=EDGE_CURVE('',#12824,#12414,#7441,.F.);
#16218=EDGE_CURVE('',#12823,#12736,#7442,.T.);
#16219=EDGE_CURVE('',#12822,#12634,#7443,.T.);
#16220=EDGE_CURVE('',#12644,#12821,#7444,.T.);
#16221=EDGE_CURVE('',#12820,#12735,#7445,.T.);
#16222=EDGE_CURVE('',#12819,#12734,#7446,.T.);
#16223=EDGE_CURVE('',#12818,#12648,#7447,.T.);
#16224=EDGE_CURVE('',#12658,#12817,#7448,.T.);
#16225=EDGE_CURVE('',#12816,#12733,#7449,.T.);
#16226=EDGE_CURVE('',#12815,#12732,#7450,.T.);
#16227=EDGE_CURVE('',#12814,#12662,#7451,.T.);
#16228=EDGE_CURVE('',#12672,#12813,#7452,.T.);
#16229=EDGE_CURVE('',#12812,#12731,#7453,.T.);
#16230=EDGE_CURVE('',#12811,#12730,#7454,.T.);
#16231=EDGE_CURVE('',#12810,#12676,#7455,.T.);
#16232=EDGE_CURVE('',#12686,#12809,#7456,.T.);
#16233=EDGE_CURVE('',#12808,#12729,#7457,.T.);
#16234=EDGE_CURVE('',#12807,#12728,#7458,.T.);
#16235=EDGE_CURVE('',#12806,#12690,#7459,.T.);
#16236=EDGE_CURVE('',#12700,#12805,#7460,.T.);
#16237=EDGE_CURVE('',#12804,#12727,#7461,.T.);
#16238=EDGE_CURVE('',#12803,#12726,#7462,.T.);
#16239=EDGE_CURVE('',#12802,#12704,#7463,.T.);
#16240=EDGE_CURVE('',#12714,#12801,#7464,.T.);
#16241=EDGE_CURVE('',#12800,#12725,#7465,.T.);
#16242=EDGE_CURVE('',#12085,#12799,#7466,.T.);
#16243=EDGE_CURVE('',#12798,#12633,#7467,.T.);
#16244=EDGE_CURVE('',#12797,#12632,#7468,.T.);
#16245=EDGE_CURVE('',#12796,#12095,#7469,.T.);
#16246=EDGE_CURVE('',#12108,#12795,#7470,.T.);
#16247=EDGE_CURVE('',#12794,#12631,#7471,.T.);
#16248=EDGE_CURVE('',#12793,#12120,#7472,.T.);
#16249=EDGE_CURVE('',#12792,#12113,#7473,.T.);
#16250=EDGE_CURVE('',#12791,#12630,#7474,.T.);
#16251=EDGE_CURVE('',#12790,#12525,#7475,.T.);
#16252=EDGE_CURVE('',#12047,#12114,#7476,.T.);
#16253=EDGE_CURVE('',#12535,#12789,#7477,.T.);
#16254=EDGE_CURVE('',#12788,#12629,#7478,.T.);
#16255=EDGE_CURVE('',#12787,#12628,#7479,.T.);
#16256=EDGE_CURVE('',#12786,#12539,#7480,.T.);
#16257=EDGE_CURVE('',#12549,#12785,#7481,.T.);
#16258=EDGE_CURVE('',#12784,#12627,#7482,.T.);
#16259=EDGE_CURVE('',#12783,#12626,#7483,.T.);
#16260=EDGE_CURVE('',#12782,#12553,#7484,.T.);
#16261=EDGE_CURVE('',#12563,#12781,#7485,.T.);
#16262=EDGE_CURVE('',#12780,#12625,#7486,.T.);
#16263=EDGE_CURVE('',#12779,#12574,#7487,.F.);
#16264=EDGE_CURVE('',#12778,#12624,#7488,.T.);
#16265=EDGE_CURVE('',#12777,#12586,#7489,.T.);
#16266=EDGE_CURVE('',#12596,#12776,#7490,.T.);
#16267=EDGE_CURVE('',#12775,#12623,#7491,.T.);
#16268=EDGE_CURVE('',#12774,#12622,#7492,.T.);
#16269=EDGE_CURVE('',#12773,#12600,#7493,.T.);
#16270=EDGE_CURVE('',#12610,#12772,#7494,.T.);
#16271=EDGE_CURVE('',#12771,#12621,#7495,.T.);
#16272=EDGE_CURVE('',#12126,#12770,#7496,.T.);
#16273=EDGE_CURVE('',#12769,#12524,#7497,.T.);
#16274=EDGE_CURVE('',#12768,#12523,#7498,.T.);
#16275=EDGE_CURVE('',#12767,#12136,#7499,.T.);
#16276=EDGE_CURVE('',#12149,#12766,#7500,.T.);
#16277=EDGE_CURVE('',#12765,#12522,#7501,.T.);
#16278=EDGE_CURVE('',#12764,#12161,#7502,.T.);
#16279=EDGE_CURVE('',#12763,#12154,#7503,.T.);
#16280=EDGE_CURVE('',#12762,#12521,#7504,.T.);
#16281=EDGE_CURVE('',#12761,#12164,#7505,.T.);
#16282=EDGE_CURVE('',#12035,#12155,#7506,.T.);
#16283=EDGE_CURVE('',#12177,#12760,#7507,.T.);
#16284=EDGE_CURVE('',#12759,#12520,#7508,.F.);
#16285=EDGE_CURVE('',#12758,#12189,#7509,.T.);
#16286=EDGE_CURVE('',#12757,#12519,#7510,.T.);
#16287=EDGE_CURVE('',#12756,#12204,#7511,.T.);
#16288=EDGE_CURVE('',#12217,#12755,#7512,.T.);
#16289=EDGE_CURVE('',#12754,#12518,#7513,.T.);
#16290=EDGE_CURVE('',#12753,#12517,#7514,.T.);
#16291=EDGE_CURVE('',#12752,#12222,#7515,.T.);
#16292=EDGE_CURVE('',#12235,#12751,#7516,.T.);
#16293=EDGE_CURVE('',#12750,#12516,#7517,.T.);
#16294=EDGE_CURVE('',#12304,#12845,#7518,.T.);
#16295=EDGE_CURVE('',#12845,#12749,#7519,.T.);
#16296=EDGE_CURVE('',#12497,#12748,#7520,.T.);
#16297=EDGE_CURVE('',#12747,#12515,#7521,.T.);
#16298=EDGE_CURVE('',#12746,#12514,#7522,.T.);
#16299=EDGE_CURVE('',#12745,#12501,#7523,.T.);
#16300=EDGE_CURVE('',#12511,#12744,#7524,.T.);
#16301=EDGE_CURVE('',#12743,#12485,#7525,.T.);
#16302=EDGE_CURVE('',#12742,#12484,#7526,.T.);
#16303=EDGE_CURVE('',#12846,#12847,#7527,.T.);
#16304=EDGE_CURVE('',#12847,#12848,#1395,.T.);
#16305=EDGE_CURVE('',#12848,#12847,#1396,.T.);
#16306=EDGE_CURVE('',#12846,#12846,#1397,.T.);
#16307=EDGE_CURVE('',#12849,#12849,#10878,.T.);
#16308=EDGE_CURVE('',#12849,#12848,#7528,.T.);
#16309=EDGE_CURVE('',#12850,#12850,#10879,.T.);
#16310=EDGE_CURVE('',#12850,#12851,#7529,.T.);
#16311=EDGE_CURVE('',#12851,#12851,#10880,.T.);
#16312=EDGE_CURVE('',#12844,#12849,#7530,.T.);
#16313=EDGE_CURVE('',#12303,#12850,#7531,.T.);
#16314=EDGE_CURVE('',#12851,#12852,#7532,.T.);
#16315=EDGE_CURVE('',#12242,#12853,#7533,.T.);
#16316=EDGE_CURVE('',#12853,#12315,#7534,.T.);
#16317=EDGE_CURVE('',#12288,#12058,#7535,.T.);
#16318=EDGE_CURVE('',#12854,#12241,#7536,.T.);
#16319=EDGE_CURVE('',#12853,#12854,#7537,.T.);
#16320=EDGE_CURVE('',#12845,#12854,#7538,.T.);
#16321=EDGE_CURVE('',#12486,#12855,#7539,.T.);
#16322=EDGE_CURVE('',#12855,#12321,#7540,.T.);
#16323=EDGE_CURVE('',#12298,#12316,#7541,.T.);
#16324=EDGE_CURVE('',#12855,#12491,#7542,.T.);
#16325=EDGE_CURVE('',#12856,#12857,#7543,.F.);
#16326=EDGE_CURVE('',#12857,#12858,#7544,.T.);
#16327=EDGE_CURVE('',#12858,#12859,#7545,.F.);
#16328=EDGE_CURVE('',#12859,#12856,#7546,.T.);
#16329=EDGE_CURVE('',#12860,#12857,#10881,.T.);
#16330=EDGE_CURVE('',#12861,#12860,#7547,.T.);
#16331=EDGE_CURVE('',#12861,#12858,#10882,.T.);
#16332=EDGE_CURVE('',#12862,#12861,#7548,.F.);
#16333=EDGE_CURVE('',#12860,#12863,#7549,.F.);
#16334=EDGE_CURVE('',#12863,#12862,#7550,.T.);
#16335=EDGE_CURVE('',#12864,#12865,#7551,.F.);
#16336=EDGE_CURVE('',#12865,#12866,#7552,.T.);
#16337=EDGE_CURVE('',#12866,#12867,#7553,.F.);
#16338=EDGE_CURVE('',#12867,#12864,#7554,.T.);
#16339=EDGE_CURVE('',#12865,#12868,#10883,.T.);
#16340=EDGE_CURVE('',#12869,#12868,#7555,.T.);
#16341=EDGE_CURVE('',#12866,#12869,#10884,.T.);
#16342=EDGE_CURVE('',#12870,#12869,#7556,.F.);
#16343=EDGE_CURVE('',#12868,#12871,#7557,.F.);
#16344=EDGE_CURVE('',#12871,#12870,#7558,.T.);
#16345=EDGE_CURVE('',#12872,#12873,#7559,.F.);
#16346=EDGE_CURVE('',#12873,#12874,#7560,.T.);
#16347=EDGE_CURVE('',#12874,#12875,#7561,.F.);
#16348=EDGE_CURVE('',#12875,#12872,#7562,.T.);
#16349=EDGE_CURVE('',#12876,#12873,#10885,.T.);
#16350=EDGE_CURVE('',#12877,#12876,#7563,.T.);
#16351=EDGE_CURVE('',#12877,#12874,#10886,.T.);
#16352=EDGE_CURVE('',#12878,#12877,#7564,.F.);
#16353=EDGE_CURVE('',#12876,#12879,#7565,.F.);
#16354=EDGE_CURVE('',#12879,#12878,#7566,.T.);
#16355=EDGE_CURVE('',#12880,#12881,#7567,.F.);
#16356=EDGE_CURVE('',#12881,#12882,#7568,.T.);
#16357=EDGE_CURVE('',#12882,#12883,#7569,.F.);
#16358=EDGE_CURVE('',#12883,#12880,#7570,.T.);
#16359=EDGE_CURVE('',#12881,#12884,#10887,.T.);
#16360=EDGE_CURVE('',#12885,#12884,#7571,.T.);
#16361=EDGE_CURVE('',#12882,#12885,#10888,.T.);
#16362=EDGE_CURVE('',#12886,#12885,#7572,.F.);
#16363=EDGE_CURVE('',#12884,#12887,#7573,.F.);
#16364=EDGE_CURVE('',#12887,#12886,#7574,.T.);
#16365=EDGE_CURVE('',#12888,#12889,#7575,.F.);
#16366=EDGE_CURVE('',#12889,#12890,#7576,.T.);
#16367=EDGE_CURVE('',#12890,#12891,#7577,.F.);
#16368=EDGE_CURVE('',#12891,#12888,#7578,.T.);
#16369=EDGE_CURVE('',#12892,#12889,#10889,.T.);
#16370=EDGE_CURVE('',#12893,#12892,#7579,.T.);
#16371=EDGE_CURVE('',#12893,#12890,#10890,.T.);
#16372=EDGE_CURVE('',#12894,#12893,#7580,.F.);
#16373=EDGE_CURVE('',#12892,#12895,#7581,.F.);
#16374=EDGE_CURVE('',#12895,#12894,#7582,.T.);
#16375=EDGE_CURVE('',#12896,#12897,#7583,.F.);
#16376=EDGE_CURVE('',#12897,#12898,#7584,.T.);
#16377=EDGE_CURVE('',#12898,#12899,#7585,.F.);
#16378=EDGE_CURVE('',#12899,#12896,#7586,.T.);
#16379=EDGE_CURVE('',#12897,#12900,#10891,.T.);
#16380=EDGE_CURVE('',#12901,#12900,#7587,.T.);
#16381=EDGE_CURVE('',#12898,#12901,#10892,.T.);
#16382=EDGE_CURVE('',#12902,#12901,#7588,.F.);
#16383=EDGE_CURVE('',#12900,#12903,#7589,.F.);
#16384=EDGE_CURVE('',#12903,#12902,#7590,.T.);
#16385=EDGE_CURVE('',#12904,#12905,#7591,.F.);
#16386=EDGE_CURVE('',#12905,#12906,#7592,.T.);
#16387=EDGE_CURVE('',#12906,#12907,#7593,.F.);
#16388=EDGE_CURVE('',#12907,#12904,#7594,.T.);
#16389=EDGE_CURVE('',#12905,#12908,#10893,.T.);
#16390=EDGE_CURVE('',#12909,#12908,#7595,.T.);
#16391=EDGE_CURVE('',#12906,#12909,#10894,.T.);
#16392=EDGE_CURVE('',#12910,#12909,#7596,.F.);
#16393=EDGE_CURVE('',#12908,#12911,#7597,.F.);
#16394=EDGE_CURVE('',#12911,#12910,#7598,.T.);
#16395=EDGE_CURVE('',#12912,#12913,#7599,.F.);
#16396=EDGE_CURVE('',#12913,#12914,#7600,.T.);
#16397=EDGE_CURVE('',#12914,#12915,#7601,.F.);
#16398=EDGE_CURVE('',#12915,#12912,#7602,.T.);
#16399=EDGE_CURVE('',#12913,#12916,#10895,.T.);
#16400=EDGE_CURVE('',#12917,#12916,#7603,.T.);
#16401=EDGE_CURVE('',#12914,#12917,#10896,.T.);
#16402=EDGE_CURVE('',#12918,#12917,#7604,.F.);
#16403=EDGE_CURVE('',#12916,#12919,#7605,.F.);
#16404=EDGE_CURVE('',#12919,#12918,#7606,.T.);
#16405=EDGE_CURVE('',#12919,#12912,#10897,.T.);
#16406=EDGE_CURVE('',#12915,#12918,#10898,.T.);
#16407=EDGE_CURVE('',#12911,#12920,#10899,.T.);
#16408=EDGE_CURVE('',#12920,#12904,#10900,.T.);
#16409=EDGE_CURVE('',#12907,#12921,#10901,.T.);
#16410=EDGE_CURVE('',#12921,#12910,#10902,.T.);
#16411=EDGE_CURVE('',#12903,#12896,#10903,.T.);
#16412=EDGE_CURVE('',#12899,#12902,#10904,.T.);
#16413=EDGE_CURVE('',#12895,#12888,#10905,.T.);
#16414=EDGE_CURVE('',#12891,#12894,#10906,.T.);
#16415=EDGE_CURVE('',#12887,#12880,#10907,.T.);
#16416=EDGE_CURVE('',#12883,#12886,#10908,.T.);
#16417=EDGE_CURVE('',#12879,#12872,#10909,.T.);
#16418=EDGE_CURVE('',#12875,#12878,#10910,.T.);
#16419=EDGE_CURVE('',#12871,#12864,#10911,.T.);
#16420=EDGE_CURVE('',#12867,#12870,#10912,.T.);
#16421=EDGE_CURVE('',#12863,#12856,#10913,.T.);
#16422=EDGE_CURVE('',#12859,#12862,#10914,.T.);
#16423=EDGE_CURVE('',#12922,#12922,#10915,.T.);
#16424=EDGE_CURVE('',#12922,#12923,#7607,.T.);
#16425=EDGE_CURVE('',#12923,#12923,#10916,.T.);
#16426=EDGE_CURVE('',#12924,#12924,#10917,.T.);
#16427=EDGE_CURVE('',#12924,#12925,#7608,.T.);
#16428=EDGE_CURVE('',#12925,#12925,#10918,.T.);
#16429=EDGE_CURVE('',#12925,#12926,#7609,.T.);
#16430=EDGE_CURVE('',#12927,#12927,#10919,.T.);
#16431=EDGE_CURVE('',#12928,#12928,#10920,.T.);
#16432=EDGE_CURVE('',#12928,#12927,#7610,.T.);
#16433=EDGE_CURVE('',#12929,#12929,#10921,.T.);
#16434=EDGE_CURVE('',#12929,#12920,#7611,.T.);
#16435=EDGE_CURVE('',#12921,#12928,#7612,.T.);
#16436=EDGE_CURVE('',#12930,#12929,#10922,.T.);
#16437=EDGE_CURVE('',#12931,#12932,#10923,.T.);
#16438=EDGE_CURVE('',#12932,#12933,#10924,.T.);
#16439=EDGE_CURVE('',#12933,#12934,#1398,.T.);
#16440=EDGE_CURVE('',#12934,#12935,#10925,.T.);
#16441=EDGE_CURVE('',#12935,#12931,#1399,.T.);
#16442=EDGE_CURVE('',#12936,#12937,#7613,.T.);
#16443=EDGE_CURVE('',#12937,#12934,#10926,.T.);
#16444=EDGE_CURVE('',#12933,#12938,#7614,.T.);
#16445=EDGE_CURVE('',#12938,#12939,#1400,.T.);
#16446=EDGE_CURVE('',#12939,#12936,#10927,.T.);
#16447=EDGE_CURVE('',#12940,#12931,#7615,.T.);
#16448=EDGE_CURVE('',#12935,#12941,#10928,.T.);
#16449=EDGE_CURVE('',#12941,#12942,#7616,.T.);
#16450=EDGE_CURVE('',#12942,#12943,#10929,.T.);
#16451=EDGE_CURVE('',#12943,#12940,#1401,.T.);
#16452=EDGE_CURVE('',#12938,#12944,#10930,.T.);
#16453=EDGE_CURVE('',#12944,#12940,#10931,.T.);
#16454=EDGE_CURVE('',#12943,#12939,#10932,.T.);
#16455=EDGE_CURVE('',#12945,#12941,#7617,.T.);
#16456=EDGE_CURVE('',#12946,#12945,#7618,.T.);
#16457=EDGE_CURVE('',#12946,#12942,#7619,.T.);
#16458=EDGE_CURVE('',#12937,#12947,#7620,.T.);
#16459=EDGE_CURVE('',#12948,#12947,#7621,.T.);
#16460=EDGE_CURVE('',#12949,#12948,#7622,.T.);
#16461=EDGE_CURVE('',#12950,#12949,#10933,.F.);
#16462=EDGE_CURVE('',#12945,#12950,#7623,.T.);
#16463=EDGE_CURVE('',#12951,#12951,#10934,.T.);
#16464=EDGE_CURVE('',#12951,#12944,#7624,.T.);
#16465=EDGE_CURVE('',#12932,#12952,#7625,.T.);
#16466=EDGE_CURVE('',#12952,#12952,#10935,.T.);
#16467=EDGE_CURVE('',#12953,#12954,#103,.T.);
#16468=EDGE_CURVE('',#12954,#12955,#7626,.T.);
#16469=EDGE_CURVE('',#12955,#12956,#104,.T.);
#16470=EDGE_CURVE('',#12956,#12957,#7627,.T.);
#16471=EDGE_CURVE('',#12957,#12953,#105,.T.);
#16472=EDGE_CURVE('',#12958,#12956,#7628,.T.);
#16473=EDGE_CURVE('',#12958,#12959,#7629,.T.);
#16474=EDGE_CURVE('',#12960,#12959,#7630,.T.);
#16475=EDGE_CURVE('',#12961,#12960,#7631,.T.);
#16476=EDGE_CURVE('',#12957,#12961,#7632,.T.);
#16477=EDGE_CURVE('',#12955,#12962,#7633,.T.);
#16478=EDGE_CURVE('',#12963,#12962,#7634,.T.);
#16479=EDGE_CURVE('',#12963,#12956,#7635,.T.);
#16480=EDGE_CURVE('',#12964,#12954,#7636,.T.);
#16481=EDGE_CURVE('',#12962,#12964,#7637,.T.);
#16482=EDGE_CURVE('',#12965,#12966,#106,.T.);
#16483=EDGE_CURVE('',#12966,#12967,#7638,.T.);
#16484=EDGE_CURVE('',#12967,#12968,#107,.T.);
#16485=EDGE_CURVE('',#12968,#12969,#108,.T.);
#16486=EDGE_CURVE('',#12969,#12965,#7639,.T.);
#16487=EDGE_CURVE('',#12965,#12970,#7640,.T.);
#16488=EDGE_CURVE('',#12970,#12971,#7641,.T.);
#16489=EDGE_CURVE('',#12971,#12966,#7642,.T.);
#16490=EDGE_CURVE('',#12972,#12969,#7643,.T.);
#16491=EDGE_CURVE('',#12973,#12972,#7644,.T.);
#16492=EDGE_CURVE('',#12974,#12973,#7645,.T.);
#16493=EDGE_CURVE('',#12975,#12974,#7646,.T.);
#16494=EDGE_CURVE('',#12965,#12975,#7647,.T.);
#16495=EDGE_CURVE('',#12968,#12976,#109,.T.);
#16496=EDGE_CURVE('',#12976,#12977,#7648,.T.);
#16497=EDGE_CURVE('',#12977,#12972,#10936,.F.);
#16498=EDGE_CURVE('',#12961,#12978,#10937,.F.);
#16499=EDGE_CURVE('',#12979,#12961,#10938,.F.);
#16500=EDGE_CURVE('',#12978,#12979,#10939,.F.);
#16501=EDGE_CURVE('',#12980,#12979,#7649,.T.);
#16502=EDGE_CURVE('',#12960,#12980,#110,.T.);
#16503=EDGE_CURVE('',#12972,#12981,#10940,.F.);
#16504=EDGE_CURVE('',#12981,#12977,#10941,.F.);
#16505=EDGE_CURVE('',#12982,#12983,#7650,.T.);
#16506=EDGE_CURVE('',#12983,#12984,#111,.T.);
#16507=EDGE_CURVE('',#12984,#12985,#7651,.T.);
#16508=EDGE_CURVE('',#12985,#12982,#112,.T.);
#16509=EDGE_CURVE('',#12983,#12981,#7652,.T.);
#16510=EDGE_CURVE('',#12977,#12984,#7653,.T.);
#16511=EDGE_CURVE('',#12981,#12986,#7654,.T.);
#16512=EDGE_CURVE('',#12986,#12973,#113,.T.);
#16513=EDGE_CURVE('',#12987,#12982,#7655,.T.);
#16514=EDGE_CURVE('',#12985,#12988,#7656,.T.);
#16515=EDGE_CURVE('',#12988,#12987,#114,.T.);
#16516=EDGE_CURVE('',#12986,#12989,#7657,.T.);
#16517=EDGE_CURVE('',#12989,#12974,#10942,.T.);
#16518=EDGE_CURVE('',#12990,#12959,#10943,.T.);
#16519=EDGE_CURVE('',#12959,#12974,#10944,.T.);
#16520=EDGE_CURVE('',#12989,#12990,#10945,.T.);
#16521=EDGE_CURVE('',#12990,#12980,#7658,.T.);
#16522=EDGE_CURVE('',#12991,#12987,#7659,.T.);
#16523=EDGE_CURVE('',#12988,#12992,#7660,.T.);
#16524=EDGE_CURVE('',#12992,#12991,#115,.T.);
#16525=EDGE_CURVE('',#12992,#12978,#7661,.T.);
#16526=EDGE_CURVE('',#12979,#12991,#7662,.T.);
#16527=EDGE_CURVE('',#12978,#12993,#7663,.T.);
#16528=EDGE_CURVE('',#12993,#12953,#116,.T.);
#16529=EDGE_CURVE('',#12993,#12994,#7664,.T.);
#16530=EDGE_CURVE('',#12994,#12964,#7665,.T.);
#16531=EDGE_CURVE('',#12995,#12976,#7666,.T.);
#16532=EDGE_CURVE('',#12996,#12995,#10946,.T.);
#16533=EDGE_CURVE('',#12997,#12996,#7667,.T.);
#16534=EDGE_CURVE('',#12998,#12997,#10947,.T.);
#16535=EDGE_CURVE('',#12999,#12998,#7668,.T.);
#16536=EDGE_CURVE('',#13000,#12999,#10948,.T.);
#16537=EDGE_CURVE('',#13001,#13000,#7669,.T.);
#16538=EDGE_CURVE('',#12994,#13001,#10949,.T.);
#16539=EDGE_CURVE('',#13002,#13002,#10950,.T.);
#16540=EDGE_CURVE('',#13003,#13003,#10951,.T.);
#16541=EDGE_CURVE('',#13004,#13004,#10952,.T.);
#16542=EDGE_CURVE('',#13005,#13005,#10953,.T.);
#16543=EDGE_CURVE('',#13006,#12986,#7670,.T.);
#16544=EDGE_CURVE('',#13007,#13006,#7671,.T.);
#16545=EDGE_CURVE('',#13008,#13007,#7672,.T.);
#16546=EDGE_CURVE('',#13009,#13008,#7673,.T.);
#16547=EDGE_CURVE('',#12980,#13009,#7674,.T.);
#16548=EDGE_CURVE('',#13010,#13010,#10954,.T.);
#16549=EDGE_CURVE('',#12983,#13006,#7675,.T.);
#16550=EDGE_CURVE('',#12982,#13007,#7676,.T.);
#16551=EDGE_CURVE('',#13011,#13011,#10955,.T.);
#16552=EDGE_CURVE('',#13011,#13012,#10956,.T.);
#16553=EDGE_CURVE('',#13012,#13012,#10957,.T.);
#16554=EDGE_CURVE('',#13013,#13013,#10958,.T.);
#16555=EDGE_CURVE('',#13013,#13011,#7677,.T.);
#16556=EDGE_CURVE('',#13014,#13014,#10959,.T.);
#16557=EDGE_CURVE('',#13002,#13013,#10960,.T.);
#16558=EDGE_CURVE('',#13015,#13015,#10961,.T.);
#16559=EDGE_CURVE('',#13015,#13016,#10962,.T.);
#16560=EDGE_CURVE('',#13016,#13016,#10963,.T.);
#16561=EDGE_CURVE('',#13017,#13017,#10964,.T.);
#16562=EDGE_CURVE('',#13017,#13015,#7678,.T.);
#16563=EDGE_CURVE('',#13018,#13018,#10965,.T.);
#16564=EDGE_CURVE('',#13005,#13017,#10966,.T.);
#16565=EDGE_CURVE('',#13003,#13019,#10967,.T.);
#16566=EDGE_CURVE('',#13019,#13019,#10968,.T.);
#16567=EDGE_CURVE('',#13019,#13020,#7679,.T.);
#16568=EDGE_CURVE('',#13020,#13020,#10969,.T.);
#16569=EDGE_CURVE('',#13004,#13021,#10970,.T.);
#16570=EDGE_CURVE('',#13021,#13021,#10971,.T.);
#16571=EDGE_CURVE('',#13021,#13022,#7680,.T.);
#16572=EDGE_CURVE('',#13022,#13022,#10972,.T.);
#16573=EDGE_CURVE('',#13023,#13024,#10973,.F.);
#16574=EDGE_CURVE('',#13025,#13023,#10974,.F.);
#16575=EDGE_CURVE('',#13024,#13025,#10975,.F.);
#16576=EDGE_CURVE('',#13026,#13027,#10976,.F.);
#16577=EDGE_CURVE('',#13028,#13026,#10977,.F.);
#16578=EDGE_CURVE('',#13027,#13028,#10978,.F.);
#16579=EDGE_CURVE('',#13023,#13028,#7681,.T.);
#16580=EDGE_CURVE('',#13026,#13025,#7682,.T.);
#16581=EDGE_CURVE('',#13029,#13030,#1402,.F.);
#16582=EDGE_CURVE('',#13030,#13027,#7683,.T.);
#16583=EDGE_CURVE('',#13028,#13029,#7684,.T.);
#16584=EDGE_CURVE('',#13031,#13032,#1403,.T.);
#16585=EDGE_CURVE('',#13032,#13026,#10979,.T.);
#16586=EDGE_CURVE('',#13027,#13031,#10980,.T.);
#16587=EDGE_CURVE('',#13033,#13034,#1404,.T.);
#16588=EDGE_CURVE('',#13034,#13024,#10981,.T.);
#16589=EDGE_CURVE('',#13025,#13033,#10982,.T.);
#16590=EDGE_CURVE('',#13035,#13036,#1405,.F.);
#16591=EDGE_CURVE('',#13036,#13023,#7685,.T.);
#16592=EDGE_CURVE('',#13024,#13035,#7686,.T.);
#16593=EDGE_CURVE('',#13037,#13030,#10983,.T.);
#16594=EDGE_CURVE('',#13038,#13037,#7687,.T.);
#16595=EDGE_CURVE('',#13038,#13039,#10984,.T.);
#16596=EDGE_CURVE('',#13039,#13031,#7688,.T.);
#16597=EDGE_CURVE('',#13029,#13040,#7689,.T.);
#16598=EDGE_CURVE('',#13041,#13036,#7690,.T.);
#16599=EDGE_CURVE('',#13041,#13042,#7691,.T.);
#16600=EDGE_CURVE('',#13043,#13042,#7692,.T.);
#16601=EDGE_CURVE('',#13043,#13040,#7693,.T.);
#16602=EDGE_CURVE('',#13044,#13045,#1406,.T.);
#16603=EDGE_CURVE('',#13045,#13046,#7694,.T.);
#16604=EDGE_CURVE('',#13046,#13047,#10985,.T.);
#16605=EDGE_CURVE('',#13047,#13044,#7695,.T.);
#16606=EDGE_CURVE('',#13048,#13049,#1407,.F.);
#16607=EDGE_CURVE('',#13049,#13050,#7696,.F.);
#16608=EDGE_CURVE('',#13051,#13050,#10986,.T.);
#16609=EDGE_CURVE('',#13051,#13052,#7697,.T.);
#16610=EDGE_CURVE('',#13052,#13046,#10987,.T.);
#16611=EDGE_CURVE('',#13046,#13048,#7698,.T.);
#16612=EDGE_CURVE('',#13052,#13047,#10988,.T.);
#16613=EDGE_CURVE('',#13053,#13044,#10989,.T.);
#16614=EDGE_CURVE('',#13054,#13053,#7699,.T.);
#16615=EDGE_CURVE('',#13055,#13054,#10990,.T.);
#16616=EDGE_CURVE('',#13056,#13055,#1408,.T.);
#16617=EDGE_CURVE('',#13057,#13056,#7700,.T.);
#16618=EDGE_CURVE('',#13058,#13057,#10991,.T.);
#16619=EDGE_CURVE('',#13059,#13058,#7701,.T.);
#16620=EDGE_CURVE('',#13060,#13059,#1409,.T.);
#16621=EDGE_CURVE('',#13061,#13060,#10992,.T.);
#16622=EDGE_CURVE('',#13061,#13045,#7702,.T.);
#16623=EDGE_CURVE('',#13062,#13047,#10993,.T.);
#16624=EDGE_CURVE('',#13063,#13062,#7703,.T.);
#16625=EDGE_CURVE('',#13063,#13064,#7704,.T.);
#16626=EDGE_CURVE('',#13064,#13053,#7705,.T.);
#16627=EDGE_CURVE('',#13052,#13065,#10994,.T.);
#16628=EDGE_CURVE('',#13065,#13062,#10995,.T.);
#16629=EDGE_CURVE('',#13066,#13051,#10996,.T.);
#16630=EDGE_CURVE('',#13067,#13066,#7706,.T.);
#16631=EDGE_CURVE('',#13068,#13067,#10997,.T.);
#16632=EDGE_CURVE('',#13069,#13068,#7707,.T.);
#16633=EDGE_CURVE('',#13070,#13069,#10998,.T.);
#16634=EDGE_CURVE('',#13065,#13070,#7708,.T.);
#16635=EDGE_CURVE('',#13071,#13072,#10999,.T.);
#16636=EDGE_CURVE('',#13073,#13071,#7709,.T.);
#16637=EDGE_CURVE('',#13073,#13074,#11000,.T.);
#16638=EDGE_CURVE('',#13072,#13074,#7710,.T.);
#16639=EDGE_CURVE('',#13075,#13076,#1410,.T.);
#16640=EDGE_CURVE('',#13075,#13077,#7711,.T.);
#16641=EDGE_CURVE('',#13077,#13069,#11001,.T.);
#16642=EDGE_CURVE('',#13068,#13078,#11002,.F.);
#16643=EDGE_CURVE('',#13076,#13078,#7712,.T.);
#16644=EDGE_CURVE('',#13079,#13080,#1411,.T.);
#16645=EDGE_CURVE('',#13080,#13081,#7713,.T.);
#16646=EDGE_CURVE('',#13081,#13077,#11003,.T.);
#16647=EDGE_CURVE('',#13077,#13079,#7714,.T.);
#16648=EDGE_CURVE('',#13081,#13069,#11004,.T.);
#16649=EDGE_CURVE('',#13081,#13082,#11005,.T.);
#16650=EDGE_CURVE('',#13070,#13082,#11006,.T.);
#16651=EDGE_CURVE('',#13080,#13083,#11007,.T.);
#16652=EDGE_CURVE('',#13083,#13084,#7715,.T.);
#16653=EDGE_CURVE('',#13084,#13085,#7716,.T.);
#16654=EDGE_CURVE('',#13082,#13085,#7717,.T.);
#16655=EDGE_CURVE('',#13079,#13086,#7718,.T.);
#16656=EDGE_CURVE('',#13087,#13086,#11008,.T.);
#16657=EDGE_CURVE('',#13088,#13087,#1412,.T.);
#16658=EDGE_CURVE('',#13089,#13088,#7719,.T.);
#16659=EDGE_CURVE('',#13090,#13089,#11009,.T.);
#16660=EDGE_CURVE('',#13091,#13090,#7720,.T.);
#16661=EDGE_CURVE('',#13092,#13091,#1413,.T.);
#16662=EDGE_CURVE('',#13093,#13092,#11010,.T.);
#16663=EDGE_CURVE('',#13083,#13093,#7721,.T.);
#16664=EDGE_CURVE('',#13074,#13094,#1414,.F.);
#16665=EDGE_CURVE('',#13094,#13095,#7722,.T.);
#16666=EDGE_CURVE('',#13095,#13072,#1415,.F.);
#16667=EDGE_CURVE('',#13096,#13094,#1416,.F.);
#16668=EDGE_CURVE('',#13097,#13096,#7723,.T.);
#16669=EDGE_CURVE('',#13098,#13097,#7724,.T.);
#16670=EDGE_CURVE('',#13098,#13099,#7725,.T.);
#16671=EDGE_CURVE('',#13095,#13099,#1417,.F.);
#16672=EDGE_CURVE('',#13100,#13100,#11011,.T.);
#16673=EDGE_CURVE('',#13100,#13101,#11012,.T.);
#16674=EDGE_CURVE('',#13101,#13102,#11013,.T.);
#16675=EDGE_CURVE('',#13102,#13101,#11014,.T.);
#16676=EDGE_CURVE('',#13103,#13104,#11015,.T.);
#16677=EDGE_CURVE('',#13105,#13103,#7726,.T.);
#16678=EDGE_CURVE('',#13106,#13105,#7727,.T.);
#16679=EDGE_CURVE('',#13107,#13106,#7728,.T.);
#16680=EDGE_CURVE('',#13067,#13107,#7729,.T.);
#16681=EDGE_CURVE('',#13108,#13066,#7730,.T.);
#16682=EDGE_CURVE('',#13109,#13108,#7731,.T.);
#16683=EDGE_CURVE('',#13110,#13109,#7732,.T.);
#16684=EDGE_CURVE('',#13111,#13110,#7733,.T.);
#16685=EDGE_CURVE('',#13104,#13111,#11016,.T.);
#16686=EDGE_CURVE('',#13112,#13112,#11017,.T.);
#16687=EDGE_CURVE('',#13113,#13113,#11018,.T.);
#16688=EDGE_CURVE('',#13114,#13114,#11019,.T.);
#16689=EDGE_CURVE('',#13114,#13102,#7734,.T.);
#16690=EDGE_CURVE('',#13112,#13115,#11020,.T.);
#16691=EDGE_CURVE('',#13115,#13116,#11021,.T.);
#16692=EDGE_CURVE('',#13116,#13115,#11022,.T.);
#16693=EDGE_CURVE('',#13117,#13117,#11023,.T.);
#16694=EDGE_CURVE('',#13117,#13116,#7735,.T.);
#16695=EDGE_CURVE('',#13113,#13118,#11024,.T.);
#16696=EDGE_CURVE('',#13118,#13119,#11025,.T.);
#16697=EDGE_CURVE('',#13119,#13118,#11026,.T.);
#16698=EDGE_CURVE('',#13120,#13120,#11027,.T.);
#16699=EDGE_CURVE('',#13120,#13119,#7736,.T.);
#16700=EDGE_CURVE('',#13111,#13103,#1418,.T.);
#16701=EDGE_CURVE('',#13104,#13121,#11028,.T.);
#16702=EDGE_CURVE('',#13121,#13122,#11029,.T.);
#16703=EDGE_CURVE('',#13122,#13121,#11030,.T.);
#16704=EDGE_CURVE('',#13123,#13110,#1419,.T.);
#16705=EDGE_CURVE('',#13124,#13123,#7737,.T.);
#16706=EDGE_CURVE('',#13125,#13124,#117,.T.);
#16707=EDGE_CURVE('',#13126,#13125,#7738,.T.);
#16708=EDGE_CURVE('',#13127,#13126,#118,.T.);
#16709=EDGE_CURVE('',#13128,#13127,#7739,.T.);
#16710=EDGE_CURVE('',#13105,#13128,#1420,.T.);
#16711=EDGE_CURVE('',#13129,#13129,#11031,.T.);
#16712=EDGE_CURVE('',#13129,#13122,#7740,.T.);
#16713=EDGE_CURVE('',#13073,#13130,#1421,.T.);
#16714=EDGE_CURVE('',#13071,#13131,#1422,.F.);
#16715=EDGE_CURVE('',#13131,#13132,#11032,.F.);
#16716=EDGE_CURVE('',#13132,#13133,#7741,.T.);
#16717=EDGE_CURVE('',#13130,#13133,#11033,.T.);
#16718=EDGE_CURVE('',#13134,#13132,#7742,.T.);
#16719=EDGE_CURVE('',#13134,#13135,#7743,.T.);
#16720=EDGE_CURVE('',#13136,#13135,#7744,.F.);
#16721=EDGE_CURVE('',#13137,#13136,#7745,.T.);
#16722=EDGE_CURVE('',#12949,#13137,#7746,.T.);
#16723=EDGE_CURVE('',#12948,#13138,#7747,.T.);
#16724=EDGE_CURVE('',#13138,#13139,#7748,.T.);
#16725=EDGE_CURVE('',#13139,#13133,#7749,.T.);
#16726=EDGE_CURVE('',#13140,#13140,#11034,.T.);
#16727=EDGE_CURVE('',#13141,#13141,#11035,.T.);
#16728=EDGE_CURVE('',#13142,#13142,#11036,.T.);
#16729=EDGE_CURVE('',#13143,#13143,#11037,.T.);
#16730=EDGE_CURVE('',#13010,#13144,#11038,.T.);
#16731=EDGE_CURVE('',#13144,#13144,#11039,.T.);
#16732=EDGE_CURVE('',#13144,#13145,#7750,.T.);
#16733=EDGE_CURVE('',#13146,#13145,#11040,.T.);
#16734=EDGE_CURVE('',#13145,#13146,#11041,.T.);
#16735=EDGE_CURVE('',#13147,#13148,#1423,.T.);
#16736=EDGE_CURVE('',#13148,#13149,#11042,.T.);
#16737=EDGE_CURVE('',#13149,#13150,#1424,.T.);
#16738=EDGE_CURVE('',#13150,#13147,#11043,.T.);
#16739=EDGE_CURVE('',#13151,#13150,#7751,.T.);
#16740=EDGE_CURVE('',#13152,#13151,#11044,.T.);
#16741=EDGE_CURVE('',#13147,#13152,#7752,.T.);
#16742=EDGE_CURVE('',#13153,#13149,#7753,.T.);
#16743=EDGE_CURVE('',#13154,#13153,#7754,.T.);
#16744=EDGE_CURVE('',#13150,#13154,#7755,.T.);
#16745=EDGE_CURVE('',#13151,#13155,#1425,.T.);
#16746=EDGE_CURVE('',#13155,#13156,#11045,.T.);
#16747=EDGE_CURVE('',#13156,#13152,#1426,.T.);
#16748=EDGE_CURVE('',#13155,#13157,#7756,.T.);
#16749=EDGE_CURVE('',#13157,#13158,#11046,.T.);
#16750=EDGE_CURVE('',#13158,#13156,#7757,.T.);
#16751=EDGE_CURVE('',#13159,#13151,#7758,.T.);
#16752=EDGE_CURVE('',#13157,#13159,#7759,.T.);
#16753=EDGE_CURVE('',#13160,#13160,#11047,.T.);
#16754=EDGE_CURVE('',#13160,#13146,#11048,.T.);
#16755=EDGE_CURVE('',#12975,#12958,#11049,.T.);
#16756=EDGE_CURVE('',#13161,#12963,#11050,.T.);
#16757=EDGE_CURVE('',#13162,#13161,#7760,.T.);
#16758=EDGE_CURVE('',#13163,#13162,#11051,.T.);
#16759=EDGE_CURVE('',#13164,#13163,#7761,.T.);
#16760=EDGE_CURVE('',#13165,#13164,#11052,.T.);
#16761=EDGE_CURVE('',#13166,#13165,#7762,.T.);
#16762=EDGE_CURVE('',#12970,#13166,#11053,.T.);
#16763=EDGE_CURVE('',#13167,#13167,#11054,.T.);
#16764=EDGE_CURVE('',#13168,#13168,#11055,.T.);
#16765=EDGE_CURVE('',#13169,#13169,#11056,.T.);
#16766=EDGE_CURVE('',#13170,#13170,#11057,.T.);
#16767=EDGE_CURVE('',#13171,#13172,#7763,.T.);
#16768=EDGE_CURVE('',#13173,#13171,#7764,.T.);
#16769=EDGE_CURVE('',#13173,#13174,#7765,.T.);
#16770=EDGE_CURVE('',#13174,#13042,#7766,.T.);
#16771=EDGE_CURVE('',#13043,#13042,#7767,.T.);
#16772=EDGE_CURVE('',#13043,#13175,#7768,.T.);
#16773=EDGE_CURVE('',#13175,#13176,#7769,.T.);
#16774=EDGE_CURVE('',#13177,#13176,#7770,.T.);
#16775=EDGE_CURVE('',#13178,#13177,#7771,.T.);
#16776=EDGE_CURVE('',#13178,#13043,#7772,.T.);
#16777=EDGE_CURVE('',#13042,#13172,#7773,.T.);
#16778=EDGE_CURVE('',#13179,#13137,#11058,.T.);
#16779=EDGE_CURVE('',#13126,#13179,#119,.T.);
#16780=EDGE_CURVE('',#13125,#12950,#120,.F.);
#16781=EDGE_CURVE('',#13140,#13129,#11059,.T.);
#16782=EDGE_CURVE('',#13143,#13120,#11060,.T.);
#16783=EDGE_CURVE('',#13141,#13117,#11061,.T.);
#16784=EDGE_CURVE('',#13142,#13114,#11062,.T.);
#16785=EDGE_CURVE('',#13180,#13181,#121,.T.);
#16786=EDGE_CURVE('',#13181,#13182,#7774,.T.);
#16787=EDGE_CURVE('',#13182,#13183,#122,.T.);
#16788=EDGE_CURVE('',#13183,#13184,#7775,.T.);
#16789=EDGE_CURVE('',#13184,#13185,#1427,.T.);
#16790=EDGE_CURVE('',#13185,#13186,#7776,.T.);
#16791=EDGE_CURVE('',#13186,#13187,#1428,.T.);
#16792=EDGE_CURVE('',#13187,#13180,#7777,.T.);
#16793=EDGE_CURVE('',#13180,#13063,#11063,.T.);
#16794=EDGE_CURVE('',#13065,#13181,#7778,.T.);
#16795=EDGE_CURVE('',#13187,#13188,#7779,.T.);
#16796=EDGE_CURVE('',#13189,#13188,#7780,.T.);
#16797=EDGE_CURVE('',#13189,#13064,#7781,.T.);
#16798=EDGE_CURVE('',#13186,#13190,#253,.T.);
#16799=EDGE_CURVE('',#13190,#13188,#11064,.T.);
#16800=EDGE_CURVE('',#13191,#13185,#254,.T.);
#16801=EDGE_CURVE('',#13192,#13191,#7782,.T.);
#16802=EDGE_CURVE('',#13193,#13192,#7783,.T.);
#16803=EDGE_CURVE('',#13193,#13043,#7784,.T.);
#16804=EDGE_CURVE('',#13042,#13194,#7785,.T.);
#16805=EDGE_CURVE('',#13195,#13194,#7786,.T.);
#16806=EDGE_CURVE('',#13190,#13195,#7787,.T.);
#16807=EDGE_CURVE('',#13182,#13070,#7788,.T.);
#16808=EDGE_CURVE('',#13099,#13131,#11065,.T.);
#16809=EDGE_CURVE('',#13196,#13098,#7789,.T.);
#16810=EDGE_CURVE('',#13134,#13196,#11066,.T.);
#16811=EDGE_CURVE('',#13130,#13096,#11067,.T.);
#16812=EDGE_CURVE('',#13197,#13139,#11068,.T.);
#16813=EDGE_CURVE('',#13097,#13197,#7790,.T.);
#16814=EDGE_CURVE('',#13085,#13183,#11069,.T.);
#16815=EDGE_CURVE('',#13084,#13198,#7791,.T.);
#16816=EDGE_CURVE('',#13199,#13198,#7792,.T.);
#16817=EDGE_CURVE('',#13184,#13199,#7793,.T.);
#16818=EDGE_CURVE('',#13198,#13093,#7794,.T.);
#16819=EDGE_CURVE('',#13200,#13075,#255,.T.);
#16820=EDGE_CURVE('',#13086,#13200,#7795,.T.);
#16821=EDGE_CURVE('',#13201,#13076,#1429,.F.);
#16822=EDGE_CURVE('',#13201,#13106,#1430,.T.);
#16823=EDGE_CURVE('',#13106,#13202,#7796,.T.);
#16824=EDGE_CURVE('',#13202,#13200,#11070,.T.);
#16825=EDGE_CURVE('',#13087,#13203,#11071,.T.);
#16826=EDGE_CURVE('',#13204,#13203,#7797,.T.);
#16827=EDGE_CURVE('',#13204,#13088,#1431,.T.);
#16828=EDGE_CURVE('',#13205,#13202,#7798,.T.);
#16829=EDGE_CURVE('',#13206,#13205,#11072,.T.);
#16830=EDGE_CURVE('',#13207,#13206,#7799,.T.);
#16831=EDGE_CURVE('',#13208,#13207,#11073,.T.);
#16832=EDGE_CURVE('',#13209,#13208,#7800,.T.);
#16833=EDGE_CURVE('',#13210,#13209,#11074,.T.);
#16834=EDGE_CURVE('',#13192,#13210,#7801,.T.);
#16835=EDGE_CURVE('',#13199,#13191,#11075,.T.);
#16836=EDGE_CURVE('',#13211,#13092,#11076,.T.);
#16837=EDGE_CURVE('',#13212,#13211,#7802,.T.);
#16838=EDGE_CURVE('',#13213,#13212,#11077,.T.);
#16839=EDGE_CURVE('',#13203,#13213,#7803,.T.);
#16840=EDGE_CURVE('',#13214,#13215,#1432,.T.);
#16841=EDGE_CURVE('',#13215,#13216,#1433,.T.);
#16842=EDGE_CURVE('',#13216,#13217,#1434,.T.);
#16843=EDGE_CURVE('',#13217,#13218,#1435,.T.);
#16844=EDGE_CURVE('',#13218,#13219,#1436,.T.);
#16845=EDGE_CURVE('',#13219,#13220,#1437,.T.);
#16846=EDGE_CURVE('',#13220,#13221,#1438,.T.);
#16847=EDGE_CURVE('',#13221,#13222,#1439,.T.);
#16848=EDGE_CURVE('',#13222,#13223,#1440,.T.);
#16849=EDGE_CURVE('',#13223,#13214,#1441,.T.);
#16850=EDGE_CURVE('',#13224,#13225,#7804,.T.);
#16851=EDGE_CURVE('',#13225,#13226,#7805,.T.);
#16852=EDGE_CURVE('',#13226,#13227,#7806,.T.);
#16853=EDGE_CURVE('',#13227,#13224,#7807,.T.);
#16854=EDGE_CURVE('',#13228,#13228,#11078,.T.);
#16855=EDGE_CURVE('',#13229,#13230,#7808,.T.);
#16856=EDGE_CURVE('',#13230,#13231,#7809,.T.);
#16857=EDGE_CURVE('',#13231,#13232,#7810,.T.);
#16858=EDGE_CURVE('',#13232,#13233,#7811,.T.);
#16859=EDGE_CURVE('',#13233,#13234,#7812,.T.);
#16860=EDGE_CURVE('',#13234,#13235,#7813,.T.);
#16861=EDGE_CURVE('',#13235,#13236,#7814,.T.);
#16862=EDGE_CURVE('',#13236,#13237,#7815,.T.);
#16863=EDGE_CURVE('',#13237,#13238,#7816,.T.);
#16864=EDGE_CURVE('',#13238,#13229,#7817,.T.);
#16865=EDGE_CURVE('',#13239,#13240,#7818,.T.);
#16866=EDGE_CURVE('',#13240,#13241,#7819,.T.);
#16867=EDGE_CURVE('',#13241,#13242,#7820,.T.);
#16868=EDGE_CURVE('',#13242,#13243,#1442,.T.);
#16869=EDGE_CURVE('',#13243,#13244,#1443,.T.);
#16870=EDGE_CURVE('',#13244,#13245,#7821,.T.);
#16871=EDGE_CURVE('',#13245,#13246,#1444,.T.);
#16872=EDGE_CURVE('',#13246,#13247,#1445,.T.);
#16873=EDGE_CURVE('',#13247,#13239,#7822,.T.);
#16874=EDGE_CURVE('',#13078,#13107,#11079,.T.);
#16875=EDGE_CURVE('',#13248,#13061,#7823,.T.);
#16876=EDGE_CURVE('',#13048,#13248,#256,.T.);
#16877=EDGE_CURVE('',#13054,#13189,#7824,.T.);
#16878=EDGE_CURVE('',#13249,#13056,#11080,.T.);
#16879=EDGE_CURVE('',#13249,#13250,#7825,.T.);
#16880=EDGE_CURVE('',#13057,#13250,#11081,.T.);
#16881=EDGE_CURVE('',#13055,#13251,#11082,.T.);
#16882=EDGE_CURVE('',#13249,#13251,#7826,.T.);
#16883=EDGE_CURVE('',#13252,#13195,#7827,.T.);
#16884=EDGE_CURVE('',#13253,#13252,#11083,.T.);
#16885=EDGE_CURVE('',#13254,#13253,#7828,.T.);
#16886=EDGE_CURVE('',#13255,#13254,#11084,.T.);
#16887=EDGE_CURVE('',#13256,#13255,#7829,.T.);
#16888=EDGE_CURVE('',#13257,#13256,#11085,.T.);
#16889=EDGE_CURVE('',#13258,#13257,#7830,.T.);
#16890=EDGE_CURVE('',#13248,#13258,#11086,.T.);
#16891=EDGE_CURVE('',#13259,#13060,#11087,.T.);
#16892=EDGE_CURVE('',#13260,#13259,#7831,.T.);
#16893=EDGE_CURVE('',#13261,#13260,#11088,.T.);
#16894=EDGE_CURVE('',#13251,#13261,#7832,.T.);
#16895=EDGE_CURVE('',#13262,#13262,#11089,.T.);
#16896=EDGE_CURVE('',#13109,#13258,#7833,.T.);
#16897=EDGE_CURVE('',#13109,#13263,#1446,.T.);
#16898=EDGE_CURVE('',#13263,#13049,#1447,.T.);
#16899=EDGE_CURVE('',#13050,#13108,#11090,.T.);
#16900=EDGE_CURVE('',#13264,#13196,#7834,.T.);
#16901=EDGE_CURVE('',#13135,#13264,#123,.T.);
#16902=EDGE_CURVE('',#13265,#13138,#124,.T.);
#16903=EDGE_CURVE('',#13197,#13265,#7835,.T.);
#16904=EDGE_CURVE('',#13266,#13193,#7836,.T.);
#16905=EDGE_CURVE('',#13267,#13266,#11091,.T.);
#16906=EDGE_CURVE('',#13268,#13267,#7837,.T.);
#16907=EDGE_CURVE('',#13175,#13268,#11092,.T.);
#16908=EDGE_CURVE('',#13194,#13269,#7838,.T.);
#16909=EDGE_CURVE('',#13270,#13174,#11093,.T.);
#16910=EDGE_CURVE('',#13271,#13270,#7839,.T.);
#16911=EDGE_CURVE('',#13269,#13271,#11094,.T.);
#16912=EDGE_CURVE('',#13172,#13041,#11095,.T.);
#16913=EDGE_CURVE('',#13040,#13178,#11096,.T.);
#16914=EDGE_CURVE('',#13037,#13177,#125,.T.);
#16915=EDGE_CURVE('',#13035,#13272,#11097,.T.);
#16916=EDGE_CURVE('',#13171,#13272,#126,.T.);
#16917=EDGE_CURVE('',#13124,#13273,#7840,.T.);
#16918=EDGE_CURVE('',#13273,#12945,#7841,.T.);
#16919=EDGE_CURVE('',#13110,#13257,#7842,.T.);
#16920=EDGE_CURVE('',#13123,#13256,#7843,.T.);
#16921=EDGE_CURVE('',#13274,#13266,#127,.T.);
#16922=EDGE_CURVE('',#13267,#13274,#257,.T.);
#16923=EDGE_CURVE('',#13269,#13275,#128,.T.);
#16924=EDGE_CURVE('',#13275,#13276,#7844,.T.);
#16925=EDGE_CURVE('',#13276,#13252,#129,.T.);
#16926=EDGE_CURVE('',#13270,#13173,#130,.T.);
#16927=EDGE_CURVE('',#13275,#13271,#258,.T.);
#16928=EDGE_CURVE('',#13277,#13158,#7845,.T.);
#16929=EDGE_CURVE('',#13152,#13277,#7846,.T.);
#16930=EDGE_CURVE('',#13278,#13147,#7847,.T.);
#16931=EDGE_CURVE('',#13279,#13278,#7848,.T.);
#16932=EDGE_CURVE('',#13148,#13279,#7849,.T.);
#16933=EDGE_CURVE('',#13277,#13159,#1448,.T.);
#16934=EDGE_CURVE('',#13154,#13278,#1449,.T.);
#16935=EDGE_CURVE('',#13279,#13153,#11098,.T.);
#16936=EDGE_CURVE('',#13128,#13152,#7850,.T.);
#16937=EDGE_CURVE('',#13280,#13127,#7851,.T.);
#16938=EDGE_CURVE('',#13273,#13280,#7852,.T.);
#16939=EDGE_CURVE('',#13147,#13123,#7853,.T.);
#16940=EDGE_CURVE('',#13159,#13208,#7854,.T.);
#16941=EDGE_CURVE('',#13277,#13207,#7855,.T.);
#16942=EDGE_CURVE('',#13281,#13090,#11099,.T.);
#16943=EDGE_CURVE('',#13281,#13282,#7856,.T.);
#16944=EDGE_CURVE('',#13091,#13282,#11100,.T.);
#16945=EDGE_CURVE('',#13282,#13283,#7857,.T.);
#16946=EDGE_CURVE('',#13284,#13281,#7858,.T.);
#16947=EDGE_CURVE('',#13283,#13284,#7859,.T.);
#16948=EDGE_CURVE('',#13285,#13249,#7860,.T.);
#16949=EDGE_CURVE('',#13286,#13285,#7861,.T.);
#16950=EDGE_CURVE('',#13250,#13286,#7862,.T.);
#16951=EDGE_CURVE('',#13287,#13265,#7863,.T.);
#16952=EDGE_CURVE('',#13288,#13287,#7864,.T.);
#16953=EDGE_CURVE('',#13264,#13288,#7865,.T.);
#16954=EDGE_CURVE('',#13289,#13204,#7866,.T.);
#16955=EDGE_CURVE('',#13290,#13289,#7867,.T.);
#16956=EDGE_CURVE('',#13291,#13290,#7868,.T.);
#16957=EDGE_CURVE('',#13291,#13204,#7869,.T.);
#16958=EDGE_CURVE('',#13292,#13293,#7870,.T.);
#16959=EDGE_CURVE('',#13292,#13294,#7871,.T.);
#16960=EDGE_CURVE('',#13295,#13294,#7872,.T.);
#16961=EDGE_CURVE('',#13293,#13295,#7873,.T.);
#16962=EDGE_CURVE('',#13089,#13291,#11101,.T.);
#16963=EDGE_CURVE('',#13290,#13284,#11102,.T.);
#16964=EDGE_CURVE('',#13294,#13058,#11103,.T.);
#16965=EDGE_CURVE('',#13059,#13292,#1450,.T.);
#16966=EDGE_CURVE('',#13289,#13293,#7874,.T.);
#16967=EDGE_CURVE('',#13286,#13295,#11104,.T.);
#16968=EDGE_CURVE('',#13285,#13283,#7875,.T.);
#16969=EDGE_CURVE('',#13292,#13259,#7876,.T.);
#16970=EDGE_CURVE('',#12947,#13287,#7877,.T.);
#16971=EDGE_CURVE('',#13039,#13296,#7878,.T.);
#16972=EDGE_CURVE('',#13032,#13296,#7879,.T.);
#16973=EDGE_CURVE('',#13297,#13033,#7880,.T.);
#16974=EDGE_CURVE('',#13297,#13298,#7881,.T.);
#16975=EDGE_CURVE('',#13034,#13298,#7882,.T.);
#16976=EDGE_CURVE('',#13299,#13038,#131,.T.);
#16977=EDGE_CURVE('',#13296,#13299,#1451,.T.);
#16978=EDGE_CURVE('',#13300,#13301,#132,.T.);
#16979=EDGE_CURVE('',#13298,#13300,#11105,.T.);
#16980=EDGE_CURVE('',#13301,#13297,#1452,.T.);
#16981=EDGE_CURVE('',#13033,#13032,#7883,.T.);
#16982=EDGE_CURVE('',#13272,#13300,#7884,.T.);
#16983=EDGE_CURVE('',#13302,#13301,#259,.F.);
#16984=EDGE_CURVE('',#13302,#13276,#260,.T.);
#16985=EDGE_CURVE('',#13297,#13253,#7885,.T.);
#16986=EDGE_CURVE('',#13033,#13150,#7886,.T.);
#16987=EDGE_CURVE('',#13151,#13032,#7887,.T.);
#16988=EDGE_CURVE('',#13239,#13303,#7888,.T.);
#16989=EDGE_CURVE('',#13304,#13303,#7889,.T.);
#16990=EDGE_CURVE('',#13240,#13304,#7890,.T.);
#16991=EDGE_CURVE('',#13305,#13304,#7891,.T.);
#16992=EDGE_CURVE('',#13241,#13305,#7892,.T.);
#16993=EDGE_CURVE('',#13306,#13305,#7893,.T.);
#16994=EDGE_CURVE('',#13242,#13306,#7894,.T.);
#16995=EDGE_CURVE('',#13307,#13306,#1453,.T.);
#16996=EDGE_CURVE('',#13243,#13307,#7895,.T.);
#16997=EDGE_CURVE('',#13308,#13307,#1454,.T.);
#16998=EDGE_CURVE('',#13244,#13308,#7896,.T.);
#16999=EDGE_CURVE('',#13309,#13308,#7897,.T.);
#17000=EDGE_CURVE('',#13245,#13309,#7898,.T.);
#17001=EDGE_CURVE('',#13310,#13309,#1455,.T.);
#17002=EDGE_CURVE('',#13246,#13310,#7899,.T.);
#17003=EDGE_CURVE('',#13311,#13310,#1456,.T.);
#17004=EDGE_CURVE('',#13247,#13311,#7900,.T.);
#17005=EDGE_CURVE('',#13303,#13311,#7901,.T.);
#17006=EDGE_CURVE('',#13229,#13312,#7902,.T.);
#17007=EDGE_CURVE('',#13313,#13312,#7903,.T.);
#17008=EDGE_CURVE('',#13230,#13313,#7904,.T.);
#17009=EDGE_CURVE('',#13314,#13313,#7905,.T.);
#17010=EDGE_CURVE('',#13231,#13314,#7906,.T.);
#17011=EDGE_CURVE('',#13315,#13314,#7907,.T.);
#17012=EDGE_CURVE('',#13232,#13315,#7908,.T.);
#17013=EDGE_CURVE('',#13316,#13315,#7909,.T.);
#17014=EDGE_CURVE('',#13233,#13316,#7910,.T.);
#17015=EDGE_CURVE('',#13317,#13316,#7911,.T.);
#17016=EDGE_CURVE('',#13234,#13317,#7912,.T.);
#17017=EDGE_CURVE('',#13318,#13317,#7913,.T.);
#17018=EDGE_CURVE('',#13235,#13318,#7914,.T.);
#17019=EDGE_CURVE('',#13319,#13318,#7915,.T.);
#17020=EDGE_CURVE('',#13236,#13319,#7916,.T.);
#17021=EDGE_CURVE('',#13320,#13319,#7917,.T.);
#17022=EDGE_CURVE('',#13237,#13320,#7918,.T.);
#17023=EDGE_CURVE('',#13321,#13320,#7919,.T.);
#17024=EDGE_CURVE('',#13238,#13321,#7920,.T.);
#17025=EDGE_CURVE('',#13312,#13321,#7921,.T.);
#17026=EDGE_CURVE('',#13322,#13323,#1457,.T.);
#17027=EDGE_CURVE('',#13322,#13324,#7922,.T.);
#17028=EDGE_CURVE('',#13325,#13324,#1458,.T.);
#17029=EDGE_CURVE('',#13323,#13325,#7923,.T.);
#17030=EDGE_CURVE('',#13323,#13326,#1459,.T.);
#17031=EDGE_CURVE('',#13327,#13325,#1460,.T.);
#17032=EDGE_CURVE('',#13326,#13327,#7924,.T.);
#17033=EDGE_CURVE('',#13326,#13328,#1461,.T.);
#17034=EDGE_CURVE('',#13329,#13327,#1462,.T.);
#17035=EDGE_CURVE('',#13328,#13329,#7925,.T.);
#17036=EDGE_CURVE('',#13328,#13330,#1463,.T.);
#17037=EDGE_CURVE('',#13331,#13329,#1464,.T.);
#17038=EDGE_CURVE('',#13330,#13331,#7926,.T.);
#17039=EDGE_CURVE('',#13330,#13332,#1465,.T.);
#17040=EDGE_CURVE('',#13333,#13331,#1466,.T.);
#17041=EDGE_CURVE('',#13332,#13333,#7927,.T.);
#17042=EDGE_CURVE('',#13332,#13334,#1467,.T.);
#17043=EDGE_CURVE('',#13335,#13333,#1468,.T.);
#17044=EDGE_CURVE('',#13334,#13335,#7928,.T.);
#17045=EDGE_CURVE('',#13334,#13336,#1469,.T.);
#17046=EDGE_CURVE('',#13337,#13335,#1470,.T.);
#17047=EDGE_CURVE('',#13336,#13337,#7929,.T.);
#17048=EDGE_CURVE('',#13336,#13322,#1471,.T.);
#17049=EDGE_CURVE('',#13324,#13337,#1472,.T.);
#17050=EDGE_CURVE('',#13214,#13338,#7930,.T.);
#17051=EDGE_CURVE('',#13339,#13338,#1473,.T.);
#17052=EDGE_CURVE('',#13215,#13339,#7931,.T.);
#17053=EDGE_CURVE('',#13340,#13339,#1474,.T.);
#17054=EDGE_CURVE('',#13216,#13340,#7932,.T.);
#17055=EDGE_CURVE('',#13341,#13340,#1475,.T.);
#17056=EDGE_CURVE('',#13217,#13341,#7933,.T.);
#17057=EDGE_CURVE('',#13342,#13341,#1476,.T.);
#17058=EDGE_CURVE('',#13218,#13342,#7934,.T.);
#17059=EDGE_CURVE('',#13343,#13342,#1477,.T.);
#17060=EDGE_CURVE('',#13219,#13343,#7935,.T.);
#17061=EDGE_CURVE('',#13344,#13343,#1478,.T.);
#17062=EDGE_CURVE('',#13220,#13344,#7936,.T.);
#17063=EDGE_CURVE('',#13345,#13344,#1479,.T.);
#17064=EDGE_CURVE('',#13221,#13345,#7937,.T.);
#17065=EDGE_CURVE('',#13346,#13345,#1480,.T.);
#17066=EDGE_CURVE('',#13222,#13346,#7938,.T.);
#17067=EDGE_CURVE('',#13347,#13346,#1481,.T.);
#17068=EDGE_CURVE('',#13223,#13347,#7939,.T.);
#17069=EDGE_CURVE('',#13338,#13347,#1482,.T.);
#17070=EDGE_CURVE('',#13224,#13348,#7940,.T.);
#17071=EDGE_CURVE('',#13349,#13348,#7941,.T.);
#17072=EDGE_CURVE('',#13225,#13349,#7942,.T.);
#17073=EDGE_CURVE('',#13350,#13349,#7943,.T.);
#17074=EDGE_CURVE('',#13226,#13350,#7944,.T.);
#17075=EDGE_CURVE('',#13351,#13350,#7945,.T.);
#17076=EDGE_CURVE('',#13227,#13351,#7946,.T.);
#17077=EDGE_CURVE('',#13348,#13351,#7947,.T.);
#17078=EDGE_CURVE('',#13352,#13352,#11106,.T.);
#17079=EDGE_CURVE('',#13352,#13170,#7948,.T.);
#17080=EDGE_CURVE('',#13353,#13353,#11107,.T.);
#17081=EDGE_CURVE('',#13353,#13168,#7949,.T.);
#17082=EDGE_CURVE('',#13018,#13169,#7950,.T.);
#17083=EDGE_CURVE('',#13014,#13167,#7951,.T.);
#17084=EDGE_CURVE('',#12991,#13009,#7952,.T.);
#17085=EDGE_CURVE('',#12987,#13008,#7953,.T.);
#17086=EDGE_CURVE('',#12967,#13354,#7954,.T.);
#17087=EDGE_CURVE('',#12995,#13354,#7955,.T.);
#17088=EDGE_CURVE('',#13354,#12971,#7956,.T.);
#17089=EDGE_CURVE('',#13280,#12946,#7957,.T.);
#17090=EDGE_CURVE('',#13179,#12946,#7958,.F.);
#17091=EDGE_CURVE('',#13355,#13136,#7959,.T.);
#17092=EDGE_CURVE('',#12936,#13355,#7960,.T.);
#17093=EDGE_CURVE('',#12947,#13355,#7961,.T.);
#17094=EDGE_CURVE('',#13355,#13288,#7962,.T.);
#17095=EDGE_CURVE('',#13356,#13356,#11108,.T.);
#17096=EDGE_CURVE('',#13356,#12952,#7963,.T.);
#17097=EDGE_CURVE('',#13357,#13357,#11109,.T.);
#17098=EDGE_CURVE('',#13358,#13358,#11110,.T.);
#17099=EDGE_CURVE('',#13358,#12951,#7964,.T.);
#17100=EDGE_CURVE('',#13359,#13359,#11111,.T.);
#17101=EDGE_CURVE('',#13228,#13360,#7965,.T.);
#17102=EDGE_CURVE('',#13360,#13360,#11112,.T.);
#17103=EDGE_CURVE('',#13360,#13361,#7966,.T.);
#17104=EDGE_CURVE('',#13361,#13361,#11113,.T.);
#17105=EDGE_CURVE('',#13359,#13361,#7967,.T.);
#17106=EDGE_CURVE('',#13262,#13362,#7968,.T.);
#17107=EDGE_CURVE('',#13362,#13362,#11114,.T.);
#17108=EDGE_CURVE('',#13363,#13363,#11115,.T.);
#17109=EDGE_CURVE('',#13363,#13362,#7969,.T.);
#17110=EDGE_CURVE('',#13357,#13363,#7970,.T.);
#17111=EDGE_CURVE('',#13210,#13364,#133,.T.);
#17112=EDGE_CURVE('',#13364,#13274,#7971,.T.);
#17113=EDGE_CURVE('',#13282,#13211,#7972,.T.);
#17114=EDGE_CURVE('',#13283,#13212,#7973,.T.);
#17115=EDGE_CURVE('',#13289,#13213,#7974,.T.);
#17116=EDGE_CURVE('',#13283,#13289,#11116,.T.);
#17117=EDGE_CURVE('',#13105,#13205,#7975,.T.);
#17118=EDGE_CURVE('',#13128,#13206,#7976,.T.);
#17119=EDGE_CURVE('',#13296,#13209,#7977,.T.);
#17120=EDGE_CURVE('',#13299,#13365,#261,.F.);
#17121=EDGE_CURVE('',#13364,#13365,#262,.T.);
#17122=EDGE_CURVE('',#13293,#13285,#11117,.T.);
#17123=EDGE_CURVE('',#13176,#13268,#134,.T.);
#17124=EDGE_CURVE('',#13154,#13254,#7978,.T.);
#17125=EDGE_CURVE('',#13278,#13255,#7979,.T.);
#17126=EDGE_CURVE('',#13293,#13260,#7980,.T.);
#17127=EDGE_CURVE('',#13285,#13261,#7981,.T.);
#17128=EDGE_CURVE('',#12998,#13366,#7982,.T.);
#17129=EDGE_CURVE('',#13366,#13367,#7983,.T.);
#17130=EDGE_CURVE('',#13367,#12999,#7984,.T.);
#17131=EDGE_CURVE('',#12997,#13368,#7985,.T.);
#17132=EDGE_CURVE('',#13368,#13366,#11118,.T.);
#17133=EDGE_CURVE('',#12996,#13369,#7986,.T.);
#17134=EDGE_CURVE('',#13369,#13368,#7987,.T.);
#17135=EDGE_CURVE('',#13354,#13369,#11119,.T.);
#17136=EDGE_CURVE('',#13001,#13370,#7988,.T.);
#17137=EDGE_CURVE('',#13370,#12964,#11120,.T.);
#17138=EDGE_CURVE('',#13000,#13371,#7989,.T.);
#17139=EDGE_CURVE('',#13371,#13370,#7990,.T.);
#17140=EDGE_CURVE('',#13367,#13371,#11121,.T.);
#17141=EDGE_CURVE('',#13370,#13372,#7991,.T.);
#17142=EDGE_CURVE('',#12962,#13372,#11122,.T.);
#17143=EDGE_CURVE('',#13373,#13371,#7992,.T.);
#17144=EDGE_CURVE('',#13372,#13373,#7993,.T.);
#17145=EDGE_CURVE('',#13367,#13374,#7994,.T.);
#17146=EDGE_CURVE('',#13373,#13374,#11123,.T.);
#17147=EDGE_CURVE('',#13375,#13366,#7995,.T.);
#17148=EDGE_CURVE('',#13374,#13375,#7996,.T.);
#17149=EDGE_CURVE('',#13372,#13161,#7997,.T.);
#17150=EDGE_CURVE('',#13166,#13376,#7998,.T.);
#17151=EDGE_CURVE('',#13376,#12971,#11124,.T.);
#17152=EDGE_CURVE('',#13165,#13377,#7999,.T.);
#17153=EDGE_CURVE('',#13377,#13376,#8000,.T.);
#17154=EDGE_CURVE('',#13164,#13375,#8001,.T.);
#17155=EDGE_CURVE('',#13375,#13377,#11125,.T.);
#17156=EDGE_CURVE('',#13163,#13374,#8002,.T.);
#17157=EDGE_CURVE('',#13162,#13373,#8003,.T.);
#17158=EDGE_CURVE('',#13368,#13377,#8004,.T.);
#17159=EDGE_CURVE('',#13376,#13369,#8005,.T.);
#17160=EDGE_CURVE('',#13378,#13379,#8006,.T.);
#17161=EDGE_CURVE('',#13378,#13380,#1483,.T.);
#17162=EDGE_CURVE('',#13380,#13381,#11126,.T.);
#17163=EDGE_CURVE('',#13381,#13379,#1484,.T.);
#17164=EDGE_CURVE('',#13382,#13383,#8007,.T.);
#17165=EDGE_CURVE('',#13382,#13378,#1485,.T.);
#17166=EDGE_CURVE('',#13379,#13383,#1486,.T.);
#17167=EDGE_CURVE('',#13384,#13385,#8008,.T.);
#17168=EDGE_CURVE('',#13384,#13382,#1487,.T.);
#17169=EDGE_CURVE('',#13383,#13385,#1488,.T.);
#17170=EDGE_CURVE('',#13386,#13387,#8009,.T.);
#17171=EDGE_CURVE('',#13386,#13384,#1489,.T.);
#17172=EDGE_CURVE('',#13385,#13387,#1490,.T.);
#17173=EDGE_CURVE('',#13388,#13389,#8010,.T.);
#17174=EDGE_CURVE('',#13388,#13386,#1491,.T.);
#17175=EDGE_CURVE('',#13387,#13389,#1492,.T.);
#17176=EDGE_CURVE('',#13390,#13391,#8011,.T.);
#17177=EDGE_CURVE('',#13390,#13388,#1493,.T.);
#17178=EDGE_CURVE('',#13389,#13391,#1494,.T.);
#17179=EDGE_CURVE('',#13392,#13393,#8012,.T.);
#17180=EDGE_CURVE('',#13392,#13390,#1495,.T.);
#17181=EDGE_CURVE('',#13391,#13393,#1496,.T.);
#17182=EDGE_CURVE('',#13394,#13395,#8013,.T.);
#17183=EDGE_CURVE('',#13394,#13392,#1497,.T.);
#17184=EDGE_CURVE('',#13393,#13395,#1498,.T.);
#17185=EDGE_CURVE('',#13396,#13397,#8014,.T.);
#17186=EDGE_CURVE('',#13396,#13394,#1499,.T.);
#17187=EDGE_CURVE('',#13395,#13397,#1500,.T.);
#17188=EDGE_CURVE('',#13398,#13399,#8015,.T.);
#17189=EDGE_CURVE('',#13398,#13396,#1501,.T.);
#17190=EDGE_CURVE('',#13397,#13399,#1502,.T.);
#17191=EDGE_CURVE('',#13400,#13401,#8016,.T.);
#17192=EDGE_CURVE('',#13400,#13398,#1503,.T.);
#17193=EDGE_CURVE('',#13399,#13401,#1504,.T.);
#17194=EDGE_CURVE('',#13402,#13403,#8017,.T.);
#17195=EDGE_CURVE('',#13402,#13400,#1505,.T.);
#17196=EDGE_CURVE('',#13401,#13403,#1506,.T.);
#17197=EDGE_CURVE('',#13404,#13405,#8018,.T.);
#17198=EDGE_CURVE('',#13404,#13402,#1507,.T.);
#17199=EDGE_CURVE('',#13403,#13405,#1508,.T.);
#17200=EDGE_CURVE('',#13406,#13407,#8019,.T.);
#17201=EDGE_CURVE('',#13406,#13404,#1509,.T.);
#17202=EDGE_CURVE('',#13405,#13407,#1510,.T.);
#17203=EDGE_CURVE('',#13408,#13409,#8020,.T.);
#17204=EDGE_CURVE('',#13410,#13408,#11127,.T.);
#17205=EDGE_CURVE('',#13410,#13406,#1511,.T.);
#17206=EDGE_CURVE('',#13407,#13409,#1512,.T.);
#17207=EDGE_CURVE('',#13411,#13412,#8021,.T.);
#17208=EDGE_CURVE('',#13411,#13413,#1513,.T.);
#17209=EDGE_CURVE('',#13414,#13413,#11128,.T.);
#17210=EDGE_CURVE('',#13412,#13414,#1514,.T.);
#17211=EDGE_CURVE('',#13415,#13416,#8022,.T.);
#17212=EDGE_CURVE('',#13415,#13411,#1515,.T.);
#17213=EDGE_CURVE('',#13416,#13412,#1516,.T.);
#17214=EDGE_CURVE('',#13417,#13418,#8023,.T.);
#17215=EDGE_CURVE('',#13417,#13415,#1517,.T.);
#17216=EDGE_CURVE('',#13418,#13416,#1518,.T.);
#17217=EDGE_CURVE('',#13419,#13420,#8024,.T.);
#17218=EDGE_CURVE('',#13419,#13417,#1519,.T.);
#17219=EDGE_CURVE('',#13420,#13418,#1520,.T.);
#17220=EDGE_CURVE('',#13421,#13422,#8025,.T.);
#17221=EDGE_CURVE('',#13421,#13419,#1521,.T.);
#17222=EDGE_CURVE('',#13422,#13420,#1522,.T.);
#17223=EDGE_CURVE('',#13423,#13424,#8026,.T.);
#17224=EDGE_CURVE('',#13423,#13421,#1523,.T.);
#17225=EDGE_CURVE('',#13424,#13422,#1524,.T.);
#17226=EDGE_CURVE('',#13425,#13426,#8027,.T.);
#17227=EDGE_CURVE('',#13425,#13423,#1525,.T.);
#17228=EDGE_CURVE('',#13426,#13424,#1526,.T.);
#17229=EDGE_CURVE('',#13427,#13428,#8028,.T.);
#17230=EDGE_CURVE('',#13427,#13425,#1527,.T.);
#17231=EDGE_CURVE('',#13428,#13426,#1528,.T.);
#17232=EDGE_CURVE('',#13429,#13430,#8029,.T.);
#17233=EDGE_CURVE('',#13429,#13427,#1529,.T.);
#17234=EDGE_CURVE('',#13430,#13428,#1530,.T.);
#17235=EDGE_CURVE('',#13431,#13432,#8030,.T.);
#17236=EDGE_CURVE('',#13431,#13429,#1531,.T.);
#17237=EDGE_CURVE('',#13432,#13430,#1532,.T.);
#17238=EDGE_CURVE('',#13433,#13434,#8031,.T.);
#17239=EDGE_CURVE('',#13433,#13431,#1533,.T.);
#17240=EDGE_CURVE('',#13434,#13432,#1534,.T.);
#17241=EDGE_CURVE('',#13435,#13436,#8032,.T.);
#17242=EDGE_CURVE('',#13435,#13433,#1535,.T.);
#17243=EDGE_CURVE('',#13436,#13434,#1536,.T.);
#17244=EDGE_CURVE('',#13437,#13438,#8033,.T.);
#17245=EDGE_CURVE('',#13437,#13435,#1537,.T.);
#17246=EDGE_CURVE('',#13438,#13436,#1538,.T.);
#17247=EDGE_CURVE('',#13439,#13440,#8034,.T.);
#17248=EDGE_CURVE('',#13439,#13437,#1539,.T.);
#17249=EDGE_CURVE('',#13440,#13438,#1540,.T.);
#17250=EDGE_CURVE('',#13441,#13442,#1541,.T.);
#17251=EDGE_CURVE('',#13441,#13443,#8035,.T.);
#17252=EDGE_CURVE('',#13443,#13444,#1542,.T.);
#17253=EDGE_CURVE('',#13442,#13444,#8036,.T.);
#17254=EDGE_CURVE('',#13445,#13441,#1543,.T.);
#17255=EDGE_CURVE('',#13445,#13446,#8037,.T.);
#17256=EDGE_CURVE('',#13446,#13443,#1544,.T.);
#17257=EDGE_CURVE('',#13447,#13445,#1545,.T.);
#17258=EDGE_CURVE('',#13447,#13448,#8038,.T.);
#17259=EDGE_CURVE('',#13448,#13446,#1546,.T.);
#17260=EDGE_CURVE('',#13449,#13447,#1547,.T.);
#17261=EDGE_CURVE('',#13449,#13450,#8039,.T.);
#17262=EDGE_CURVE('',#13450,#13448,#1548,.T.);
#17263=EDGE_CURVE('',#13451,#13449,#1549,.T.);
#17264=EDGE_CURVE('',#13451,#13452,#8040,.T.);
#17265=EDGE_CURVE('',#13452,#13450,#1550,.T.);
#17266=EDGE_CURVE('',#13453,#13451,#1551,.T.);
#17267=EDGE_CURVE('',#13453,#13454,#8041,.T.);
#17268=EDGE_CURVE('',#13454,#13452,#1552,.T.);
#17269=EDGE_CURVE('',#13455,#13453,#1553,.T.);
#17270=EDGE_CURVE('',#13455,#13456,#8042,.T.);
#17271=EDGE_CURVE('',#13456,#13454,#1554,.T.);
#17272=EDGE_CURVE('',#13442,#13455,#1555,.T.);
#17273=EDGE_CURVE('',#13444,#13456,#1556,.T.);
#17274=EDGE_CURVE('',#13457,#13458,#1557,.T.);
#17275=EDGE_CURVE('',#13457,#13459,#8043,.T.);
#17276=EDGE_CURVE('',#13459,#13460,#1558,.T.);
#17277=EDGE_CURVE('',#13458,#13460,#8044,.T.);
#17278=EDGE_CURVE('',#13461,#13457,#1559,.T.);
#17279=EDGE_CURVE('',#13461,#13462,#8045,.T.);
#17280=EDGE_CURVE('',#13462,#13459,#1560,.T.);
#17281=EDGE_CURVE('',#13463,#13461,#1561,.T.);
#17282=EDGE_CURVE('',#13463,#13464,#8046,.T.);
#17283=EDGE_CURVE('',#13464,#13462,#1562,.T.);
#17284=EDGE_CURVE('',#13465,#13463,#1563,.T.);
#17285=EDGE_CURVE('',#13465,#13466,#8047,.T.);
#17286=EDGE_CURVE('',#13466,#13464,#1564,.T.);
#17287=EDGE_CURVE('',#13467,#13465,#1565,.T.);
#17288=EDGE_CURVE('',#13467,#13468,#8048,.T.);
#17289=EDGE_CURVE('',#13468,#13466,#1566,.T.);
#17290=EDGE_CURVE('',#13469,#13467,#1567,.T.);
#17291=EDGE_CURVE('',#13469,#13470,#8049,.T.);
#17292=EDGE_CURVE('',#13470,#13468,#1568,.T.);
#17293=EDGE_CURVE('',#13471,#13469,#1569,.T.);
#17294=EDGE_CURVE('',#13471,#13472,#8050,.T.);
#17295=EDGE_CURVE('',#13472,#13470,#1570,.T.);
#17296=EDGE_CURVE('',#13473,#13471,#1571,.T.);
#17297=EDGE_CURVE('',#13473,#13474,#8051,.T.);
#17298=EDGE_CURVE('',#13474,#13472,#1572,.T.);
#17299=EDGE_CURVE('',#13458,#13473,#1573,.T.);
#17300=EDGE_CURVE('',#13460,#13474,#1574,.T.);
#17301=EDGE_CURVE('',#13475,#13476,#1575,.T.);
#17302=EDGE_CURVE('',#13475,#13477,#8052,.T.);
#17303=EDGE_CURVE('',#13477,#13478,#1576,.T.);
#17304=EDGE_CURVE('',#13476,#13478,#8053,.T.);
#17305=EDGE_CURVE('',#13479,#13475,#1577,.T.);
#17306=EDGE_CURVE('',#13479,#13480,#8054,.T.);
#17307=EDGE_CURVE('',#13480,#13477,#1578,.T.);
#17308=EDGE_CURVE('',#13481,#13479,#1579,.T.);
#17309=EDGE_CURVE('',#13481,#13482,#8055,.T.);
#17310=EDGE_CURVE('',#13482,#13480,#1580,.T.);
#17311=EDGE_CURVE('',#13483,#13481,#1581,.T.);
#17312=EDGE_CURVE('',#13483,#13484,#8056,.T.);
#17313=EDGE_CURVE('',#13484,#13482,#1582,.T.);
#17314=EDGE_CURVE('',#13485,#13483,#1583,.T.);
#17315=EDGE_CURVE('',#13485,#13486,#8057,.T.);
#17316=EDGE_CURVE('',#13486,#13484,#1584,.T.);
#17317=EDGE_CURVE('',#13487,#13485,#1585,.T.);
#17318=EDGE_CURVE('',#13487,#13488,#8058,.T.);
#17319=EDGE_CURVE('',#13488,#13486,#1586,.T.);
#17320=EDGE_CURVE('',#13489,#13487,#1587,.T.);
#17321=EDGE_CURVE('',#13489,#13490,#8059,.T.);
#17322=EDGE_CURVE('',#13490,#13488,#1588,.T.);
#17323=EDGE_CURVE('',#13491,#13489,#1589,.T.);
#17324=EDGE_CURVE('',#13491,#13492,#8060,.T.);
#17325=EDGE_CURVE('',#13492,#13490,#1590,.T.);
#17326=EDGE_CURVE('',#13493,#13491,#1591,.T.);
#17327=EDGE_CURVE('',#13493,#13494,#8061,.T.);
#17328=EDGE_CURVE('',#13494,#13492,#1592,.T.);
#17329=EDGE_CURVE('',#13495,#13493,#1593,.T.);
#17330=EDGE_CURVE('',#13495,#13496,#8062,.T.);
#17331=EDGE_CURVE('',#13496,#13494,#1594,.T.);
#17332=EDGE_CURVE('',#13497,#13495,#1595,.T.);
#17333=EDGE_CURVE('',#13497,#13498,#8063,.T.);
#17334=EDGE_CURVE('',#13498,#13496,#1596,.T.);
#17335=EDGE_CURVE('',#13499,#13497,#1597,.T.);
#17336=EDGE_CURVE('',#13499,#13500,#8064,.T.);
#17337=EDGE_CURVE('',#13500,#13498,#1598,.T.);
#17338=EDGE_CURVE('',#13501,#13499,#1599,.T.);
#17339=EDGE_CURVE('',#13501,#13502,#8065,.T.);
#17340=EDGE_CURVE('',#13502,#13500,#1600,.T.);
#17341=EDGE_CURVE('',#13503,#13501,#1601,.T.);
#17342=EDGE_CURVE('',#13503,#13504,#8066,.T.);
#17343=EDGE_CURVE('',#13504,#13502,#1602,.T.);
#17344=EDGE_CURVE('',#13505,#13503,#1603,.T.);
#17345=EDGE_CURVE('',#13505,#13506,#8067,.T.);
#17346=EDGE_CURVE('',#13506,#13504,#1604,.T.);
#17347=EDGE_CURVE('',#13476,#13505,#1605,.T.);
#17348=EDGE_CURVE('',#13478,#13506,#1606,.T.);
#17349=EDGE_CURVE('',#13507,#13508,#8068,.T.);
#17350=EDGE_CURVE('',#13507,#13509,#8069,.T.);
#17351=EDGE_CURVE('',#13509,#13510,#8070,.T.);
#17352=EDGE_CURVE('',#13508,#13510,#8071,.T.);
#17353=EDGE_CURVE('',#13511,#13507,#8072,.T.);
#17354=EDGE_CURVE('',#13511,#13512,#8073,.T.);
#17355=EDGE_CURVE('',#13512,#13509,#8074,.T.);
#17356=EDGE_CURVE('',#13513,#13511,#8075,.T.);
#17357=EDGE_CURVE('',#13513,#13514,#8076,.T.);
#17358=EDGE_CURVE('',#13514,#13512,#8077,.T.);
#17359=EDGE_CURVE('',#13508,#13513,#8078,.T.);
#17360=EDGE_CURVE('',#13510,#13514,#8079,.T.);
#17361=EDGE_CURVE('',#13515,#13516,#1607,.T.);
#17362=EDGE_CURVE('',#13515,#13517,#8080,.T.);
#17363=EDGE_CURVE('',#13517,#13518,#1608,.T.);
#17364=EDGE_CURVE('',#13516,#13518,#8081,.T.);
#17365=EDGE_CURVE('',#13519,#13515,#1609,.T.);
#17366=EDGE_CURVE('',#13519,#13520,#8082,.T.);
#17367=EDGE_CURVE('',#13520,#13517,#1610,.T.);
#17368=EDGE_CURVE('',#13521,#13519,#1611,.T.);
#17369=EDGE_CURVE('',#13521,#13522,#8083,.T.);
#17370=EDGE_CURVE('',#13522,#13520,#1612,.T.);
#17371=EDGE_CURVE('',#13523,#13521,#1613,.T.);
#17372=EDGE_CURVE('',#13523,#13524,#8084,.T.);
#17373=EDGE_CURVE('',#13524,#13522,#1614,.T.);
#17374=EDGE_CURVE('',#13525,#13523,#1615,.T.);
#17375=EDGE_CURVE('',#13525,#13526,#8085,.T.);
#17376=EDGE_CURVE('',#13526,#13524,#1616,.T.);
#17377=EDGE_CURVE('',#13527,#13525,#1617,.T.);
#17378=EDGE_CURVE('',#13527,#13528,#8086,.T.);
#17379=EDGE_CURVE('',#13528,#13526,#1618,.T.);
#17380=EDGE_CURVE('',#13529,#13527,#1619,.T.);
#17381=EDGE_CURVE('',#13529,#13530,#8087,.T.);
#17382=EDGE_CURVE('',#13530,#13528,#1620,.T.);
#17383=EDGE_CURVE('',#13516,#13529,#1621,.T.);
#17384=EDGE_CURVE('',#13518,#13530,#1622,.T.);
#17385=EDGE_CURVE('',#13531,#13532,#1623,.T.);
#17386=EDGE_CURVE('',#13531,#13533,#8088,.T.);
#17387=EDGE_CURVE('',#13533,#13534,#1624,.T.);
#17388=EDGE_CURVE('',#13532,#13534,#8089,.T.);
#17389=EDGE_CURVE('',#13535,#13531,#1625,.T.);
#17390=EDGE_CURVE('',#13535,#13536,#8090,.T.);
#17391=EDGE_CURVE('',#13536,#13533,#1626,.T.);
#17392=EDGE_CURVE('',#13537,#13535,#1627,.T.);
#17393=EDGE_CURVE('',#13537,#13538,#8091,.T.);
#17394=EDGE_CURVE('',#13538,#13536,#1628,.T.);
#17395=EDGE_CURVE('',#13539,#13537,#1629,.T.);
#17396=EDGE_CURVE('',#13539,#13540,#8092,.T.);
#17397=EDGE_CURVE('',#13540,#13538,#1630,.T.);
#17398=EDGE_CURVE('',#13541,#13539,#1631,.T.);
#17399=EDGE_CURVE('',#13541,#13542,#8093,.T.);
#17400=EDGE_CURVE('',#13542,#13540,#1632,.T.);
#17401=EDGE_CURVE('',#13543,#13541,#1633,.T.);
#17402=EDGE_CURVE('',#13543,#13544,#8094,.T.);
#17403=EDGE_CURVE('',#13544,#13542,#1634,.T.);
#17404=EDGE_CURVE('',#13545,#13543,#1635,.T.);
#17405=EDGE_CURVE('',#13545,#13546,#8095,.T.);
#17406=EDGE_CURVE('',#13546,#13544,#1636,.T.);
#17407=EDGE_CURVE('',#13547,#13545,#1637,.T.);
#17408=EDGE_CURVE('',#13547,#13548,#8096,.T.);
#17409=EDGE_CURVE('',#13548,#13546,#1638,.T.);
#17410=EDGE_CURVE('',#13532,#13547,#1639,.T.);
#17411=EDGE_CURVE('',#13534,#13548,#1640,.T.);
#17412=EDGE_CURVE('',#13549,#13550,#1641,.T.);
#17413=EDGE_CURVE('',#13549,#13551,#8097,.T.);
#17414=EDGE_CURVE('',#13551,#13552,#1642,.T.);
#17415=EDGE_CURVE('',#13550,#13552,#8098,.T.);
#17416=EDGE_CURVE('',#13553,#13549,#1643,.T.);
#17417=EDGE_CURVE('',#13553,#13554,#8099,.T.);
#17418=EDGE_CURVE('',#13554,#13551,#1644,.T.);
#17419=EDGE_CURVE('',#13555,#13553,#1645,.T.);
#17420=EDGE_CURVE('',#13555,#13556,#8100,.T.);
#17421=EDGE_CURVE('',#13556,#13554,#1646,.T.);
#17422=EDGE_CURVE('',#13557,#13555,#1647,.T.);
#17423=EDGE_CURVE('',#13557,#13558,#8101,.T.);
#17424=EDGE_CURVE('',#13558,#13556,#1648,.T.);
#17425=EDGE_CURVE('',#13559,#13557,#1649,.T.);
#17426=EDGE_CURVE('',#13559,#13560,#8102,.T.);
#17427=EDGE_CURVE('',#13560,#13558,#1650,.T.);
#17428=EDGE_CURVE('',#13561,#13559,#1651,.T.);
#17429=EDGE_CURVE('',#13561,#13562,#8103,.T.);
#17430=EDGE_CURVE('',#13562,#13560,#1652,.T.);
#17431=EDGE_CURVE('',#13563,#13561,#1653,.T.);
#17432=EDGE_CURVE('',#13563,#13564,#8104,.T.);
#17433=EDGE_CURVE('',#13564,#13562,#1654,.T.);
#17434=EDGE_CURVE('',#13565,#13563,#1655,.T.);
#17435=EDGE_CURVE('',#13565,#13566,#8105,.T.);
#17436=EDGE_CURVE('',#13566,#13564,#1656,.T.);
#17437=EDGE_CURVE('',#13567,#13565,#1657,.T.);
#17438=EDGE_CURVE('',#13567,#13568,#8106,.T.);
#17439=EDGE_CURVE('',#13568,#13566,#1658,.T.);
#17440=EDGE_CURVE('',#13569,#13567,#1659,.T.);
#17441=EDGE_CURVE('',#13569,#13570,#8107,.T.);
#17442=EDGE_CURVE('',#13570,#13568,#1660,.T.);
#17443=EDGE_CURVE('',#13571,#13569,#1661,.T.);
#17444=EDGE_CURVE('',#13571,#13572,#8108,.T.);
#17445=EDGE_CURVE('',#13572,#13570,#1662,.T.);
#17446=EDGE_CURVE('',#13573,#13571,#1663,.T.);
#17447=EDGE_CURVE('',#13573,#13574,#8109,.T.);
#17448=EDGE_CURVE('',#13574,#13572,#1664,.T.);
#17449=EDGE_CURVE('',#13575,#13573,#1665,.T.);
#17450=EDGE_CURVE('',#13575,#13576,#8110,.T.);
#17451=EDGE_CURVE('',#13576,#13574,#1666,.T.);
#17452=EDGE_CURVE('',#13577,#13575,#1667,.T.);
#17453=EDGE_CURVE('',#13577,#13578,#8111,.T.);
#17454=EDGE_CURVE('',#13578,#13576,#1668,.T.);
#17455=EDGE_CURVE('',#13579,#13577,#1669,.T.);
#17456=EDGE_CURVE('',#13579,#13580,#8112,.T.);
#17457=EDGE_CURVE('',#13580,#13578,#1670,.T.);
#17458=EDGE_CURVE('',#13550,#13579,#1671,.T.);
#17459=EDGE_CURVE('',#13552,#13580,#1672,.T.);
#17460=EDGE_CURVE('',#13413,#13410,#1673,.T.);
#17461=EDGE_CURVE('',#13581,#13410,#11129,.T.);
#17462=EDGE_CURVE('',#13582,#13581,#11130,.T.);
#17463=EDGE_CURVE('',#13582,#13414,#1674,.T.);
#17464=EDGE_CURVE('',#13409,#13582,#1675,.T.);
#17465=EDGE_CURVE('',#13583,#13381,#1676,.T.);
#17466=EDGE_CURVE('',#13583,#13440,#1677,.T.);
#17467=EDGE_CURVE('',#13381,#13584,#11131,.T.);
#17468=EDGE_CURVE('',#13584,#13380,#11132,.T.);
#17469=EDGE_CURVE('',#13380,#13585,#1678,.T.);
#17470=EDGE_CURVE('',#13585,#13583,#11133,.T.);
#17471=EDGE_CURVE('',#13585,#13439,#1679,.T.);
#17472=EDGE_CURVE('',#13586,#13586,#11134,.T.);
#17473=EDGE_CURVE('',#13586,#13581,#11135,.T.);
#17474=EDGE_CURVE('',#13408,#13582,#11136,.T.);
#17475=EDGE_CURVE('',#13587,#13588,#8113,.T.);
#17476=EDGE_CURVE('',#13589,#13587,#8114,.T.);
#17477=EDGE_CURVE('',#13590,#13589,#8115,.T.);
#17478=EDGE_CURVE('',#13591,#13590,#8116,.T.);
#17479=EDGE_CURVE('',#13592,#13591,#8117,.T.);
#17480=EDGE_CURVE('',#13588,#13592,#8118,.T.);
#17481=EDGE_CURVE('',#13593,#13594,#263,.T.);
#17482=EDGE_CURVE('',#13595,#13593,#264,.T.);
#17483=EDGE_CURVE('',#13596,#13595,#265,.T.);
#17484=EDGE_CURVE('',#13597,#13596,#266,.T.);
#17485=EDGE_CURVE('',#13598,#13597,#267,.T.);
#17486=EDGE_CURVE('',#13598,#13599,#8119,.T.);
#17487=EDGE_CURVE('',#13599,#13599,#11137,.T.);
#17488=EDGE_CURVE('',#13600,#13598,#268,.T.);
#17489=EDGE_CURVE('',#13594,#13600,#269,.T.);
#17490=EDGE_CURVE('',#13592,#13596,#8120,.T.);
#17491=EDGE_CURVE('',#13591,#13597,#8121,.T.);
#17492=EDGE_CURVE('',#13588,#13595,#8122,.T.);
#17493=EDGE_CURVE('',#13587,#13593,#8123,.T.);
#17494=EDGE_CURVE('',#13589,#13594,#8124,.T.);
#17495=EDGE_CURVE('',#13590,#13600,#8125,.T.);
#17496=EDGE_CURVE('',#13601,#13601,#11138,.T.);
#17497=EDGE_CURVE('',#13584,#13601,#8126,.T.);
#17498=ORIENTED_EDGE('',*,*,#13602,.T.);
#17499=ORIENTED_EDGE('',*,*,#13603,.T.);
#17500=ORIENTED_EDGE('',*,*,#13604,.T.);
#17501=ORIENTED_EDGE('',*,*,#13605,.T.);
#17502=ORIENTED_EDGE('',*,*,#13604,.F.);
#17503=ORIENTED_EDGE('',*,*,#13605,.F.);
#17504=ORIENTED_EDGE('',*,*,#13606,.T.);
#17505=ORIENTED_EDGE('',*,*,#13607,.T.);
#17506=ORIENTED_EDGE('',*,*,#13608,.T.);
#17507=ORIENTED_EDGE('',*,*,#13609,.T.);
#17508=ORIENTED_EDGE('',*,*,#13610,.T.);
#17509=ORIENTED_EDGE('',*,*,#13611,.T.);
#17510=ORIENTED_EDGE('',*,*,#13612,.T.);
#17511=ORIENTED_EDGE('',*,*,#13613,.T.);
#17512=ORIENTED_EDGE('',*,*,#13614,.T.);
#17513=ORIENTED_EDGE('',*,*,#13615,.T.);
#17514=ORIENTED_EDGE('',*,*,#13616,.T.);
#17515=ORIENTED_EDGE('',*,*,#13617,.T.);
#17516=ORIENTED_EDGE('',*,*,#13618,.T.);
#17517=ORIENTED_EDGE('',*,*,#13619,.T.);
#17518=ORIENTED_EDGE('',*,*,#13620,.T.);
#17519=ORIENTED_EDGE('',*,*,#13621,.T.);
#17520=ORIENTED_EDGE('',*,*,#13622,.T.);
#17521=ORIENTED_EDGE('',*,*,#13623,.T.);
#17522=ORIENTED_EDGE('',*,*,#13624,.T.);
#17523=ORIENTED_EDGE('',*,*,#13625,.T.);
#17524=ORIENTED_EDGE('',*,*,#13626,.T.);
#17525=ORIENTED_EDGE('',*,*,#13627,.T.);
#17526=ORIENTED_EDGE('',*,*,#13628,.T.);
#17527=ORIENTED_EDGE('',*,*,#13629,.T.);
#17528=ORIENTED_EDGE('',*,*,#13630,.T.);
#17529=ORIENTED_EDGE('',*,*,#13631,.T.);
#17530=ORIENTED_EDGE('',*,*,#13632,.T.);
#17531=ORIENTED_EDGE('',*,*,#13633,.T.);
#17532=ORIENTED_EDGE('',*,*,#13634,.T.);
#17533=ORIENTED_EDGE('',*,*,#13635,.T.);
#17534=ORIENTED_EDGE('',*,*,#13636,.T.);
#17535=ORIENTED_EDGE('',*,*,#13637,.T.);
#17536=ORIENTED_EDGE('',*,*,#13638,.T.);
#17537=ORIENTED_EDGE('',*,*,#13639,.T.);
#17538=ORIENTED_EDGE('',*,*,#13640,.T.);
#17539=ORIENTED_EDGE('',*,*,#13641,.T.);
#17540=ORIENTED_EDGE('',*,*,#13642,.T.);
#17541=ORIENTED_EDGE('',*,*,#13643,.T.);
#17542=ORIENTED_EDGE('',*,*,#13644,.T.);
#17543=ORIENTED_EDGE('',*,*,#13645,.T.);
#17544=ORIENTED_EDGE('',*,*,#13646,.T.);
#17545=ORIENTED_EDGE('',*,*,#13647,.T.);
#17546=ORIENTED_EDGE('',*,*,#13648,.T.);
#17547=ORIENTED_EDGE('',*,*,#13649,.T.);
#17548=ORIENTED_EDGE('',*,*,#13650,.T.);
#17549=ORIENTED_EDGE('',*,*,#13651,.T.);
#17550=ORIENTED_EDGE('',*,*,#13652,.T.);
#17551=ORIENTED_EDGE('',*,*,#13653,.T.);
#17552=ORIENTED_EDGE('',*,*,#13654,.T.);
#17553=ORIENTED_EDGE('',*,*,#13655,.T.);
#17554=ORIENTED_EDGE('',*,*,#13656,.T.);
#17555=ORIENTED_EDGE('',*,*,#13657,.T.);
#17556=ORIENTED_EDGE('',*,*,#13658,.T.);
#17557=ORIENTED_EDGE('',*,*,#13659,.T.);
#17558=ORIENTED_EDGE('',*,*,#13660,.T.);
#17559=ORIENTED_EDGE('',*,*,#13661,.T.);
#17560=ORIENTED_EDGE('',*,*,#13662,.T.);
#17561=ORIENTED_EDGE('',*,*,#13663,.T.);
#17562=ORIENTED_EDGE('',*,*,#13664,.T.);
#17563=ORIENTED_EDGE('',*,*,#13665,.T.);
#17564=ORIENTED_EDGE('',*,*,#13666,.T.);
#17565=ORIENTED_EDGE('',*,*,#13667,.T.);
#17566=ORIENTED_EDGE('',*,*,#13668,.T.);
#17567=ORIENTED_EDGE('',*,*,#13669,.T.);
#17568=ORIENTED_EDGE('',*,*,#13670,.T.);
#17569=ORIENTED_EDGE('',*,*,#13671,.T.);
#17570=ORIENTED_EDGE('',*,*,#13672,.T.);
#17571=ORIENTED_EDGE('',*,*,#13673,.T.);
#17572=ORIENTED_EDGE('',*,*,#13674,.T.);
#17573=ORIENTED_EDGE('',*,*,#13675,.T.);
#17574=ORIENTED_EDGE('',*,*,#13676,.T.);
#17575=ORIENTED_EDGE('',*,*,#13677,.T.);
#17576=ORIENTED_EDGE('',*,*,#13678,.T.);
#17577=ORIENTED_EDGE('',*,*,#13679,.T.);
#17578=ORIENTED_EDGE('',*,*,#13680,.T.);
#17579=ORIENTED_EDGE('',*,*,#13681,.T.);
#17580=ORIENTED_EDGE('',*,*,#13682,.T.);
#17581=ORIENTED_EDGE('',*,*,#13683,.T.);
#17582=ORIENTED_EDGE('',*,*,#13684,.T.);
#17583=ORIENTED_EDGE('',*,*,#13685,.T.);
#17584=ORIENTED_EDGE('',*,*,#13686,.T.);
#17585=ORIENTED_EDGE('',*,*,#13687,.T.);
#17586=ORIENTED_EDGE('',*,*,#13688,.T.);
#17587=ORIENTED_EDGE('',*,*,#13689,.T.);
#17588=ORIENTED_EDGE('',*,*,#13690,.T.);
#17589=ORIENTED_EDGE('',*,*,#13691,.T.);
#17590=ORIENTED_EDGE('',*,*,#13692,.T.);
#17591=ORIENTED_EDGE('',*,*,#13693,.T.);
#17592=ORIENTED_EDGE('',*,*,#13694,.T.);
#17593=ORIENTED_EDGE('',*,*,#13695,.T.);
#17594=ORIENTED_EDGE('',*,*,#13696,.T.);
#17595=ORIENTED_EDGE('',*,*,#13697,.T.);
#17596=ORIENTED_EDGE('',*,*,#13698,.T.);
#17597=ORIENTED_EDGE('',*,*,#13699,.T.);
#17598=ORIENTED_EDGE('',*,*,#13700,.T.);
#17599=ORIENTED_EDGE('',*,*,#13701,.T.);
#17600=ORIENTED_EDGE('',*,*,#13702,.T.);
#17601=ORIENTED_EDGE('',*,*,#13703,.T.);
#17602=ORIENTED_EDGE('',*,*,#13704,.T.);
#17603=ORIENTED_EDGE('',*,*,#13705,.T.);
#17604=ORIENTED_EDGE('',*,*,#13706,.T.);
#17605=ORIENTED_EDGE('',*,*,#13707,.T.);
#17606=ORIENTED_EDGE('',*,*,#13708,.T.);
#17607=ORIENTED_EDGE('',*,*,#13709,.T.);
#17608=ORIENTED_EDGE('',*,*,#13710,.T.);
#17609=ORIENTED_EDGE('',*,*,#13711,.T.);
#17610=ORIENTED_EDGE('',*,*,#13712,.T.);
#17611=ORIENTED_EDGE('',*,*,#13713,.T.);
#17612=ORIENTED_EDGE('',*,*,#13714,.F.);
#17613=ORIENTED_EDGE('',*,*,#13715,.T.);
#17614=ORIENTED_EDGE('',*,*,#13602,.F.);
#17615=ORIENTED_EDGE('',*,*,#13603,.F.);
#17616=ORIENTED_EDGE('',*,*,#13715,.F.);
#17617=ORIENTED_EDGE('',*,*,#13716,.T.);
#17618=ORIENTED_EDGE('',*,*,#13717,.T.);
#17619=ORIENTED_EDGE('',*,*,#13718,.T.);
#17620=ORIENTED_EDGE('',*,*,#13719,.T.);
#17621=ORIENTED_EDGE('',*,*,#13717,.F.);
#17622=ORIENTED_EDGE('',*,*,#13716,.F.);
#17623=ORIENTED_EDGE('',*,*,#13720,.T.);
#17624=ORIENTED_EDGE('',*,*,#13721,.T.);
#17625=ORIENTED_EDGE('',*,*,#13722,.T.);
#17626=ORIENTED_EDGE('',*,*,#13723,.T.);
#17627=ORIENTED_EDGE('',*,*,#13724,.T.);
#17628=ORIENTED_EDGE('',*,*,#13725,.T.);
#17629=ORIENTED_EDGE('',*,*,#13726,.T.);
#17630=ORIENTED_EDGE('',*,*,#13727,.T.);
#17631=ORIENTED_EDGE('',*,*,#13728,.T.);
#17632=ORIENTED_EDGE('',*,*,#13729,.T.);
#17633=ORIENTED_EDGE('',*,*,#13730,.T.);
#17634=ORIENTED_EDGE('',*,*,#13731,.T.);
#17635=ORIENTED_EDGE('',*,*,#13732,.T.);
#17636=ORIENTED_EDGE('',*,*,#13733,.T.);
#17637=ORIENTED_EDGE('',*,*,#13734,.T.);
#17638=ORIENTED_EDGE('',*,*,#13735,.T.);
#17639=ORIENTED_EDGE('',*,*,#13736,.T.);
#17640=ORIENTED_EDGE('',*,*,#13737,.T.);
#17641=ORIENTED_EDGE('',*,*,#13738,.T.);
#17642=ORIENTED_EDGE('',*,*,#13739,.T.);
#17643=ORIENTED_EDGE('',*,*,#13740,.T.);
#17644=ORIENTED_EDGE('',*,*,#13741,.T.);
#17645=ORIENTED_EDGE('',*,*,#13742,.T.);
#17646=ORIENTED_EDGE('',*,*,#13743,.T.);
#17647=ORIENTED_EDGE('',*,*,#13744,.T.);
#17648=ORIENTED_EDGE('',*,*,#13745,.T.);
#17649=ORIENTED_EDGE('',*,*,#13746,.T.);
#17650=ORIENTED_EDGE('',*,*,#13747,.T.);
#17651=ORIENTED_EDGE('',*,*,#13748,.T.);
#17652=ORIENTED_EDGE('',*,*,#13749,.T.);
#17653=ORIENTED_EDGE('',*,*,#13750,.T.);
#17654=ORIENTED_EDGE('',*,*,#13751,.T.);
#17655=ORIENTED_EDGE('',*,*,#13752,.T.);
#17656=ORIENTED_EDGE('',*,*,#13753,.T.);
#17657=ORIENTED_EDGE('',*,*,#13754,.T.);
#17658=ORIENTED_EDGE('',*,*,#13755,.T.);
#17659=ORIENTED_EDGE('',*,*,#13756,.T.);
#17660=ORIENTED_EDGE('',*,*,#13757,.T.);
#17661=ORIENTED_EDGE('',*,*,#13758,.T.);
#17662=ORIENTED_EDGE('',*,*,#13759,.T.);
#17663=ORIENTED_EDGE('',*,*,#13760,.T.);
#17664=ORIENTED_EDGE('',*,*,#13761,.T.);
#17665=ORIENTED_EDGE('',*,*,#13762,.T.);
#17666=ORIENTED_EDGE('',*,*,#13763,.T.);
#17667=ORIENTED_EDGE('',*,*,#13764,.T.);
#17668=ORIENTED_EDGE('',*,*,#13765,.T.);
#17669=ORIENTED_EDGE('',*,*,#13766,.T.);
#17670=ORIENTED_EDGE('',*,*,#13767,.T.);
#17671=ORIENTED_EDGE('',*,*,#13768,.T.);
#17672=ORIENTED_EDGE('',*,*,#13769,.T.);
#17673=ORIENTED_EDGE('',*,*,#13770,.T.);
#17674=ORIENTED_EDGE('',*,*,#13771,.T.);
#17675=ORIENTED_EDGE('',*,*,#13772,.T.);
#17676=ORIENTED_EDGE('',*,*,#13773,.T.);
#17677=ORIENTED_EDGE('',*,*,#13774,.T.);
#17678=ORIENTED_EDGE('',*,*,#13775,.T.);
#17679=ORIENTED_EDGE('',*,*,#13776,.T.);
#17680=ORIENTED_EDGE('',*,*,#13777,.T.);
#17681=ORIENTED_EDGE('',*,*,#13778,.T.);
#17682=ORIENTED_EDGE('',*,*,#13779,.T.);
#17683=ORIENTED_EDGE('',*,*,#13780,.T.);
#17684=ORIENTED_EDGE('',*,*,#13781,.T.);
#17685=ORIENTED_EDGE('',*,*,#13782,.T.);
#17686=ORIENTED_EDGE('',*,*,#13783,.T.);
#17687=ORIENTED_EDGE('',*,*,#13784,.T.);
#17688=ORIENTED_EDGE('',*,*,#13785,.T.);
#17689=ORIENTED_EDGE('',*,*,#13786,.T.);
#17690=ORIENTED_EDGE('',*,*,#13787,.T.);
#17691=ORIENTED_EDGE('',*,*,#13788,.T.);
#17692=ORIENTED_EDGE('',*,*,#13789,.T.);
#17693=ORIENTED_EDGE('',*,*,#13790,.T.);
#17694=ORIENTED_EDGE('',*,*,#13791,.T.);
#17695=ORIENTED_EDGE('',*,*,#13792,.T.);
#17696=ORIENTED_EDGE('',*,*,#13793,.T.);
#17697=ORIENTED_EDGE('',*,*,#13794,.T.);
#17698=ORIENTED_EDGE('',*,*,#13795,.T.);
#17699=ORIENTED_EDGE('',*,*,#13796,.T.);
#17700=ORIENTED_EDGE('',*,*,#13797,.T.);
#17701=ORIENTED_EDGE('',*,*,#13798,.T.);
#17702=ORIENTED_EDGE('',*,*,#13799,.T.);
#17703=ORIENTED_EDGE('',*,*,#13800,.T.);
#17704=ORIENTED_EDGE('',*,*,#13801,.T.);
#17705=ORIENTED_EDGE('',*,*,#13802,.T.);
#17706=ORIENTED_EDGE('',*,*,#13803,.T.);
#17707=ORIENTED_EDGE('',*,*,#13804,.T.);
#17708=ORIENTED_EDGE('',*,*,#13805,.T.);
#17709=ORIENTED_EDGE('',*,*,#13806,.T.);
#17710=ORIENTED_EDGE('',*,*,#13807,.T.);
#17711=ORIENTED_EDGE('',*,*,#13808,.T.);
#17712=ORIENTED_EDGE('',*,*,#13809,.T.);
#17713=ORIENTED_EDGE('',*,*,#13810,.T.);
#17714=ORIENTED_EDGE('',*,*,#13811,.T.);
#17715=ORIENTED_EDGE('',*,*,#13812,.T.);
#17716=ORIENTED_EDGE('',*,*,#13813,.T.);
#17717=ORIENTED_EDGE('',*,*,#13814,.T.);
#17718=ORIENTED_EDGE('',*,*,#13815,.T.);
#17719=ORIENTED_EDGE('',*,*,#13816,.T.);
#17720=ORIENTED_EDGE('',*,*,#13817,.T.);
#17721=ORIENTED_EDGE('',*,*,#13818,.T.);
#17722=ORIENTED_EDGE('',*,*,#13819,.T.);
#17723=ORIENTED_EDGE('',*,*,#13820,.T.);
#17724=ORIENTED_EDGE('',*,*,#13821,.T.);
#17725=ORIENTED_EDGE('',*,*,#13822,.T.);
#17726=ORIENTED_EDGE('',*,*,#13823,.T.);
#17727=ORIENTED_EDGE('',*,*,#13824,.T.);
#17728=ORIENTED_EDGE('',*,*,#13825,.T.);
#17729=ORIENTED_EDGE('',*,*,#13826,.T.);
#17730=ORIENTED_EDGE('',*,*,#13827,.T.);
#17731=ORIENTED_EDGE('',*,*,#13718,.F.);
#17732=ORIENTED_EDGE('',*,*,#13719,.F.);
#17733=ORIENTED_EDGE('',*,*,#13828,.T.);
#17734=ORIENTED_EDGE('',*,*,#13829,.T.);
#17735=ORIENTED_EDGE('',*,*,#13828,.F.);
#17736=ORIENTED_EDGE('',*,*,#13830,.F.);
#17737=ORIENTED_EDGE('',*,*,#13831,.F.);
#17738=ORIENTED_EDGE('',*,*,#13832,.T.);
#17739=ORIENTED_EDGE('',*,*,#13830,.T.);
#17740=ORIENTED_EDGE('',*,*,#13832,.F.);
#17741=ORIENTED_EDGE('',*,*,#13833,.F.);
#17742=ORIENTED_EDGE('',*,*,#13834,.T.);
#17743=ORIENTED_EDGE('',*,*,#13831,.T.);
#17744=ORIENTED_EDGE('',*,*,#13834,.F.);
#17745=ORIENTED_EDGE('',*,*,#13835,.F.);
#17746=ORIENTED_EDGE('',*,*,#13833,.T.);
#17747=ORIENTED_EDGE('',*,*,#13829,.F.);
#17748=ORIENTED_EDGE('',*,*,#13836,.T.);
#17749=ORIENTED_EDGE('',*,*,#13835,.T.);
#17750=ORIENTED_EDGE('',*,*,#13836,.F.);
#17751=ORIENTED_EDGE('',*,*,#13837,.F.);
#17752=ORIENTED_EDGE('',*,*,#13838,.T.);
#17753=ORIENTED_EDGE('',*,*,#13714,.T.);
#17754=ORIENTED_EDGE('',*,*,#13838,.F.);
#17755=ORIENTED_EDGE('',*,*,#13837,.T.);
#17756=ORIENTED_EDGE('',*,*,#13839,.F.);
#17757=ORIENTED_EDGE('',*,*,#13840,.F.);
#17758=ORIENTED_EDGE('',*,*,#13841,.T.);
#17759=ORIENTED_EDGE('',*,*,#13839,.T.);
#17760=ORIENTED_EDGE('',*,*,#13841,.F.);
#17761=ORIENTED_EDGE('',*,*,#13842,.F.);
#17762=ORIENTED_EDGE('',*,*,#13843,.T.);
#17763=ORIENTED_EDGE('',*,*,#13840,.T.);
#17764=ORIENTED_EDGE('',*,*,#13843,.F.);
#17765=ORIENTED_EDGE('',*,*,#13842,.T.);
#17766=ORIENTED_EDGE('',*,*,#13730,.F.);
#17767=ORIENTED_EDGE('',*,*,#13844,.F.);
#17768=ORIENTED_EDGE('',*,*,#13704,.F.);
#17769=ORIENTED_EDGE('',*,*,#13845,.F.);
#17770=ORIENTED_EDGE('',*,*,#13728,.F.);
#17771=ORIENTED_EDGE('',*,*,#13846,.T.);
#17772=ORIENTED_EDGE('',*,*,#13706,.F.);
#17773=ORIENTED_EDGE('',*,*,#13847,.T.);
#17774=ORIENTED_EDGE('',*,*,#13729,.F.);
#17775=ORIENTED_EDGE('',*,*,#13847,.F.);
#17776=ORIENTED_EDGE('',*,*,#13705,.F.);
#17777=ORIENTED_EDGE('',*,*,#13844,.T.);
#17778=ORIENTED_EDGE('',*,*,#13726,.F.);
#17779=ORIENTED_EDGE('',*,*,#13848,.F.);
#17780=ORIENTED_EDGE('',*,*,#13708,.F.);
#17781=ORIENTED_EDGE('',*,*,#13849,.T.);
#17782=ORIENTED_EDGE('',*,*,#13727,.F.);
#17783=ORIENTED_EDGE('',*,*,#13849,.F.);
#17784=ORIENTED_EDGE('',*,*,#13707,.F.);
#17785=ORIENTED_EDGE('',*,*,#13846,.F.);
#17786=ORIENTED_EDGE('',*,*,#13742,.F.);
#17787=ORIENTED_EDGE('',*,*,#13850,.F.);
#17788=ORIENTED_EDGE('',*,*,#13692,.F.);
#17789=ORIENTED_EDGE('',*,*,#13851,.F.);
#17790=ORIENTED_EDGE('',*,*,#13740,.F.);
#17791=ORIENTED_EDGE('',*,*,#13852,.T.);
#17792=ORIENTED_EDGE('',*,*,#13694,.F.);
#17793=ORIENTED_EDGE('',*,*,#13853,.T.);
#17794=ORIENTED_EDGE('',*,*,#13741,.F.);
#17795=ORIENTED_EDGE('',*,*,#13853,.F.);
#17796=ORIENTED_EDGE('',*,*,#13693,.F.);
#17797=ORIENTED_EDGE('',*,*,#13850,.T.);
#17798=ORIENTED_EDGE('',*,*,#13738,.F.);
#17799=ORIENTED_EDGE('',*,*,#13854,.F.);
#17800=ORIENTED_EDGE('',*,*,#13696,.F.);
#17801=ORIENTED_EDGE('',*,*,#13855,.T.);
#17802=ORIENTED_EDGE('',*,*,#13739,.F.);
#17803=ORIENTED_EDGE('',*,*,#13855,.F.);
#17804=ORIENTED_EDGE('',*,*,#13695,.F.);
#17805=ORIENTED_EDGE('',*,*,#13852,.F.);
#17806=ORIENTED_EDGE('',*,*,#13754,.F.);
#17807=ORIENTED_EDGE('',*,*,#13856,.F.);
#17808=ORIENTED_EDGE('',*,*,#13680,.F.);
#17809=ORIENTED_EDGE('',*,*,#13857,.F.);
#17810=ORIENTED_EDGE('',*,*,#13752,.F.);
#17811=ORIENTED_EDGE('',*,*,#13858,.T.);
#17812=ORIENTED_EDGE('',*,*,#13682,.F.);
#17813=ORIENTED_EDGE('',*,*,#13859,.T.);
#17814=ORIENTED_EDGE('',*,*,#13753,.F.);
#17815=ORIENTED_EDGE('',*,*,#13859,.F.);
#17816=ORIENTED_EDGE('',*,*,#13681,.F.);
#17817=ORIENTED_EDGE('',*,*,#13856,.T.);
#17818=ORIENTED_EDGE('',*,*,#13750,.F.);
#17819=ORIENTED_EDGE('',*,*,#13860,.F.);
#17820=ORIENTED_EDGE('',*,*,#13684,.F.);
#17821=ORIENTED_EDGE('',*,*,#13861,.T.);
#17822=ORIENTED_EDGE('',*,*,#13751,.F.);
#17823=ORIENTED_EDGE('',*,*,#13861,.F.);
#17824=ORIENTED_EDGE('',*,*,#13683,.F.);
#17825=ORIENTED_EDGE('',*,*,#13858,.F.);
#17826=ORIENTED_EDGE('',*,*,#13766,.F.);
#17827=ORIENTED_EDGE('',*,*,#13862,.F.);
#17828=ORIENTED_EDGE('',*,*,#13668,.F.);
#17829=ORIENTED_EDGE('',*,*,#13863,.F.);
#17830=ORIENTED_EDGE('',*,*,#13764,.F.);
#17831=ORIENTED_EDGE('',*,*,#13864,.T.);
#17832=ORIENTED_EDGE('',*,*,#13670,.F.);
#17833=ORIENTED_EDGE('',*,*,#13865,.T.);
#17834=ORIENTED_EDGE('',*,*,#13765,.F.);
#17835=ORIENTED_EDGE('',*,*,#13865,.F.);
#17836=ORIENTED_EDGE('',*,*,#13669,.F.);
#17837=ORIENTED_EDGE('',*,*,#13862,.T.);
#17838=ORIENTED_EDGE('',*,*,#13762,.F.);
#17839=ORIENTED_EDGE('',*,*,#13866,.F.);
#17840=ORIENTED_EDGE('',*,*,#13672,.F.);
#17841=ORIENTED_EDGE('',*,*,#13867,.T.);
#17842=ORIENTED_EDGE('',*,*,#13763,.F.);
#17843=ORIENTED_EDGE('',*,*,#13867,.F.);
#17844=ORIENTED_EDGE('',*,*,#13671,.F.);
#17845=ORIENTED_EDGE('',*,*,#13864,.F.);
#17846=ORIENTED_EDGE('',*,*,#13826,.F.);
#17847=ORIENTED_EDGE('',*,*,#13868,.F.);
#17848=ORIENTED_EDGE('',*,*,#13608,.F.);
#17849=ORIENTED_EDGE('',*,*,#13869,.F.);
#17850=ORIENTED_EDGE('',*,*,#13824,.F.);
#17851=ORIENTED_EDGE('',*,*,#13870,.T.);
#17852=ORIENTED_EDGE('',*,*,#13610,.F.);
#17853=ORIENTED_EDGE('',*,*,#13871,.T.);
#17854=ORIENTED_EDGE('',*,*,#13825,.F.);
#17855=ORIENTED_EDGE('',*,*,#13871,.F.);
#17856=ORIENTED_EDGE('',*,*,#13609,.F.);
#17857=ORIENTED_EDGE('',*,*,#13868,.T.);
#17858=ORIENTED_EDGE('',*,*,#13822,.F.);
#17859=ORIENTED_EDGE('',*,*,#13872,.F.);
#17860=ORIENTED_EDGE('',*,*,#13612,.F.);
#17861=ORIENTED_EDGE('',*,*,#13873,.T.);
#17862=ORIENTED_EDGE('',*,*,#13823,.F.);
#17863=ORIENTED_EDGE('',*,*,#13873,.F.);
#17864=ORIENTED_EDGE('',*,*,#13611,.F.);
#17865=ORIENTED_EDGE('',*,*,#13870,.F.);
#17866=ORIENTED_EDGE('',*,*,#13784,.F.);
#17867=ORIENTED_EDGE('',*,*,#13874,.F.);
#17868=ORIENTED_EDGE('',*,*,#13650,.F.);
#17869=ORIENTED_EDGE('',*,*,#13875,.F.);
#17870=ORIENTED_EDGE('',*,*,#13782,.F.);
#17871=ORIENTED_EDGE('',*,*,#13876,.T.);
#17872=ORIENTED_EDGE('',*,*,#13652,.F.);
#17873=ORIENTED_EDGE('',*,*,#13877,.T.);
#17874=ORIENTED_EDGE('',*,*,#13783,.F.);
#17875=ORIENTED_EDGE('',*,*,#13877,.F.);
#17876=ORIENTED_EDGE('',*,*,#13651,.F.);
#17877=ORIENTED_EDGE('',*,*,#13874,.T.);
#17878=ORIENTED_EDGE('',*,*,#13780,.F.);
#17879=ORIENTED_EDGE('',*,*,#13878,.F.);
#17880=ORIENTED_EDGE('',*,*,#13654,.F.);
#17881=ORIENTED_EDGE('',*,*,#13879,.T.);
#17882=ORIENTED_EDGE('',*,*,#13781,.F.);
#17883=ORIENTED_EDGE('',*,*,#13879,.F.);
#17884=ORIENTED_EDGE('',*,*,#13653,.F.);
#17885=ORIENTED_EDGE('',*,*,#13876,.F.);
#17886=ORIENTED_EDGE('',*,*,#13796,.F.);
#17887=ORIENTED_EDGE('',*,*,#13880,.F.);
#17888=ORIENTED_EDGE('',*,*,#13638,.F.);
#17889=ORIENTED_EDGE('',*,*,#13881,.F.);
#17890=ORIENTED_EDGE('',*,*,#13794,.F.);
#17891=ORIENTED_EDGE('',*,*,#13882,.T.);
#17892=ORIENTED_EDGE('',*,*,#13640,.F.);
#17893=ORIENTED_EDGE('',*,*,#13883,.T.);
#17894=ORIENTED_EDGE('',*,*,#13795,.F.);
#17895=ORIENTED_EDGE('',*,*,#13883,.F.);
#17896=ORIENTED_EDGE('',*,*,#13639,.F.);
#17897=ORIENTED_EDGE('',*,*,#13880,.T.);
#17898=ORIENTED_EDGE('',*,*,#13792,.F.);
#17899=ORIENTED_EDGE('',*,*,#13884,.F.);
#17900=ORIENTED_EDGE('',*,*,#13642,.F.);
#17901=ORIENTED_EDGE('',*,*,#13885,.T.);
#17902=ORIENTED_EDGE('',*,*,#13793,.F.);
#17903=ORIENTED_EDGE('',*,*,#13885,.F.);
#17904=ORIENTED_EDGE('',*,*,#13641,.F.);
#17905=ORIENTED_EDGE('',*,*,#13882,.F.);
#17906=ORIENTED_EDGE('',*,*,#13808,.F.);
#17907=ORIENTED_EDGE('',*,*,#13886,.F.);
#17908=ORIENTED_EDGE('',*,*,#13626,.F.);
#17909=ORIENTED_EDGE('',*,*,#13887,.F.);
#17910=ORIENTED_EDGE('',*,*,#13806,.F.);
#17911=ORIENTED_EDGE('',*,*,#13888,.T.);
#17912=ORIENTED_EDGE('',*,*,#13628,.F.);
#17913=ORIENTED_EDGE('',*,*,#13889,.T.);
#17914=ORIENTED_EDGE('',*,*,#13807,.F.);
#17915=ORIENTED_EDGE('',*,*,#13889,.F.);
#17916=ORIENTED_EDGE('',*,*,#13627,.F.);
#17917=ORIENTED_EDGE('',*,*,#13886,.T.);
#17918=ORIENTED_EDGE('',*,*,#13804,.F.);
#17919=ORIENTED_EDGE('',*,*,#13890,.F.);
#17920=ORIENTED_EDGE('',*,*,#13630,.F.);
#17921=ORIENTED_EDGE('',*,*,#13891,.T.);
#17922=ORIENTED_EDGE('',*,*,#13805,.F.);
#17923=ORIENTED_EDGE('',*,*,#13891,.F.);
#17924=ORIENTED_EDGE('',*,*,#13629,.F.);
#17925=ORIENTED_EDGE('',*,*,#13888,.F.);
#17926=ORIENTED_EDGE('',*,*,#13820,.F.);
#17927=ORIENTED_EDGE('',*,*,#13892,.F.);
#17928=ORIENTED_EDGE('',*,*,#13614,.F.);
#17929=ORIENTED_EDGE('',*,*,#13893,.F.);
#17930=ORIENTED_EDGE('',*,*,#13818,.F.);
#17931=ORIENTED_EDGE('',*,*,#13894,.T.);
#17932=ORIENTED_EDGE('',*,*,#13616,.F.);
#17933=ORIENTED_EDGE('',*,*,#13895,.T.);
#17934=ORIENTED_EDGE('',*,*,#13819,.F.);
#17935=ORIENTED_EDGE('',*,*,#13895,.F.);
#17936=ORIENTED_EDGE('',*,*,#13615,.F.);
#17937=ORIENTED_EDGE('',*,*,#13892,.T.);
#17938=ORIENTED_EDGE('',*,*,#13816,.F.);
#17939=ORIENTED_EDGE('',*,*,#13896,.F.);
#17940=ORIENTED_EDGE('',*,*,#13618,.F.);
#17941=ORIENTED_EDGE('',*,*,#13897,.T.);
#17942=ORIENTED_EDGE('',*,*,#13817,.F.);
#17943=ORIENTED_EDGE('',*,*,#13897,.F.);
#17944=ORIENTED_EDGE('',*,*,#13617,.F.);
#17945=ORIENTED_EDGE('',*,*,#13894,.F.);
#17946=ORIENTED_EDGE('',*,*,#13814,.F.);
#17947=ORIENTED_EDGE('',*,*,#13898,.F.);
#17948=ORIENTED_EDGE('',*,*,#13620,.F.);
#17949=ORIENTED_EDGE('',*,*,#13899,.F.);
#17950=ORIENTED_EDGE('',*,*,#13812,.F.);
#17951=ORIENTED_EDGE('',*,*,#13900,.T.);
#17952=ORIENTED_EDGE('',*,*,#13622,.F.);
#17953=ORIENTED_EDGE('',*,*,#13901,.T.);
#17954=ORIENTED_EDGE('',*,*,#13813,.F.);
#17955=ORIENTED_EDGE('',*,*,#13901,.F.);
#17956=ORIENTED_EDGE('',*,*,#13621,.F.);
#17957=ORIENTED_EDGE('',*,*,#13898,.T.);
#17958=ORIENTED_EDGE('',*,*,#13810,.F.);
#17959=ORIENTED_EDGE('',*,*,#13902,.F.);
#17960=ORIENTED_EDGE('',*,*,#13624,.F.);
#17961=ORIENTED_EDGE('',*,*,#13903,.T.);
#17962=ORIENTED_EDGE('',*,*,#13811,.F.);
#17963=ORIENTED_EDGE('',*,*,#13903,.F.);
#17964=ORIENTED_EDGE('',*,*,#13623,.F.);
#17965=ORIENTED_EDGE('',*,*,#13900,.F.);
#17966=ORIENTED_EDGE('',*,*,#13802,.F.);
#17967=ORIENTED_EDGE('',*,*,#13904,.F.);
#17968=ORIENTED_EDGE('',*,*,#13632,.F.);
#17969=ORIENTED_EDGE('',*,*,#13905,.F.);
#17970=ORIENTED_EDGE('',*,*,#13800,.F.);
#17971=ORIENTED_EDGE('',*,*,#13906,.T.);
#17972=ORIENTED_EDGE('',*,*,#13634,.F.);
#17973=ORIENTED_EDGE('',*,*,#13907,.T.);
#17974=ORIENTED_EDGE('',*,*,#13801,.F.);
#17975=ORIENTED_EDGE('',*,*,#13907,.F.);
#17976=ORIENTED_EDGE('',*,*,#13633,.F.);
#17977=ORIENTED_EDGE('',*,*,#13904,.T.);
#17978=ORIENTED_EDGE('',*,*,#13798,.F.);
#17979=ORIENTED_EDGE('',*,*,#13908,.F.);
#17980=ORIENTED_EDGE('',*,*,#13636,.F.);
#17981=ORIENTED_EDGE('',*,*,#13909,.T.);
#17982=ORIENTED_EDGE('',*,*,#13799,.F.);
#17983=ORIENTED_EDGE('',*,*,#13909,.F.);
#17984=ORIENTED_EDGE('',*,*,#13635,.F.);
#17985=ORIENTED_EDGE('',*,*,#13906,.F.);
#17986=ORIENTED_EDGE('',*,*,#13790,.F.);
#17987=ORIENTED_EDGE('',*,*,#13910,.F.);
#17988=ORIENTED_EDGE('',*,*,#13644,.F.);
#17989=ORIENTED_EDGE('',*,*,#13911,.F.);
#17990=ORIENTED_EDGE('',*,*,#13788,.F.);
#17991=ORIENTED_EDGE('',*,*,#13912,.T.);
#17992=ORIENTED_EDGE('',*,*,#13646,.F.);
#17993=ORIENTED_EDGE('',*,*,#13913,.T.);
#17994=ORIENTED_EDGE('',*,*,#13789,.F.);
#17995=ORIENTED_EDGE('',*,*,#13913,.F.);
#17996=ORIENTED_EDGE('',*,*,#13645,.F.);
#17997=ORIENTED_EDGE('',*,*,#13910,.T.);
#17998=ORIENTED_EDGE('',*,*,#13786,.F.);
#17999=ORIENTED_EDGE('',*,*,#13914,.F.);
#18000=ORIENTED_EDGE('',*,*,#13648,.F.);
#18001=ORIENTED_EDGE('',*,*,#13915,.T.);
#18002=ORIENTED_EDGE('',*,*,#13787,.F.);
#18003=ORIENTED_EDGE('',*,*,#13915,.F.);
#18004=ORIENTED_EDGE('',*,*,#13647,.F.);
#18005=ORIENTED_EDGE('',*,*,#13912,.F.);
#18006=ORIENTED_EDGE('',*,*,#13778,.F.);
#18007=ORIENTED_EDGE('',*,*,#13916,.F.);
#18008=ORIENTED_EDGE('',*,*,#13656,.F.);
#18009=ORIENTED_EDGE('',*,*,#13917,.F.);
#18010=ORIENTED_EDGE('',*,*,#13776,.F.);
#18011=ORIENTED_EDGE('',*,*,#13918,.T.);
#18012=ORIENTED_EDGE('',*,*,#13658,.F.);
#18013=ORIENTED_EDGE('',*,*,#13919,.T.);
#18014=ORIENTED_EDGE('',*,*,#13777,.F.);
#18015=ORIENTED_EDGE('',*,*,#13919,.F.);
#18016=ORIENTED_EDGE('',*,*,#13657,.F.);
#18017=ORIENTED_EDGE('',*,*,#13916,.T.);
#18018=ORIENTED_EDGE('',*,*,#13774,.F.);
#18019=ORIENTED_EDGE('',*,*,#13920,.F.);
#18020=ORIENTED_EDGE('',*,*,#13660,.F.);
#18021=ORIENTED_EDGE('',*,*,#13921,.T.);
#18022=ORIENTED_EDGE('',*,*,#13775,.F.);
#18023=ORIENTED_EDGE('',*,*,#13921,.F.);
#18024=ORIENTED_EDGE('',*,*,#13659,.F.);
#18025=ORIENTED_EDGE('',*,*,#13918,.F.);
#18026=ORIENTED_EDGE('',*,*,#13772,.F.);
#18027=ORIENTED_EDGE('',*,*,#13922,.F.);
#18028=ORIENTED_EDGE('',*,*,#13662,.F.);
#18029=ORIENTED_EDGE('',*,*,#13923,.F.);
#18030=ORIENTED_EDGE('',*,*,#13770,.F.);
#18031=ORIENTED_EDGE('',*,*,#13924,.T.);
#18032=ORIENTED_EDGE('',*,*,#13664,.F.);
#18033=ORIENTED_EDGE('',*,*,#13925,.T.);
#18034=ORIENTED_EDGE('',*,*,#13771,.F.);
#18035=ORIENTED_EDGE('',*,*,#13925,.F.);
#18036=ORIENTED_EDGE('',*,*,#13663,.F.);
#18037=ORIENTED_EDGE('',*,*,#13922,.T.);
#18038=ORIENTED_EDGE('',*,*,#13768,.F.);
#18039=ORIENTED_EDGE('',*,*,#13926,.F.);
#18040=ORIENTED_EDGE('',*,*,#13666,.F.);
#18041=ORIENTED_EDGE('',*,*,#13927,.T.);
#18042=ORIENTED_EDGE('',*,*,#13769,.F.);
#18043=ORIENTED_EDGE('',*,*,#13927,.F.);
#18044=ORIENTED_EDGE('',*,*,#13665,.F.);
#18045=ORIENTED_EDGE('',*,*,#13924,.F.);
#18046=ORIENTED_EDGE('',*,*,#13760,.F.);
#18047=ORIENTED_EDGE('',*,*,#13928,.F.);
#18048=ORIENTED_EDGE('',*,*,#13674,.F.);
#18049=ORIENTED_EDGE('',*,*,#13929,.F.);
#18050=ORIENTED_EDGE('',*,*,#13758,.F.);
#18051=ORIENTED_EDGE('',*,*,#13930,.T.);
#18052=ORIENTED_EDGE('',*,*,#13676,.F.);
#18053=ORIENTED_EDGE('',*,*,#13931,.T.);
#18054=ORIENTED_EDGE('',*,*,#13759,.F.);
#18055=ORIENTED_EDGE('',*,*,#13931,.F.);
#18056=ORIENTED_EDGE('',*,*,#13675,.F.);
#18057=ORIENTED_EDGE('',*,*,#13928,.T.);
#18058=ORIENTED_EDGE('',*,*,#13756,.F.);
#18059=ORIENTED_EDGE('',*,*,#13932,.F.);
#18060=ORIENTED_EDGE('',*,*,#13678,.F.);
#18061=ORIENTED_EDGE('',*,*,#13933,.T.);
#18062=ORIENTED_EDGE('',*,*,#13757,.F.);
#18063=ORIENTED_EDGE('',*,*,#13933,.F.);
#18064=ORIENTED_EDGE('',*,*,#13677,.F.);
#18065=ORIENTED_EDGE('',*,*,#13930,.F.);
#18066=ORIENTED_EDGE('',*,*,#13748,.F.);
#18067=ORIENTED_EDGE('',*,*,#13934,.F.);
#18068=ORIENTED_EDGE('',*,*,#13686,.F.);
#18069=ORIENTED_EDGE('',*,*,#13935,.F.);
#18070=ORIENTED_EDGE('',*,*,#13746,.F.);
#18071=ORIENTED_EDGE('',*,*,#13936,.T.);
#18072=ORIENTED_EDGE('',*,*,#13688,.F.);
#18073=ORIENTED_EDGE('',*,*,#13937,.T.);
#18074=ORIENTED_EDGE('',*,*,#13747,.F.);
#18075=ORIENTED_EDGE('',*,*,#13937,.F.);
#18076=ORIENTED_EDGE('',*,*,#13687,.F.);
#18077=ORIENTED_EDGE('',*,*,#13934,.T.);
#18078=ORIENTED_EDGE('',*,*,#13744,.F.);
#18079=ORIENTED_EDGE('',*,*,#13938,.F.);
#18080=ORIENTED_EDGE('',*,*,#13690,.F.);
#18081=ORIENTED_EDGE('',*,*,#13939,.T.);
#18082=ORIENTED_EDGE('',*,*,#13745,.F.);
#18083=ORIENTED_EDGE('',*,*,#13939,.F.);
#18084=ORIENTED_EDGE('',*,*,#13689,.F.);
#18085=ORIENTED_EDGE('',*,*,#13936,.F.);
#18086=ORIENTED_EDGE('',*,*,#13736,.F.);
#18087=ORIENTED_EDGE('',*,*,#13940,.F.);
#18088=ORIENTED_EDGE('',*,*,#13698,.F.);
#18089=ORIENTED_EDGE('',*,*,#13941,.F.);
#18090=ORIENTED_EDGE('',*,*,#13734,.F.);
#18091=ORIENTED_EDGE('',*,*,#13942,.T.);
#18092=ORIENTED_EDGE('',*,*,#13700,.F.);
#18093=ORIENTED_EDGE('',*,*,#13943,.T.);
#18094=ORIENTED_EDGE('',*,*,#13735,.F.);
#18095=ORIENTED_EDGE('',*,*,#13943,.F.);
#18096=ORIENTED_EDGE('',*,*,#13699,.F.);
#18097=ORIENTED_EDGE('',*,*,#13940,.T.);
#18098=ORIENTED_EDGE('',*,*,#13732,.F.);
#18099=ORIENTED_EDGE('',*,*,#13944,.F.);
#18100=ORIENTED_EDGE('',*,*,#13702,.F.);
#18101=ORIENTED_EDGE('',*,*,#13945,.T.);
#18102=ORIENTED_EDGE('',*,*,#13733,.F.);
#18103=ORIENTED_EDGE('',*,*,#13945,.F.);
#18104=ORIENTED_EDGE('',*,*,#13701,.F.);
#18105=ORIENTED_EDGE('',*,*,#13942,.F.);
#18106=ORIENTED_EDGE('',*,*,#13724,.F.);
#18107=ORIENTED_EDGE('',*,*,#13946,.F.);
#18108=ORIENTED_EDGE('',*,*,#13710,.F.);
#18109=ORIENTED_EDGE('',*,*,#13947,.F.);
#18110=ORIENTED_EDGE('',*,*,#13722,.F.);
#18111=ORIENTED_EDGE('',*,*,#13948,.T.);
#18112=ORIENTED_EDGE('',*,*,#13712,.F.);
#18113=ORIENTED_EDGE('',*,*,#13949,.T.);
#18114=ORIENTED_EDGE('',*,*,#13723,.F.);
#18115=ORIENTED_EDGE('',*,*,#13949,.F.);
#18116=ORIENTED_EDGE('',*,*,#13711,.F.);
#18117=ORIENTED_EDGE('',*,*,#13946,.T.);
#18118=ORIENTED_EDGE('',*,*,#13720,.F.);
#18119=ORIENTED_EDGE('',*,*,#13950,.F.);
#18120=ORIENTED_EDGE('',*,*,#13606,.F.);
#18121=ORIENTED_EDGE('',*,*,#13951,.T.);
#18122=ORIENTED_EDGE('',*,*,#13721,.F.);
#18123=ORIENTED_EDGE('',*,*,#13951,.F.);
#18124=ORIENTED_EDGE('',*,*,#13713,.F.);
#18125=ORIENTED_EDGE('',*,*,#13948,.F.);
#18126=ORIENTED_EDGE('',*,*,#13920,.T.);
#18127=ORIENTED_EDGE('',*,*,#13773,.F.);
#18128=ORIENTED_EDGE('',*,*,#13923,.T.);
#18129=ORIENTED_EDGE('',*,*,#13661,.F.);
#18130=ORIENTED_EDGE('',*,*,#13896,.T.);
#18131=ORIENTED_EDGE('',*,*,#13815,.F.);
#18132=ORIENTED_EDGE('',*,*,#13899,.T.);
#18133=ORIENTED_EDGE('',*,*,#13619,.F.);
#18134=ORIENTED_EDGE('',*,*,#13890,.T.);
#18135=ORIENTED_EDGE('',*,*,#13803,.F.);
#18136=ORIENTED_EDGE('',*,*,#13905,.T.);
#18137=ORIENTED_EDGE('',*,*,#13631,.F.);
#18138=ORIENTED_EDGE('',*,*,#13887,.T.);
#18139=ORIENTED_EDGE('',*,*,#13625,.F.);
#18140=ORIENTED_EDGE('',*,*,#13902,.T.);
#18141=ORIENTED_EDGE('',*,*,#13809,.F.);
#18142=ORIENTED_EDGE('',*,*,#13884,.T.);
#18143=ORIENTED_EDGE('',*,*,#13791,.F.);
#18144=ORIENTED_EDGE('',*,*,#13911,.T.);
#18145=ORIENTED_EDGE('',*,*,#13643,.F.);
#18146=ORIENTED_EDGE('',*,*,#13881,.T.);
#18147=ORIENTED_EDGE('',*,*,#13637,.F.);
#18148=ORIENTED_EDGE('',*,*,#13908,.T.);
#18149=ORIENTED_EDGE('',*,*,#13797,.F.);
#18150=ORIENTED_EDGE('',*,*,#13878,.T.);
#18151=ORIENTED_EDGE('',*,*,#13779,.F.);
#18152=ORIENTED_EDGE('',*,*,#13917,.T.);
#18153=ORIENTED_EDGE('',*,*,#13655,.F.);
#18154=ORIENTED_EDGE('',*,*,#13875,.T.);
#18155=ORIENTED_EDGE('',*,*,#13649,.F.);
#18156=ORIENTED_EDGE('',*,*,#13914,.T.);
#18157=ORIENTED_EDGE('',*,*,#13785,.F.);
#18158=ORIENTED_EDGE('',*,*,#13872,.T.);
#18159=ORIENTED_EDGE('',*,*,#13821,.F.);
#18160=ORIENTED_EDGE('',*,*,#13893,.T.);
#18161=ORIENTED_EDGE('',*,*,#13613,.F.);
#18162=ORIENTED_EDGE('',*,*,#13869,.T.);
#18163=ORIENTED_EDGE('',*,*,#13607,.F.);
#18164=ORIENTED_EDGE('',*,*,#13950,.T.);
#18165=ORIENTED_EDGE('',*,*,#13827,.F.);
#18166=ORIENTED_EDGE('',*,*,#13866,.T.);
#18167=ORIENTED_EDGE('',*,*,#13761,.F.);
#18168=ORIENTED_EDGE('',*,*,#13929,.T.);
#18169=ORIENTED_EDGE('',*,*,#13673,.F.);
#18170=ORIENTED_EDGE('',*,*,#13863,.T.);
#18171=ORIENTED_EDGE('',*,*,#13667,.F.);
#18172=ORIENTED_EDGE('',*,*,#13926,.T.);
#18173=ORIENTED_EDGE('',*,*,#13767,.F.);
#18174=ORIENTED_EDGE('',*,*,#13860,.T.);
#18175=ORIENTED_EDGE('',*,*,#13749,.F.);
#18176=ORIENTED_EDGE('',*,*,#13935,.T.);
#18177=ORIENTED_EDGE('',*,*,#13685,.F.);
#18178=ORIENTED_EDGE('',*,*,#13857,.T.);
#18179=ORIENTED_EDGE('',*,*,#13679,.F.);
#18180=ORIENTED_EDGE('',*,*,#13932,.T.);
#18181=ORIENTED_EDGE('',*,*,#13755,.F.);
#18182=ORIENTED_EDGE('',*,*,#13854,.T.);
#18183=ORIENTED_EDGE('',*,*,#13737,.F.);
#18184=ORIENTED_EDGE('',*,*,#13941,.T.);
#18185=ORIENTED_EDGE('',*,*,#13697,.F.);
#18186=ORIENTED_EDGE('',*,*,#13851,.T.);
#18187=ORIENTED_EDGE('',*,*,#13691,.F.);
#18188=ORIENTED_EDGE('',*,*,#13938,.T.);
#18189=ORIENTED_EDGE('',*,*,#13743,.F.);
#18190=ORIENTED_EDGE('',*,*,#13848,.T.);
#18191=ORIENTED_EDGE('',*,*,#13725,.F.);
#18192=ORIENTED_EDGE('',*,*,#13947,.T.);
#18193=ORIENTED_EDGE('',*,*,#13709,.F.);
#18194=ORIENTED_EDGE('',*,*,#13845,.T.);
#18195=ORIENTED_EDGE('',*,*,#13703,.F.);
#18196=ORIENTED_EDGE('',*,*,#13944,.T.);
#18197=ORIENTED_EDGE('',*,*,#13731,.F.);
#18198=ORIENTED_EDGE('',*,*,#13952,.F.);
#18199=ORIENTED_EDGE('',*,*,#13953,.T.);
#18200=ORIENTED_EDGE('',*,*,#13954,.T.);
#18201=ORIENTED_EDGE('',*,*,#13955,.T.);
#18202=ORIENTED_EDGE('',*,*,#13956,.F.);
#18203=ORIENTED_EDGE('',*,*,#13957,.T.);
#18204=ORIENTED_EDGE('',*,*,#13952,.T.);
#18205=ORIENTED_EDGE('',*,*,#13958,.T.);
#18206=ORIENTED_EDGE('',*,*,#13959,.F.);
#18207=ORIENTED_EDGE('',*,*,#13960,.T.);
#18208=ORIENTED_EDGE('',*,*,#13956,.T.);
#18209=ORIENTED_EDGE('',*,*,#13961,.T.);
#18210=ORIENTED_EDGE('',*,*,#13962,.F.);
#18211=ORIENTED_EDGE('',*,*,#13963,.T.);
#18212=ORIENTED_EDGE('',*,*,#13959,.T.);
#18213=ORIENTED_EDGE('',*,*,#13964,.T.);
#18214=ORIENTED_EDGE('',*,*,#13965,.F.);
#18215=ORIENTED_EDGE('',*,*,#13966,.T.);
#18216=ORIENTED_EDGE('',*,*,#13962,.T.);
#18217=ORIENTED_EDGE('',*,*,#13967,.T.);
#18218=ORIENTED_EDGE('',*,*,#13968,.F.);
#18219=ORIENTED_EDGE('',*,*,#13969,.T.);
#18220=ORIENTED_EDGE('',*,*,#13965,.T.);
#18221=ORIENTED_EDGE('',*,*,#13970,.T.);
#18222=ORIENTED_EDGE('',*,*,#13971,.F.);
#18223=ORIENTED_EDGE('',*,*,#13972,.T.);
#18224=ORIENTED_EDGE('',*,*,#13968,.T.);
#18225=ORIENTED_EDGE('',*,*,#13973,.T.);
#18226=ORIENTED_EDGE('',*,*,#13974,.F.);
#18227=ORIENTED_EDGE('',*,*,#13975,.T.);
#18228=ORIENTED_EDGE('',*,*,#13971,.T.);
#18229=ORIENTED_EDGE('',*,*,#13976,.T.);
#18230=ORIENTED_EDGE('',*,*,#13977,.F.);
#18231=ORIENTED_EDGE('',*,*,#13978,.T.);
#18232=ORIENTED_EDGE('',*,*,#13974,.T.);
#18233=ORIENTED_EDGE('',*,*,#13979,.T.);
#18234=ORIENTED_EDGE('',*,*,#13980,.F.);
#18235=ORIENTED_EDGE('',*,*,#13981,.T.);
#18236=ORIENTED_EDGE('',*,*,#13977,.T.);
#18237=ORIENTED_EDGE('',*,*,#13982,.T.);
#18238=ORIENTED_EDGE('',*,*,#13983,.F.);
#18239=ORIENTED_EDGE('',*,*,#13984,.T.);
#18240=ORIENTED_EDGE('',*,*,#13980,.T.);
#18241=ORIENTED_EDGE('',*,*,#13985,.T.);
#18242=ORIENTED_EDGE('',*,*,#13986,.F.);
#18243=ORIENTED_EDGE('',*,*,#13987,.T.);
#18244=ORIENTED_EDGE('',*,*,#13983,.T.);
#18245=ORIENTED_EDGE('',*,*,#13988,.T.);
#18246=ORIENTED_EDGE('',*,*,#13989,.F.);
#18247=ORIENTED_EDGE('',*,*,#13990,.T.);
#18248=ORIENTED_EDGE('',*,*,#13986,.T.);
#18249=ORIENTED_EDGE('',*,*,#13991,.T.);
#18250=ORIENTED_EDGE('',*,*,#13992,.F.);
#18251=ORIENTED_EDGE('',*,*,#13993,.T.);
#18252=ORIENTED_EDGE('',*,*,#13994,.F.);
#18253=ORIENTED_EDGE('',*,*,#13995,.F.);
#18254=ORIENTED_EDGE('',*,*,#13996,.T.);
#18255=ORIENTED_EDGE('',*,*,#13992,.T.);
#18256=ORIENTED_EDGE('',*,*,#13997,.F.);
#18257=ORIENTED_EDGE('',*,*,#13998,.F.);
#18258=ORIENTED_EDGE('',*,*,#13999,.F.);
#18259=ORIENTED_EDGE('',*,*,#14000,.T.);
#18260=ORIENTED_EDGE('',*,*,#13995,.T.);
#18261=ORIENTED_EDGE('',*,*,#14001,.F.);
#18262=ORIENTED_EDGE('',*,*,#14002,.F.);
#18263=ORIENTED_EDGE('',*,*,#14003,.T.);
#18264=ORIENTED_EDGE('',*,*,#13999,.T.);
#18265=ORIENTED_EDGE('',*,*,#14004,.F.);
#18266=ORIENTED_EDGE('',*,*,#14005,.F.);
#18267=ORIENTED_EDGE('',*,*,#14006,.T.);
#18268=ORIENTED_EDGE('',*,*,#14002,.T.);
#18269=ORIENTED_EDGE('',*,*,#14007,.F.);
#18270=ORIENTED_EDGE('',*,*,#14008,.F.);
#18271=ORIENTED_EDGE('',*,*,#14009,.T.);
#18272=ORIENTED_EDGE('',*,*,#14005,.T.);
#18273=ORIENTED_EDGE('',*,*,#14010,.F.);
#18274=ORIENTED_EDGE('',*,*,#14011,.F.);
#18275=ORIENTED_EDGE('',*,*,#14012,.T.);
#18276=ORIENTED_EDGE('',*,*,#14008,.T.);
#18277=ORIENTED_EDGE('',*,*,#14013,.F.);
#18278=ORIENTED_EDGE('',*,*,#14014,.F.);
#18279=ORIENTED_EDGE('',*,*,#14015,.T.);
#18280=ORIENTED_EDGE('',*,*,#14011,.T.);
#18281=ORIENTED_EDGE('',*,*,#14016,.F.);
#18282=ORIENTED_EDGE('',*,*,#14017,.F.);
#18283=ORIENTED_EDGE('',*,*,#14018,.T.);
#18284=ORIENTED_EDGE('',*,*,#14014,.T.);
#18285=ORIENTED_EDGE('',*,*,#14019,.F.);
#18286=ORIENTED_EDGE('',*,*,#14020,.F.);
#18287=ORIENTED_EDGE('',*,*,#14021,.T.);
#18288=ORIENTED_EDGE('',*,*,#14017,.T.);
#18289=ORIENTED_EDGE('',*,*,#14022,.F.);
#18290=ORIENTED_EDGE('',*,*,#14023,.F.);
#18291=ORIENTED_EDGE('',*,*,#14024,.T.);
#18292=ORIENTED_EDGE('',*,*,#14020,.T.);
#18293=ORIENTED_EDGE('',*,*,#14025,.F.);
#18294=ORIENTED_EDGE('',*,*,#14026,.F.);
#18295=ORIENTED_EDGE('',*,*,#14027,.T.);
#18296=ORIENTED_EDGE('',*,*,#14023,.T.);
#18297=ORIENTED_EDGE('',*,*,#14028,.F.);
#18298=ORIENTED_EDGE('',*,*,#14029,.F.);
#18299=ORIENTED_EDGE('',*,*,#14030,.T.);
#18300=ORIENTED_EDGE('',*,*,#14026,.T.);
#18301=ORIENTED_EDGE('',*,*,#14031,.F.);
#18302=ORIENTED_EDGE('',*,*,#13997,.T.);
#18303=ORIENTED_EDGE('',*,*,#13994,.T.);
#18304=ORIENTED_EDGE('',*,*,#14032,.T.);
#18305=ORIENTED_EDGE('',*,*,#14033,.F.);
#18306=ORIENTED_EDGE('',*,*,#14034,.F.);
#18307=ORIENTED_EDGE('',*,*,#14035,.T.);
#18308=ORIENTED_EDGE('',*,*,#14035,.F.);
#18309=ORIENTED_EDGE('',*,*,#14036,.F.);
#18310=ORIENTED_EDGE('',*,*,#13991,.F.);
#18311=ORIENTED_EDGE('',*,*,#13988,.F.);
#18312=ORIENTED_EDGE('',*,*,#13985,.F.);
#18313=ORIENTED_EDGE('',*,*,#13982,.F.);
#18314=ORIENTED_EDGE('',*,*,#13979,.F.);
#18315=ORIENTED_EDGE('',*,*,#13976,.F.);
#18316=ORIENTED_EDGE('',*,*,#13973,.F.);
#18317=ORIENTED_EDGE('',*,*,#13970,.F.);
#18318=ORIENTED_EDGE('',*,*,#13967,.F.);
#18319=ORIENTED_EDGE('',*,*,#13964,.F.);
#18320=ORIENTED_EDGE('',*,*,#13961,.F.);
#18321=ORIENTED_EDGE('',*,*,#13958,.F.);
#18322=ORIENTED_EDGE('',*,*,#13955,.F.);
#18323=ORIENTED_EDGE('',*,*,#14037,.F.);
#18324=ORIENTED_EDGE('',*,*,#14038,.T.);
#18325=ORIENTED_EDGE('',*,*,#14031,.T.);
#18326=ORIENTED_EDGE('',*,*,#14028,.T.);
#18327=ORIENTED_EDGE('',*,*,#14025,.T.);
#18328=ORIENTED_EDGE('',*,*,#14022,.T.);
#18329=ORIENTED_EDGE('',*,*,#14019,.T.);
#18330=ORIENTED_EDGE('',*,*,#14016,.T.);
#18331=ORIENTED_EDGE('',*,*,#14013,.T.);
#18332=ORIENTED_EDGE('',*,*,#14010,.T.);
#18333=ORIENTED_EDGE('',*,*,#14007,.T.);
#18334=ORIENTED_EDGE('',*,*,#14004,.T.);
#18335=ORIENTED_EDGE('',*,*,#14001,.T.);
#18336=ORIENTED_EDGE('',*,*,#13998,.T.);
#18337=ORIENTED_EDGE('',*,*,#14039,.T.);
#18338=ORIENTED_EDGE('',*,*,#14040,.T.);
#18339=ORIENTED_EDGE('',*,*,#14041,.T.);
#18340=ORIENTED_EDGE('',*,*,#14042,.T.);
#18341=ORIENTED_EDGE('',*,*,#14037,.T.);
#18342=ORIENTED_EDGE('',*,*,#14029,.T.);
#18343=ORIENTED_EDGE('',*,*,#14038,.F.);
#18344=ORIENTED_EDGE('',*,*,#14042,.F.);
#18345=ORIENTED_EDGE('',*,*,#14043,.T.);
#18346=ORIENTED_EDGE('',*,*,#14032,.F.);
#18347=ORIENTED_EDGE('',*,*,#13993,.F.);
#18348=ORIENTED_EDGE('',*,*,#13996,.F.);
#18349=ORIENTED_EDGE('',*,*,#14000,.F.);
#18350=ORIENTED_EDGE('',*,*,#14003,.F.);
#18351=ORIENTED_EDGE('',*,*,#14006,.F.);
#18352=ORIENTED_EDGE('',*,*,#14009,.F.);
#18353=ORIENTED_EDGE('',*,*,#14012,.F.);
#18354=ORIENTED_EDGE('',*,*,#14015,.F.);
#18355=ORIENTED_EDGE('',*,*,#14018,.F.);
#18356=ORIENTED_EDGE('',*,*,#14021,.F.);
#18357=ORIENTED_EDGE('',*,*,#14024,.F.);
#18358=ORIENTED_EDGE('',*,*,#14027,.F.);
#18359=ORIENTED_EDGE('',*,*,#14030,.F.);
#18360=ORIENTED_EDGE('',*,*,#14043,.F.);
#18361=ORIENTED_EDGE('',*,*,#14041,.F.);
#18362=ORIENTED_EDGE('',*,*,#13953,.F.);
#18363=ORIENTED_EDGE('',*,*,#13957,.F.);
#18364=ORIENTED_EDGE('',*,*,#13960,.F.);
#18365=ORIENTED_EDGE('',*,*,#13963,.F.);
#18366=ORIENTED_EDGE('',*,*,#13966,.F.);
#18367=ORIENTED_EDGE('',*,*,#13969,.F.);
#18368=ORIENTED_EDGE('',*,*,#13972,.F.);
#18369=ORIENTED_EDGE('',*,*,#13975,.F.);
#18370=ORIENTED_EDGE('',*,*,#13978,.F.);
#18371=ORIENTED_EDGE('',*,*,#13981,.F.);
#18372=ORIENTED_EDGE('',*,*,#13984,.F.);
#18373=ORIENTED_EDGE('',*,*,#13987,.F.);
#18374=ORIENTED_EDGE('',*,*,#13990,.F.);
#18375=ORIENTED_EDGE('',*,*,#14044,.F.);
#18376=ORIENTED_EDGE('',*,*,#13989,.T.);
#18377=ORIENTED_EDGE('',*,*,#14036,.T.);
#18378=ORIENTED_EDGE('',*,*,#14045,.F.);
#18379=ORIENTED_EDGE('',*,*,#14044,.T.);
#18380=ORIENTED_EDGE('',*,*,#14046,.F.);
#18381=ORIENTED_EDGE('',*,*,#14047,.F.);
#18382=ORIENTED_EDGE('',*,*,#14048,.T.);
#18383=ORIENTED_EDGE('',*,*,#14046,.T.);
#18384=ORIENTED_EDGE('',*,*,#14048,.F.);
#18385=ORIENTED_EDGE('',*,*,#14049,.F.);
#18386=ORIENTED_EDGE('',*,*,#14050,.T.);
#18387=ORIENTED_EDGE('',*,*,#14047,.T.);
#18388=ORIENTED_EDGE('',*,*,#14050,.F.);
#18389=ORIENTED_EDGE('',*,*,#14049,.T.);
#18390=ORIENTED_EDGE('',*,*,#14051,.F.);
#18391=ORIENTED_EDGE('',*,*,#14039,.F.);
#18392=ORIENTED_EDGE('',*,*,#13954,.F.);
#18393=ORIENTED_EDGE('',*,*,#14040,.F.);
#18394=ORIENTED_EDGE('',*,*,#14052,.T.);
#18395=ORIENTED_EDGE('',*,*,#14051,.T.);
#18396=ORIENTED_EDGE('',*,*,#14052,.F.);
#18397=ORIENTED_EDGE('',*,*,#14053,.F.);
#18398=ORIENTED_EDGE('',*,*,#14054,.T.);
#18399=ORIENTED_EDGE('',*,*,#14033,.T.);
#18400=ORIENTED_EDGE('',*,*,#14045,.T.);
#18401=ORIENTED_EDGE('',*,*,#14034,.T.);
#18402=ORIENTED_EDGE('',*,*,#14054,.F.);
#18403=ORIENTED_EDGE('',*,*,#14053,.T.);
#18404=ORIENTED_EDGE('',*,*,#14055,.T.);
#18405=ORIENTED_EDGE('',*,*,#14056,.T.);
#18406=ORIENTED_EDGE('',*,*,#14057,.T.);
#18407=ORIENTED_EDGE('',*,*,#14058,.T.);
#18408=ORIENTED_EDGE('',*,*,#14059,.T.);
#18409=ORIENTED_EDGE('',*,*,#14060,.T.);
#18410=ORIENTED_EDGE('',*,*,#14056,.F.);
#18411=ORIENTED_EDGE('',*,*,#14061,.F.);
#18412=ORIENTED_EDGE('',*,*,#14062,.F.);
#18413=ORIENTED_EDGE('',*,*,#14063,.F.);
#18414=ORIENTED_EDGE('',*,*,#14055,.F.);
#18415=ORIENTED_EDGE('',*,*,#14064,.F.);
#18416=ORIENTED_EDGE('',*,*,#14065,.F.);
#18417=ORIENTED_EDGE('',*,*,#14066,.F.);
#18418=ORIENTED_EDGE('',*,*,#14067,.F.);
#18419=ORIENTED_EDGE('',*,*,#14061,.T.);
#18420=ORIENTED_EDGE('',*,*,#14060,.F.);
#18421=ORIENTED_EDGE('',*,*,#14068,.T.);
#18422=ORIENTED_EDGE('',*,*,#14069,.T.);
#18423=ORIENTED_EDGE('',*,*,#14070,.T.);
#18424=ORIENTED_EDGE('',*,*,#14071,.F.);
#18425=ORIENTED_EDGE('',*,*,#14064,.T.);
#18426=ORIENTED_EDGE('',*,*,#14072,.T.);
#18427=ORIENTED_EDGE('',*,*,#14073,.T.);
#18428=ORIENTED_EDGE('',*,*,#14074,.T.);
#18429=ORIENTED_EDGE('',*,*,#14075,.T.);
#18430=ORIENTED_EDGE('',*,*,#14076,.T.);
#18431=ORIENTED_EDGE('',*,*,#14077,.T.);
#18432=ORIENTED_EDGE('',*,*,#14077,.F.);
#18433=ORIENTED_EDGE('',*,*,#14078,.T.);
#18434=ORIENTED_EDGE('',*,*,#14079,.T.);
#18435=ORIENTED_EDGE('',*,*,#14080,.T.);
#18436=ORIENTED_EDGE('',*,*,#14081,.T.);
#18437=ORIENTED_EDGE('',*,*,#14076,.F.);
#18438=ORIENTED_EDGE('',*,*,#14082,.F.);
#18439=ORIENTED_EDGE('',*,*,#14083,.T.);
#18440=ORIENTED_EDGE('',*,*,#14078,.F.);
#18441=ORIENTED_EDGE('',*,*,#14075,.F.);
#18442=ORIENTED_EDGE('',*,*,#14084,.T.);
#18443=ORIENTED_EDGE('',*,*,#14085,.F.);
#18444=ORIENTED_EDGE('',*,*,#14086,.T.);
#18445=ORIENTED_EDGE('',*,*,#14087,.F.);
#18446=ORIENTED_EDGE('',*,*,#14082,.T.);
#18447=ORIENTED_EDGE('',*,*,#14088,.T.);
#18448=ORIENTED_EDGE('',*,*,#14089,.T.);
#18449=ORIENTED_EDGE('',*,*,#14079,.F.);
#18450=ORIENTED_EDGE('',*,*,#14090,.T.);
#18451=ORIENTED_EDGE('',*,*,#14058,.F.);
#18452=ORIENTED_EDGE('',*,*,#14091,.T.);
#18453=ORIENTED_EDGE('',*,*,#14092,.T.);
#18454=ORIENTED_EDGE('',*,*,#14088,.F.);
#18455=ORIENTED_EDGE('',*,*,#14093,.T.);
#18456=ORIENTED_EDGE('',*,*,#14080,.F.);
#18457=ORIENTED_EDGE('',*,*,#14089,.F.);
#18458=ORIENTED_EDGE('',*,*,#14092,.F.);
#18459=ORIENTED_EDGE('',*,*,#14094,.F.);
#18460=ORIENTED_EDGE('',*,*,#14095,.F.);
#18461=ORIENTED_EDGE('',*,*,#14096,.F.);
#18462=ORIENTED_EDGE('',*,*,#14097,.F.);
#18463=ORIENTED_EDGE('',*,*,#14098,.F.);
#18464=ORIENTED_EDGE('',*,*,#14099,.F.);
#18465=ORIENTED_EDGE('',*,*,#14100,.F.);
#18466=ORIENTED_EDGE('',*,*,#14101,.F.);
#18467=ORIENTED_EDGE('',*,*,#14102,.F.);
#18468=ORIENTED_EDGE('',*,*,#14103,.F.);
#18469=ORIENTED_EDGE('',*,*,#14104,.F.);
#18470=ORIENTED_EDGE('',*,*,#14105,.F.);
#18471=ORIENTED_EDGE('',*,*,#14106,.F.);
#18472=ORIENTED_EDGE('',*,*,#14107,.F.);
#18473=ORIENTED_EDGE('',*,*,#14057,.F.);
#18474=ORIENTED_EDGE('',*,*,#14063,.T.);
#18475=ORIENTED_EDGE('',*,*,#14108,.F.);
#18476=ORIENTED_EDGE('',*,*,#14109,.F.);
#18477=ORIENTED_EDGE('',*,*,#14094,.T.);
#18478=ORIENTED_EDGE('',*,*,#14091,.F.);
#18479=ORIENTED_EDGE('',*,*,#14110,.T.);
#18480=ORIENTED_EDGE('',*,*,#14111,.T.);
#18481=ORIENTED_EDGE('',*,*,#14112,.T.);
#18482=ORIENTED_EDGE('',*,*,#14113,.T.);
#18483=ORIENTED_EDGE('',*,*,#14114,.T.);
#18484=ORIENTED_EDGE('',*,*,#14115,.T.);
#18485=ORIENTED_EDGE('',*,*,#14115,.F.);
#18486=ORIENTED_EDGE('',*,*,#14116,.T.);
#18487=ORIENTED_EDGE('',*,*,#14117,.T.);
#18488=ORIENTED_EDGE('',*,*,#14118,.T.);
#18489=ORIENTED_EDGE('',*,*,#14119,.F.);
#18490=ORIENTED_EDGE('',*,*,#14120,.T.);
#18491=ORIENTED_EDGE('',*,*,#14114,.F.);
#18492=ORIENTED_EDGE('',*,*,#14121,.F.);
#18493=ORIENTED_EDGE('',*,*,#14122,.F.);
#18494=ORIENTED_EDGE('',*,*,#14116,.F.);
#18495=ORIENTED_EDGE('',*,*,#14113,.F.);
#18496=ORIENTED_EDGE('',*,*,#14123,.T.);
#18497=ORIENTED_EDGE('',*,*,#14097,.T.);
#18498=ORIENTED_EDGE('',*,*,#14124,.F.);
#18499=ORIENTED_EDGE('',*,*,#14121,.T.);
#18500=ORIENTED_EDGE('',*,*,#14108,.T.);
#18501=ORIENTED_EDGE('',*,*,#14062,.T.);
#18502=ORIENTED_EDGE('',*,*,#14067,.T.);
#18503=ORIENTED_EDGE('',*,*,#14125,.T.);
#18504=ORIENTED_EDGE('',*,*,#14126,.T.);
#18505=ORIENTED_EDGE('',*,*,#14127,.T.);
#18506=ORIENTED_EDGE('',*,*,#14127,.F.);
#18507=ORIENTED_EDGE('',*,*,#14128,.T.);
#18508=ORIENTED_EDGE('',*,*,#14129,.T.);
#18509=ORIENTED_EDGE('',*,*,#14095,.T.);
#18510=ORIENTED_EDGE('',*,*,#14109,.T.);
#18511=ORIENTED_EDGE('',*,*,#14124,.T.);
#18512=ORIENTED_EDGE('',*,*,#14096,.T.);
#18513=ORIENTED_EDGE('',*,*,#14129,.F.);
#18514=ORIENTED_EDGE('',*,*,#14130,.T.);
#18515=ORIENTED_EDGE('',*,*,#14112,.F.);
#18516=ORIENTED_EDGE('',*,*,#14131,.T.);
#18517=ORIENTED_EDGE('',*,*,#14132,.F.);
#18518=ORIENTED_EDGE('',*,*,#14133,.F.);
#18519=ORIENTED_EDGE('',*,*,#14098,.T.);
#18520=ORIENTED_EDGE('',*,*,#14123,.F.);
#18521=ORIENTED_EDGE('',*,*,#14130,.F.);
#18522=ORIENTED_EDGE('',*,*,#14134,.F.);
#18523=ORIENTED_EDGE('',*,*,#14135,.F.);
#18524=ORIENTED_EDGE('',*,*,#14122,.T.);
#18525=ORIENTED_EDGE('',*,*,#14126,.F.);
#18526=ORIENTED_EDGE('',*,*,#14136,.F.);
#18527=ORIENTED_EDGE('',*,*,#14134,.T.);
#18528=ORIENTED_EDGE('',*,*,#14128,.F.);
#18529=ORIENTED_EDGE('',*,*,#14107,.T.);
#18530=ORIENTED_EDGE('',*,*,#14137,.T.);
#18531=ORIENTED_EDGE('',*,*,#14138,.T.);
#18532=ORIENTED_EDGE('',*,*,#14137,.F.);
#18533=ORIENTED_EDGE('',*,*,#14139,.F.);
#18534=ORIENTED_EDGE('',*,*,#14140,.T.);
#18535=ORIENTED_EDGE('',*,*,#14138,.F.);
#18536=ORIENTED_EDGE('',*,*,#14140,.F.);
#18537=ORIENTED_EDGE('',*,*,#14141,.T.);
#18538=ORIENTED_EDGE('',*,*,#14142,.T.);
#18539=ORIENTED_EDGE('',*,*,#14143,.T.);
#18540=ORIENTED_EDGE('',*,*,#14144,.T.);
#18541=ORIENTED_EDGE('',*,*,#14145,.T.);
#18542=ORIENTED_EDGE('',*,*,#14146,.T.);
#18543=ORIENTED_EDGE('',*,*,#14146,.F.);
#18544=ORIENTED_EDGE('',*,*,#14147,.T.);
#18545=ORIENTED_EDGE('',*,*,#14148,.T.);
#18546=ORIENTED_EDGE('',*,*,#14149,.T.);
#18547=ORIENTED_EDGE('',*,*,#14150,.F.);
#18548=ORIENTED_EDGE('',*,*,#14151,.T.);
#18549=ORIENTED_EDGE('',*,*,#14145,.F.);
#18550=ORIENTED_EDGE('',*,*,#14152,.F.);
#18551=ORIENTED_EDGE('',*,*,#14153,.F.);
#18552=ORIENTED_EDGE('',*,*,#14147,.F.);
#18553=ORIENTED_EDGE('',*,*,#14144,.F.);
#18554=ORIENTED_EDGE('',*,*,#14154,.T.);
#18555=ORIENTED_EDGE('',*,*,#14105,.T.);
#18556=ORIENTED_EDGE('',*,*,#14155,.F.);
#18557=ORIENTED_EDGE('',*,*,#14152,.T.);
#18558=ORIENTED_EDGE('',*,*,#14156,.T.);
#18559=ORIENTED_EDGE('',*,*,#14157,.T.);
#18560=ORIENTED_EDGE('',*,*,#14158,.T.);
#18561=ORIENTED_EDGE('',*,*,#14159,.T.);
#18562=ORIENTED_EDGE('',*,*,#14160,.T.);
#18563=ORIENTED_EDGE('',*,*,#14161,.T.);
#18564=ORIENTED_EDGE('',*,*,#14157,.F.);
#18565=ORIENTED_EDGE('',*,*,#14162,.F.);
#18566=ORIENTED_EDGE('',*,*,#14163,.F.);
#18567=ORIENTED_EDGE('',*,*,#14164,.F.);
#18568=ORIENTED_EDGE('',*,*,#14156,.F.);
#18569=ORIENTED_EDGE('',*,*,#14165,.F.);
#18570=ORIENTED_EDGE('',*,*,#14102,.T.);
#18571=ORIENTED_EDGE('',*,*,#14166,.F.);
#18572=ORIENTED_EDGE('',*,*,#14167,.F.);
#18573=ORIENTED_EDGE('',*,*,#14162,.T.);
#18574=ORIENTED_EDGE('',*,*,#14161,.F.);
#18575=ORIENTED_EDGE('',*,*,#14168,.T.);
#18576=ORIENTED_EDGE('',*,*,#14169,.T.);
#18577=ORIENTED_EDGE('',*,*,#14103,.T.);
#18578=ORIENTED_EDGE('',*,*,#14165,.T.);
#18579=ORIENTED_EDGE('',*,*,#14155,.T.);
#18580=ORIENTED_EDGE('',*,*,#14104,.T.);
#18581=ORIENTED_EDGE('',*,*,#14169,.F.);
#18582=ORIENTED_EDGE('',*,*,#14170,.T.);
#18583=ORIENTED_EDGE('',*,*,#14170,.F.);
#18584=ORIENTED_EDGE('',*,*,#14171,.F.);
#18585=ORIENTED_EDGE('',*,*,#14172,.F.);
#18586=ORIENTED_EDGE('',*,*,#14153,.T.);
#18587=ORIENTED_EDGE('',*,*,#14160,.F.);
#18588=ORIENTED_EDGE('',*,*,#14173,.F.);
#18589=ORIENTED_EDGE('',*,*,#14171,.T.);
#18590=ORIENTED_EDGE('',*,*,#14168,.F.);
#18591=ORIENTED_EDGE('',*,*,#14174,.T.);
#18592=ORIENTED_EDGE('',*,*,#14163,.T.);
#18593=ORIENTED_EDGE('',*,*,#14167,.T.);
#18594=ORIENTED_EDGE('',*,*,#14175,.T.);
#18595=ORIENTED_EDGE('',*,*,#14176,.T.);
#18596=ORIENTED_EDGE('',*,*,#14177,.T.);
#18597=ORIENTED_EDGE('',*,*,#14177,.F.);
#18598=ORIENTED_EDGE('',*,*,#14178,.T.);
#18599=ORIENTED_EDGE('',*,*,#14179,.T.);
#18600=ORIENTED_EDGE('',*,*,#14180,.T.);
#18601=ORIENTED_EDGE('',*,*,#14181,.F.);
#18602=ORIENTED_EDGE('',*,*,#14182,.T.);
#18603=ORIENTED_EDGE('',*,*,#14176,.F.);
#18604=ORIENTED_EDGE('',*,*,#14183,.F.);
#18605=ORIENTED_EDGE('',*,*,#14184,.F.);
#18606=ORIENTED_EDGE('',*,*,#14178,.F.);
#18607=ORIENTED_EDGE('',*,*,#14175,.F.);
#18608=ORIENTED_EDGE('',*,*,#14166,.T.);
#18609=ORIENTED_EDGE('',*,*,#14101,.T.);
#18610=ORIENTED_EDGE('',*,*,#14185,.F.);
#18611=ORIENTED_EDGE('',*,*,#14183,.T.);
#18612=ORIENTED_EDGE('',*,*,#14132,.T.);
#18613=ORIENTED_EDGE('',*,*,#14186,.T.);
#18614=ORIENTED_EDGE('',*,*,#14187,.T.);
#18615=ORIENTED_EDGE('',*,*,#14188,.T.);
#18616=ORIENTED_EDGE('',*,*,#14189,.T.);
#18617=ORIENTED_EDGE('',*,*,#14190,.T.);
#18618=ORIENTED_EDGE('',*,*,#14111,.F.);
#18619=ORIENTED_EDGE('',*,*,#14191,.F.);
#18620=ORIENTED_EDGE('',*,*,#14186,.F.);
#18621=ORIENTED_EDGE('',*,*,#14131,.F.);
#18622=ORIENTED_EDGE('',*,*,#14190,.F.);
#18623=ORIENTED_EDGE('',*,*,#14192,.T.);
#18624=ORIENTED_EDGE('',*,*,#14193,.T.);
#18625=ORIENTED_EDGE('',*,*,#14099,.T.);
#18626=ORIENTED_EDGE('',*,*,#14133,.T.);
#18627=ORIENTED_EDGE('',*,*,#14185,.T.);
#18628=ORIENTED_EDGE('',*,*,#14100,.T.);
#18629=ORIENTED_EDGE('',*,*,#14193,.F.);
#18630=ORIENTED_EDGE('',*,*,#14194,.T.);
#18631=ORIENTED_EDGE('',*,*,#14194,.F.);
#18632=ORIENTED_EDGE('',*,*,#14195,.F.);
#18633=ORIENTED_EDGE('',*,*,#14196,.F.);
#18634=ORIENTED_EDGE('',*,*,#14184,.T.);
#18635=ORIENTED_EDGE('',*,*,#14189,.F.);
#18636=ORIENTED_EDGE('',*,*,#14197,.F.);
#18637=ORIENTED_EDGE('',*,*,#14195,.T.);
#18638=ORIENTED_EDGE('',*,*,#14192,.F.);
#18639=ORIENTED_EDGE('',*,*,#14198,.T.);
#18640=ORIENTED_EDGE('',*,*,#14085,.T.);
#18641=ORIENTED_EDGE('',*,*,#14199,.T.);
#18642=ORIENTED_EDGE('',*,*,#14150,.T.);
#18643=ORIENTED_EDGE('',*,*,#14200,.T.);
#18644=ORIENTED_EDGE('',*,*,#14181,.T.);
#18645=ORIENTED_EDGE('',*,*,#14201,.T.);
#18646=ORIENTED_EDGE('',*,*,#14202,.T.);
#18647=ORIENTED_EDGE('',*,*,#14203,.T.);
#18648=ORIENTED_EDGE('',*,*,#14204,.T.);
#18649=ORIENTED_EDGE('',*,*,#14065,.T.);
#18650=ORIENTED_EDGE('',*,*,#14071,.T.);
#18651=ORIENTED_EDGE('',*,*,#14205,.T.);
#18652=ORIENTED_EDGE('',*,*,#14119,.T.);
#18653=ORIENTED_EDGE('',*,*,#14206,.T.);
#18654=ORIENTED_EDGE('',*,*,#14207,.T.);
#18655=ORIENTED_EDGE('',*,*,#14208,.T.);
#18656=ORIENTED_EDGE('',*,*,#14209,.T.);
#18657=ORIENTED_EDGE('',*,*,#14117,.F.);
#18658=ORIENTED_EDGE('',*,*,#14135,.T.);
#18659=ORIENTED_EDGE('',*,*,#14125,.F.);
#18660=ORIENTED_EDGE('',*,*,#14066,.T.);
#18661=ORIENTED_EDGE('',*,*,#14204,.F.);
#18662=ORIENTED_EDGE('',*,*,#14210,.T.);
#18663=ORIENTED_EDGE('',*,*,#14208,.F.);
#18664=ORIENTED_EDGE('',*,*,#14136,.T.);
#18665=ORIENTED_EDGE('',*,*,#14211,.T.);
#18666=ORIENTED_EDGE('',*,*,#14212,.T.);
#18667=ORIENTED_EDGE('',*,*,#14179,.F.);
#18668=ORIENTED_EDGE('',*,*,#14196,.T.);
#18669=ORIENTED_EDGE('',*,*,#14188,.F.);
#18670=ORIENTED_EDGE('',*,*,#14213,.T.);
#18671=ORIENTED_EDGE('',*,*,#14207,.F.);
#18672=ORIENTED_EDGE('',*,*,#14214,.T.);
#18673=ORIENTED_EDGE('',*,*,#14211,.F.);
#18674=ORIENTED_EDGE('',*,*,#14197,.T.);
#18675=ORIENTED_EDGE('',*,*,#14087,.T.);
#18676=ORIENTED_EDGE('',*,*,#14215,.T.);
#18677=ORIENTED_EDGE('',*,*,#14069,.F.);
#18678=ORIENTED_EDGE('',*,*,#14216,.T.);
#18679=ORIENTED_EDGE('',*,*,#14217,.T.);
#18680=ORIENTED_EDGE('',*,*,#14218,.T.);
#18681=ORIENTED_EDGE('',*,*,#14148,.F.);
#18682=ORIENTED_EDGE('',*,*,#14172,.T.);
#18683=ORIENTED_EDGE('',*,*,#14159,.F.);
#18684=ORIENTED_EDGE('',*,*,#14219,.T.);
#18685=ORIENTED_EDGE('',*,*,#14202,.F.);
#18686=ORIENTED_EDGE('',*,*,#14220,.T.);
#18687=ORIENTED_EDGE('',*,*,#14217,.F.);
#18688=ORIENTED_EDGE('',*,*,#14173,.T.);
#18689=ORIENTED_EDGE('',*,*,#14110,.F.);
#18690=ORIENTED_EDGE('',*,*,#14120,.F.);
#18691=ORIENTED_EDGE('',*,*,#14205,.F.);
#18692=ORIENTED_EDGE('',*,*,#14213,.F.);
#18693=ORIENTED_EDGE('',*,*,#14187,.F.);
#18694=ORIENTED_EDGE('',*,*,#14191,.T.);
#18695=ORIENTED_EDGE('',*,*,#14158,.F.);
#18696=ORIENTED_EDGE('',*,*,#14164,.T.);
#18697=ORIENTED_EDGE('',*,*,#14174,.F.);
#18698=ORIENTED_EDGE('',*,*,#14182,.F.);
#18699=ORIENTED_EDGE('',*,*,#14200,.F.);
#18700=ORIENTED_EDGE('',*,*,#14219,.F.);
#18701=ORIENTED_EDGE('',*,*,#14206,.F.);
#18702=ORIENTED_EDGE('',*,*,#14118,.F.);
#18703=ORIENTED_EDGE('',*,*,#14209,.F.);
#18704=ORIENTED_EDGE('',*,*,#14210,.F.);
#18705=ORIENTED_EDGE('',*,*,#14203,.F.);
#18706=ORIENTED_EDGE('',*,*,#14070,.F.);
#18707=ORIENTED_EDGE('',*,*,#14215,.F.);
#18708=ORIENTED_EDGE('',*,*,#14086,.F.);
#18709=ORIENTED_EDGE('',*,*,#14198,.F.);
#18710=ORIENTED_EDGE('',*,*,#14149,.F.);
#18711=ORIENTED_EDGE('',*,*,#14218,.F.);
#18712=ORIENTED_EDGE('',*,*,#14220,.F.);
#18713=ORIENTED_EDGE('',*,*,#14201,.F.);
#18714=ORIENTED_EDGE('',*,*,#14180,.F.);
#18715=ORIENTED_EDGE('',*,*,#14212,.F.);
#18716=ORIENTED_EDGE('',*,*,#14214,.F.);
#18717=ORIENTED_EDGE('',*,*,#14221,.F.);
#18718=ORIENTED_EDGE('',*,*,#14221,.T.);
#18719=ORIENTED_EDGE('',*,*,#14222,.T.);
#18720=ORIENTED_EDGE('',*,*,#14139,.T.);
#18721=ORIENTED_EDGE('',*,*,#14222,.F.);
#18722=ORIENTED_EDGE('',*,*,#14090,.F.);
#18723=ORIENTED_EDGE('',*,*,#14083,.F.);
#18724=ORIENTED_EDGE('',*,*,#14216,.F.);
#18725=ORIENTED_EDGE('',*,*,#14223,.T.);
#18726=ORIENTED_EDGE('',*,*,#14059,.F.);
#18727=ORIENTED_EDGE('',*,*,#14093,.F.);
#18728=ORIENTED_EDGE('',*,*,#14223,.F.);
#18729=ORIENTED_EDGE('',*,*,#14068,.F.);
#18730=ORIENTED_EDGE('',*,*,#14074,.F.);
#18731=ORIENTED_EDGE('',*,*,#14224,.T.);
#18732=ORIENTED_EDGE('',*,*,#14141,.F.);
#18733=ORIENTED_EDGE('',*,*,#14151,.F.);
#18734=ORIENTED_EDGE('',*,*,#14199,.F.);
#18735=ORIENTED_EDGE('',*,*,#14084,.F.);
#18736=ORIENTED_EDGE('',*,*,#14073,.F.);
#18737=ORIENTED_EDGE('',*,*,#14225,.F.);
#18738=ORIENTED_EDGE('',*,*,#14142,.F.);
#18739=ORIENTED_EDGE('',*,*,#14224,.F.);
#18740=ORIENTED_EDGE('',*,*,#14072,.F.);
#18741=ORIENTED_EDGE('',*,*,#14081,.F.);
#18742=ORIENTED_EDGE('',*,*,#14106,.T.);
#18743=ORIENTED_EDGE('',*,*,#14154,.F.);
#18744=ORIENTED_EDGE('',*,*,#14143,.F.);
#18745=ORIENTED_EDGE('',*,*,#14225,.T.);
#18746=ORIENTED_EDGE('',*,*,#14226,.F.);
#18747=ORIENTED_EDGE('',*,*,#14227,.F.);
#18748=ORIENTED_EDGE('',*,*,#14228,.T.);
#18749=ORIENTED_EDGE('',*,*,#14226,.T.);
#18750=ORIENTED_EDGE('',*,*,#14228,.F.);
#18751=ORIENTED_EDGE('',*,*,#14229,.F.);
#18752=ORIENTED_EDGE('',*,*,#14230,.T.);
#18753=ORIENTED_EDGE('',*,*,#14227,.T.);
#18754=ORIENTED_EDGE('',*,*,#14230,.F.);
#18755=ORIENTED_EDGE('',*,*,#14231,.F.);
#18756=ORIENTED_EDGE('',*,*,#14232,.T.);
#18757=ORIENTED_EDGE('',*,*,#14229,.T.);
#18758=ORIENTED_EDGE('',*,*,#14232,.F.);
#18759=ORIENTED_EDGE('',*,*,#14231,.T.);
#18760=ORIENTED_EDGE('',*,*,#14233,.T.);
#18761=ORIENTED_EDGE('',*,*,#14234,.T.);
#18762=ORIENTED_EDGE('',*,*,#14233,.F.);
#18763=ORIENTED_EDGE('',*,*,#14235,.T.);
#18764=ORIENTED_EDGE('',*,*,#14236,.F.);
#18765=ORIENTED_EDGE('',*,*,#14237,.F.);
#18766=ORIENTED_EDGE('',*,*,#14238,.T.);
#18767=ORIENTED_EDGE('',*,*,#14234,.F.);
#18768=ORIENTED_EDGE('',*,*,#14238,.F.);
#18769=ORIENTED_EDGE('',*,*,#14239,.F.);
#18770=ORIENTED_EDGE('',*,*,#14240,.T.);
#18771=ORIENTED_EDGE('',*,*,#14241,.T.);
#18772=ORIENTED_EDGE('',*,*,#14242,.T.);
#18773=ORIENTED_EDGE('',*,*,#14243,.T.);
#18774=ORIENTED_EDGE('',*,*,#14242,.F.);
#18775=ORIENTED_EDGE('',*,*,#14244,.T.);
#18776=ORIENTED_EDGE('',*,*,#14245,.T.);
#18777=ORIENTED_EDGE('',*,*,#14240,.F.);
#18778=ORIENTED_EDGE('',*,*,#14246,.T.);
#18779=ORIENTED_EDGE('',*,*,#14247,.T.);
#18780=ORIENTED_EDGE('',*,*,#14248,.T.);
#18781=ORIENTED_EDGE('',*,*,#14249,.T.);
#18782=ORIENTED_EDGE('',*,*,#14250,.T.);
#18783=ORIENTED_EDGE('',*,*,#14235,.F.);
#18784=ORIENTED_EDGE('',*,*,#14251,.T.);
#18785=ORIENTED_EDGE('',*,*,#14236,.T.);
#18786=ORIENTED_EDGE('',*,*,#14237,.T.);
#18787=ORIENTED_EDGE('',*,*,#14251,.F.);
#18788=ORIENTED_EDGE('',*,*,#14252,.T.);
#18789=ORIENTED_EDGE('',*,*,#14253,.T.);
#18790=ORIENTED_EDGE('',*,*,#14254,.T.);
#18791=ORIENTED_EDGE('',*,*,#14255,.T.);
#18792=ORIENTED_EDGE('',*,*,#14256,.T.);
#18793=ORIENTED_EDGE('',*,*,#14257,.F.);
#18794=ORIENTED_EDGE('',*,*,#14256,.F.);
#18795=ORIENTED_EDGE('',*,*,#14254,.F.);
#18796=ORIENTED_EDGE('',*,*,#14253,.F.);
#18797=ORIENTED_EDGE('',*,*,#14252,.F.);
#18798=ORIENTED_EDGE('',*,*,#14258,.T.);
#18799=ORIENTED_EDGE('',*,*,#14259,.F.);
#18800=ORIENTED_EDGE('',*,*,#14260,.F.);
#18801=ORIENTED_EDGE('',*,*,#14261,.F.);
#18802=ORIENTED_EDGE('',*,*,#14262,.F.);
#18803=ORIENTED_EDGE('',*,*,#14263,.F.);
#18804=ORIENTED_EDGE('',*,*,#14264,.F.);
#18805=ORIENTED_EDGE('',*,*,#14265,.F.);
#18806=ORIENTED_EDGE('',*,*,#14266,.F.);
#18807=ORIENTED_EDGE('',*,*,#14267,.F.);
#18808=ORIENTED_EDGE('',*,*,#14268,.F.);
#18809=ORIENTED_EDGE('',*,*,#14269,.F.);
#18810=ORIENTED_EDGE('',*,*,#14270,.F.);
#18811=ORIENTED_EDGE('',*,*,#14271,.F.);
#18812=ORIENTED_EDGE('',*,*,#14258,.F.);
#18813=ORIENTED_EDGE('',*,*,#14271,.T.);
#18814=ORIENTED_EDGE('',*,*,#14272,.F.);
#18815=ORIENTED_EDGE('',*,*,#14273,.F.);
#18816=ORIENTED_EDGE('',*,*,#14269,.T.);
#18817=ORIENTED_EDGE('',*,*,#14274,.F.);
#18818=ORIENTED_EDGE('',*,*,#14275,.F.);
#18819=ORIENTED_EDGE('',*,*,#14267,.T.);
#18820=ORIENTED_EDGE('',*,*,#14276,.F.);
#18821=ORIENTED_EDGE('',*,*,#14277,.F.);
#18822=ORIENTED_EDGE('',*,*,#14265,.T.);
#18823=ORIENTED_EDGE('',*,*,#14278,.F.);
#18824=ORIENTED_EDGE('',*,*,#14279,.F.);
#18825=ORIENTED_EDGE('',*,*,#14263,.T.);
#18826=ORIENTED_EDGE('',*,*,#14280,.F.);
#18827=ORIENTED_EDGE('',*,*,#14281,.F.);
#18828=ORIENTED_EDGE('',*,*,#14261,.T.);
#18829=ORIENTED_EDGE('',*,*,#14282,.F.);
#18830=ORIENTED_EDGE('',*,*,#14283,.F.);
#18831=ORIENTED_EDGE('',*,*,#14259,.T.);
#18832=ORIENTED_EDGE('',*,*,#14250,.F.);
#18833=ORIENTED_EDGE('',*,*,#14284,.T.);
#18834=ORIENTED_EDGE('',*,*,#14277,.T.);
#18835=ORIENTED_EDGE('',*,*,#14276,.T.);
#18836=ORIENTED_EDGE('',*,*,#14266,.T.);
#18837=ORIENTED_EDGE('',*,*,#14284,.F.);
#18838=ORIENTED_EDGE('',*,*,#14249,.F.);
#18839=ORIENTED_EDGE('',*,*,#14285,.T.);
#18840=ORIENTED_EDGE('',*,*,#14279,.T.);
#18841=ORIENTED_EDGE('',*,*,#14278,.T.);
#18842=ORIENTED_EDGE('',*,*,#14264,.T.);
#18843=ORIENTED_EDGE('',*,*,#14285,.F.);
#18844=ORIENTED_EDGE('',*,*,#14245,.F.);
#18845=ORIENTED_EDGE('',*,*,#14286,.T.);
#18846=ORIENTED_EDGE('',*,*,#14281,.T.);
#18847=ORIENTED_EDGE('',*,*,#14280,.T.);
#18848=ORIENTED_EDGE('',*,*,#14262,.T.);
#18849=ORIENTED_EDGE('',*,*,#14286,.F.);
#18850=ORIENTED_EDGE('',*,*,#14244,.F.);
#18851=ORIENTED_EDGE('',*,*,#14241,.F.);
#18852=ORIENTED_EDGE('',*,*,#14248,.F.);
#18853=ORIENTED_EDGE('',*,*,#14287,.T.);
#18854=ORIENTED_EDGE('',*,*,#14283,.T.);
#18855=ORIENTED_EDGE('',*,*,#14282,.T.);
#18856=ORIENTED_EDGE('',*,*,#14260,.T.);
#18857=ORIENTED_EDGE('',*,*,#14287,.F.);
#18858=ORIENTED_EDGE('',*,*,#14247,.F.);
#18859=ORIENTED_EDGE('',*,*,#14288,.T.);
#18860=ORIENTED_EDGE('',*,*,#14273,.T.);
#18861=ORIENTED_EDGE('',*,*,#14272,.T.);
#18862=ORIENTED_EDGE('',*,*,#14270,.T.);
#18863=ORIENTED_EDGE('',*,*,#14288,.F.);
#18864=ORIENTED_EDGE('',*,*,#14246,.F.);
#18865=ORIENTED_EDGE('',*,*,#14289,.T.);
#18866=ORIENTED_EDGE('',*,*,#14275,.T.);
#18867=ORIENTED_EDGE('',*,*,#14274,.T.);
#18868=ORIENTED_EDGE('',*,*,#14268,.T.);
#18869=ORIENTED_EDGE('',*,*,#14289,.F.);
#18870=ORIENTED_EDGE('',*,*,#14257,.T.);
#18871=ORIENTED_EDGE('',*,*,#14290,.T.);
#18872=ORIENTED_EDGE('',*,*,#14291,.F.);
#18873=ORIENTED_EDGE('',*,*,#14290,.F.);
#18874=ORIENTED_EDGE('',*,*,#14292,.F.);
#18875=ORIENTED_EDGE('',*,*,#14291,.T.);
#18876=ORIENTED_EDGE('',*,*,#14243,.F.);
#18877=ORIENTED_EDGE('',*,*,#14293,.T.);
#18878=ORIENTED_EDGE('',*,*,#14292,.T.);
#18879=ORIENTED_EDGE('',*,*,#14293,.F.);
#18880=ORIENTED_EDGE('',*,*,#14294,.F.);
#18881=ORIENTED_EDGE('',*,*,#14295,.T.);
#18882=ORIENTED_EDGE('',*,*,#14239,.T.);
#18883=ORIENTED_EDGE('',*,*,#14295,.F.);
#18884=ORIENTED_EDGE('',*,*,#14294,.T.);
#18885=ORIENTED_EDGE('',*,*,#14296,.F.);
#18886=ORIENTED_EDGE('',*,*,#14296,.T.);
#18887=ORIENTED_EDGE('',*,*,#14297,.T.);
#18888=ORIENTED_EDGE('',*,*,#14255,.F.);
#18889=ORIENTED_EDGE('',*,*,#14297,.F.);
#18890=ORIENTED_EDGE('',*,*,#14298,.F.);
#18891=ORIENTED_EDGE('',*,*,#14299,.T.);
#18892=ORIENTED_EDGE('',*,*,#14300,.T.);
#18893=ORIENTED_EDGE('',*,*,#14301,.T.);
#18894=ORIENTED_EDGE('',*,*,#14302,.F.);
#18895=ORIENTED_EDGE('',*,*,#14303,.T.);
#18896=ORIENTED_EDGE('',*,*,#14298,.T.);
#18897=ORIENTED_EDGE('',*,*,#14304,.T.);
#18898=ORIENTED_EDGE('',*,*,#14305,.F.);
#18899=ORIENTED_EDGE('',*,*,#14306,.T.);
#18900=ORIENTED_EDGE('',*,*,#14302,.T.);
#18901=ORIENTED_EDGE('',*,*,#14307,.T.);
#18902=ORIENTED_EDGE('',*,*,#14308,.F.);
#18903=ORIENTED_EDGE('',*,*,#14309,.T.);
#18904=ORIENTED_EDGE('',*,*,#14305,.T.);
#18905=ORIENTED_EDGE('',*,*,#14310,.T.);
#18906=ORIENTED_EDGE('',*,*,#14311,.F.);
#18907=ORIENTED_EDGE('',*,*,#14312,.T.);
#18908=ORIENTED_EDGE('',*,*,#14308,.T.);
#18909=ORIENTED_EDGE('',*,*,#14313,.T.);
#18910=ORIENTED_EDGE('',*,*,#14314,.F.);
#18911=ORIENTED_EDGE('',*,*,#14315,.T.);
#18912=ORIENTED_EDGE('',*,*,#14311,.T.);
#18913=ORIENTED_EDGE('',*,*,#14316,.T.);
#18914=ORIENTED_EDGE('',*,*,#14317,.F.);
#18915=ORIENTED_EDGE('',*,*,#14318,.T.);
#18916=ORIENTED_EDGE('',*,*,#14314,.T.);
#18917=ORIENTED_EDGE('',*,*,#14319,.T.);
#18918=ORIENTED_EDGE('',*,*,#14320,.F.);
#18919=ORIENTED_EDGE('',*,*,#14321,.T.);
#18920=ORIENTED_EDGE('',*,*,#14322,.F.);
#18921=ORIENTED_EDGE('',*,*,#14323,.F.);
#18922=ORIENTED_EDGE('',*,*,#14324,.T.);
#18923=ORIENTED_EDGE('',*,*,#14320,.T.);
#18924=ORIENTED_EDGE('',*,*,#14325,.F.);
#18925=ORIENTED_EDGE('',*,*,#14326,.F.);
#18926=ORIENTED_EDGE('',*,*,#14327,.F.);
#18927=ORIENTED_EDGE('',*,*,#14328,.T.);
#18928=ORIENTED_EDGE('',*,*,#14323,.T.);
#18929=ORIENTED_EDGE('',*,*,#14329,.F.);
#18930=ORIENTED_EDGE('',*,*,#14330,.F.);
#18931=ORIENTED_EDGE('',*,*,#14331,.T.);
#18932=ORIENTED_EDGE('',*,*,#14327,.T.);
#18933=ORIENTED_EDGE('',*,*,#14332,.F.);
#18934=ORIENTED_EDGE('',*,*,#14333,.F.);
#18935=ORIENTED_EDGE('',*,*,#14334,.T.);
#18936=ORIENTED_EDGE('',*,*,#14330,.T.);
#18937=ORIENTED_EDGE('',*,*,#14335,.F.);
#18938=ORIENTED_EDGE('',*,*,#14336,.F.);
#18939=ORIENTED_EDGE('',*,*,#14337,.T.);
#18940=ORIENTED_EDGE('',*,*,#14333,.T.);
#18941=ORIENTED_EDGE('',*,*,#14338,.F.);
#18942=ORIENTED_EDGE('',*,*,#14339,.F.);
#18943=ORIENTED_EDGE('',*,*,#14340,.T.);
#18944=ORIENTED_EDGE('',*,*,#14336,.T.);
#18945=ORIENTED_EDGE('',*,*,#14341,.F.);
#18946=ORIENTED_EDGE('',*,*,#14325,.T.);
#18947=ORIENTED_EDGE('',*,*,#14322,.T.);
#18948=ORIENTED_EDGE('',*,*,#14342,.T.);
#18949=ORIENTED_EDGE('',*,*,#14343,.F.);
#18950=ORIENTED_EDGE('',*,*,#14344,.F.);
#18951=ORIENTED_EDGE('',*,*,#14345,.T.);
#18952=ORIENTED_EDGE('',*,*,#14345,.F.);
#18953=ORIENTED_EDGE('',*,*,#14346,.F.);
#18954=ORIENTED_EDGE('',*,*,#14319,.F.);
#18955=ORIENTED_EDGE('',*,*,#14316,.F.);
#18956=ORIENTED_EDGE('',*,*,#14313,.F.);
#18957=ORIENTED_EDGE('',*,*,#14310,.F.);
#18958=ORIENTED_EDGE('',*,*,#14307,.F.);
#18959=ORIENTED_EDGE('',*,*,#14304,.F.);
#18960=ORIENTED_EDGE('',*,*,#14301,.F.);
#18961=ORIENTED_EDGE('',*,*,#14347,.F.);
#18962=ORIENTED_EDGE('',*,*,#14348,.T.);
#18963=ORIENTED_EDGE('',*,*,#14341,.T.);
#18964=ORIENTED_EDGE('',*,*,#14338,.T.);
#18965=ORIENTED_EDGE('',*,*,#14335,.T.);
#18966=ORIENTED_EDGE('',*,*,#14332,.T.);
#18967=ORIENTED_EDGE('',*,*,#14329,.T.);
#18968=ORIENTED_EDGE('',*,*,#14326,.T.);
#18969=ORIENTED_EDGE('',*,*,#14349,.T.);
#18970=ORIENTED_EDGE('',*,*,#14350,.T.);
#18971=ORIENTED_EDGE('',*,*,#14351,.T.);
#18972=ORIENTED_EDGE('',*,*,#14352,.T.);
#18973=ORIENTED_EDGE('',*,*,#14347,.T.);
#18974=ORIENTED_EDGE('',*,*,#14339,.T.);
#18975=ORIENTED_EDGE('',*,*,#14348,.F.);
#18976=ORIENTED_EDGE('',*,*,#14352,.F.);
#18977=ORIENTED_EDGE('',*,*,#14353,.T.);
#18978=ORIENTED_EDGE('',*,*,#14342,.F.);
#18979=ORIENTED_EDGE('',*,*,#14321,.F.);
#18980=ORIENTED_EDGE('',*,*,#14324,.F.);
#18981=ORIENTED_EDGE('',*,*,#14328,.F.);
#18982=ORIENTED_EDGE('',*,*,#14331,.F.);
#18983=ORIENTED_EDGE('',*,*,#14334,.F.);
#18984=ORIENTED_EDGE('',*,*,#14337,.F.);
#18985=ORIENTED_EDGE('',*,*,#14340,.F.);
#18986=ORIENTED_EDGE('',*,*,#14353,.F.);
#18987=ORIENTED_EDGE('',*,*,#14351,.F.);
#18988=ORIENTED_EDGE('',*,*,#14299,.F.);
#18989=ORIENTED_EDGE('',*,*,#14303,.F.);
#18990=ORIENTED_EDGE('',*,*,#14306,.F.);
#18991=ORIENTED_EDGE('',*,*,#14309,.F.);
#18992=ORIENTED_EDGE('',*,*,#14312,.F.);
#18993=ORIENTED_EDGE('',*,*,#14315,.F.);
#18994=ORIENTED_EDGE('',*,*,#14318,.F.);
#18995=ORIENTED_EDGE('',*,*,#14354,.F.);
#18996=ORIENTED_EDGE('',*,*,#14355,.F.);
#18997=ORIENTED_EDGE('',*,*,#14356,.F.);
#18998=ORIENTED_EDGE('',*,*,#14357,.F.);
#18999=ORIENTED_EDGE('',*,*,#14358,.F.);
#19000=ORIENTED_EDGE('',*,*,#14359,.F.);
#19001=ORIENTED_EDGE('',*,*,#14360,.F.);
#19002=ORIENTED_EDGE('',*,*,#14361,.F.);
#19003=ORIENTED_EDGE('',*,*,#14362,.F.);
#19004=ORIENTED_EDGE('',*,*,#14363,.F.);
#19005=ORIENTED_EDGE('',*,*,#14364,.F.);
#19006=ORIENTED_EDGE('',*,*,#14365,.F.);
#19007=ORIENTED_EDGE('',*,*,#14366,.F.);
#19008=ORIENTED_EDGE('',*,*,#14367,.T.);
#19009=ORIENTED_EDGE('',*,*,#14368,.F.);
#19010=ORIENTED_EDGE('',*,*,#14369,.F.);
#19011=ORIENTED_EDGE('',*,*,#14358,.T.);
#19012=ORIENTED_EDGE('',*,*,#14370,.F.);
#19013=ORIENTED_EDGE('',*,*,#14371,.F.);
#19014=ORIENTED_EDGE('',*,*,#14372,.F.);
#19015=ORIENTED_EDGE('',*,*,#14356,.T.);
#19016=ORIENTED_EDGE('',*,*,#14373,.F.);
#19017=ORIENTED_EDGE('',*,*,#14374,.F.);
#19018=ORIENTED_EDGE('',*,*,#14375,.F.);
#19019=ORIENTED_EDGE('',*,*,#14366,.T.);
#19020=ORIENTED_EDGE('',*,*,#14376,.F.);
#19021=ORIENTED_EDGE('',*,*,#14377,.F.);
#19022=ORIENTED_EDGE('',*,*,#14378,.F.);
#19023=ORIENTED_EDGE('',*,*,#14364,.T.);
#19024=ORIENTED_EDGE('',*,*,#14379,.F.);
#19025=ORIENTED_EDGE('',*,*,#14380,.F.);
#19026=ORIENTED_EDGE('',*,*,#14381,.F.);
#19027=ORIENTED_EDGE('',*,*,#14362,.T.);
#19028=ORIENTED_EDGE('',*,*,#14382,.F.);
#19029=ORIENTED_EDGE('',*,*,#14383,.F.);
#19030=ORIENTED_EDGE('',*,*,#14384,.F.);
#19031=ORIENTED_EDGE('',*,*,#14360,.T.);
#19032=ORIENTED_EDGE('',*,*,#14385,.F.);
#19033=ORIENTED_EDGE('',*,*,#14386,.F.);
#19034=ORIENTED_EDGE('',*,*,#14367,.F.);
#19035=ORIENTED_EDGE('',*,*,#14359,.T.);
#19036=ORIENTED_EDGE('',*,*,#14387,.F.);
#19037=ORIENTED_EDGE('',*,*,#14388,.F.);
#19038=ORIENTED_EDGE('',*,*,#14389,.T.);
#19039=ORIENTED_EDGE('',*,*,#14385,.T.);
#19040=ORIENTED_EDGE('',*,*,#14390,.T.);
#19041=ORIENTED_EDGE('',*,*,#14391,.T.);
#19042=ORIENTED_EDGE('',*,*,#14361,.T.);
#19043=ORIENTED_EDGE('',*,*,#14392,.F.);
#19044=ORIENTED_EDGE('',*,*,#14393,.F.);
#19045=ORIENTED_EDGE('',*,*,#14387,.T.);
#19046=ORIENTED_EDGE('',*,*,#14381,.T.);
#19047=ORIENTED_EDGE('',*,*,#14394,.T.);
#19048=ORIENTED_EDGE('',*,*,#14395,.F.);
#19049=ORIENTED_EDGE('',*,*,#14382,.T.);
#19050=ORIENTED_EDGE('',*,*,#14396,.T.);
#19051=ORIENTED_EDGE('',*,*,#14397,.T.);
#19052=ORIENTED_EDGE('',*,*,#14357,.T.);
#19053=ORIENTED_EDGE('',*,*,#14389,.F.);
#19054=ORIENTED_EDGE('',*,*,#14398,.F.);
#19055=ORIENTED_EDGE('',*,*,#14399,.T.);
#19056=ORIENTED_EDGE('',*,*,#14370,.T.);
#19057=ORIENTED_EDGE('',*,*,#14400,.T.);
#19058=ORIENTED_EDGE('',*,*,#14401,.T.);
#19059=ORIENTED_EDGE('',*,*,#14363,.T.);
#19060=ORIENTED_EDGE('',*,*,#14402,.F.);
#19061=ORIENTED_EDGE('',*,*,#14403,.F.);
#19062=ORIENTED_EDGE('',*,*,#14392,.T.);
#19063=ORIENTED_EDGE('',*,*,#14378,.T.);
#19064=ORIENTED_EDGE('',*,*,#14404,.T.);
#19065=ORIENTED_EDGE('',*,*,#14405,.F.);
#19066=ORIENTED_EDGE('',*,*,#14379,.T.);
#19067=ORIENTED_EDGE('',*,*,#14395,.T.);
#19068=ORIENTED_EDGE('',*,*,#14406,.T.);
#19069=ORIENTED_EDGE('',*,*,#14383,.T.);
#19070=ORIENTED_EDGE('',*,*,#14397,.F.);
#19071=ORIENTED_EDGE('',*,*,#14407,.F.);
#19072=ORIENTED_EDGE('',*,*,#14380,.T.);
#19073=ORIENTED_EDGE('',*,*,#14406,.F.);
#19074=ORIENTED_EDGE('',*,*,#14394,.F.);
#19075=ORIENTED_EDGE('',*,*,#14377,.T.);
#19076=ORIENTED_EDGE('',*,*,#14408,.F.);
#19077=ORIENTED_EDGE('',*,*,#14404,.F.);
#19078=ORIENTED_EDGE('',*,*,#14374,.T.);
#19079=ORIENTED_EDGE('',*,*,#14409,.F.);
#19080=ORIENTED_EDGE('',*,*,#14410,.F.);
#19081=ORIENTED_EDGE('',*,*,#14371,.T.);
#19082=ORIENTED_EDGE('',*,*,#14401,.F.);
#19083=ORIENTED_EDGE('',*,*,#14411,.F.);
#19084=ORIENTED_EDGE('',*,*,#14368,.T.);
#19085=ORIENTED_EDGE('',*,*,#14386,.T.);
#19086=ORIENTED_EDGE('',*,*,#14391,.F.);
#19087=ORIENTED_EDGE('',*,*,#14412,.F.);
#19088=ORIENTED_EDGE('',*,*,#14365,.T.);
#19089=ORIENTED_EDGE('',*,*,#14413,.F.);
#19090=ORIENTED_EDGE('',*,*,#14414,.F.);
#19091=ORIENTED_EDGE('',*,*,#14402,.T.);
#19092=ORIENTED_EDGE('',*,*,#14375,.T.);
#19093=ORIENTED_EDGE('',*,*,#14410,.T.);
#19094=ORIENTED_EDGE('',*,*,#14415,.F.);
#19095=ORIENTED_EDGE('',*,*,#14376,.T.);
#19096=ORIENTED_EDGE('',*,*,#14405,.T.);
#19097=ORIENTED_EDGE('',*,*,#14408,.T.);
#19098=ORIENTED_EDGE('',*,*,#14373,.T.);
#19099=ORIENTED_EDGE('',*,*,#14415,.T.);
#19100=ORIENTED_EDGE('',*,*,#14409,.T.);
#19101=ORIENTED_EDGE('',*,*,#14355,.T.);
#19102=ORIENTED_EDGE('',*,*,#14399,.F.);
#19103=ORIENTED_EDGE('',*,*,#14416,.F.);
#19104=ORIENTED_EDGE('',*,*,#14413,.T.);
#19105=ORIENTED_EDGE('',*,*,#14384,.T.);
#19106=ORIENTED_EDGE('',*,*,#14407,.T.);
#19107=ORIENTED_EDGE('',*,*,#14396,.F.);
#19108=ORIENTED_EDGE('',*,*,#14369,.T.);
#19109=ORIENTED_EDGE('',*,*,#14412,.T.);
#19110=ORIENTED_EDGE('',*,*,#14390,.F.);
#19111=ORIENTED_EDGE('',*,*,#14372,.T.);
#19112=ORIENTED_EDGE('',*,*,#14411,.T.);
#19113=ORIENTED_EDGE('',*,*,#14400,.F.);
#19114=ORIENTED_EDGE('',*,*,#14417,.F.);
#19115=ORIENTED_EDGE('',*,*,#14349,.F.);
#19116=ORIENTED_EDGE('',*,*,#14300,.F.);
#19117=ORIENTED_EDGE('',*,*,#14350,.F.);
#19118=ORIENTED_EDGE('',*,*,#14418,.T.);
#19119=ORIENTED_EDGE('',*,*,#14417,.T.);
#19120=ORIENTED_EDGE('',*,*,#14418,.F.);
#19121=ORIENTED_EDGE('',*,*,#14317,.T.);
#19122=ORIENTED_EDGE('',*,*,#14346,.T.);
#19123=ORIENTED_EDGE('',*,*,#14419,.F.);
#19124=ORIENTED_EDGE('',*,*,#14354,.T.);
#19125=ORIENTED_EDGE('',*,*,#14420,.F.);
#19126=ORIENTED_EDGE('',*,*,#14421,.T.);
#19127=ORIENTED_EDGE('',*,*,#14343,.T.);
#19128=ORIENTED_EDGE('',*,*,#14419,.T.);
#19129=ORIENTED_EDGE('',*,*,#14344,.T.);
#19130=ORIENTED_EDGE('',*,*,#14421,.F.);
#19131=ORIENTED_EDGE('',*,*,#14420,.T.);
#19132=ORIENTED_EDGE('',*,*,#14403,.T.);
#19133=ORIENTED_EDGE('',*,*,#14414,.T.);
#19134=ORIENTED_EDGE('',*,*,#14416,.T.);
#19135=ORIENTED_EDGE('',*,*,#14398,.T.);
#19136=ORIENTED_EDGE('',*,*,#14388,.T.);
#19137=ORIENTED_EDGE('',*,*,#14393,.T.);
#19138=ORIENTED_EDGE('',*,*,#14422,.F.);
#19139=ORIENTED_EDGE('',*,*,#14423,.T.);
#19140=ORIENTED_EDGE('',*,*,#14424,.T.);
#19141=ORIENTED_EDGE('',*,*,#14425,.F.);
#19142=ORIENTED_EDGE('',*,*,#14426,.F.);
#19143=ORIENTED_EDGE('',*,*,#14427,.T.);
#19144=ORIENTED_EDGE('',*,*,#14428,.T.);
#19145=ORIENTED_EDGE('',*,*,#14423,.F.);
#19146=ORIENTED_EDGE('',*,*,#14429,.F.);
#19147=ORIENTED_EDGE('',*,*,#14430,.T.);
#19148=ORIENTED_EDGE('',*,*,#14431,.T.);
#19149=ORIENTED_EDGE('',*,*,#14427,.F.);
#19150=ORIENTED_EDGE('',*,*,#14432,.F.);
#19151=ORIENTED_EDGE('',*,*,#14425,.T.);
#19152=ORIENTED_EDGE('',*,*,#14433,.T.);
#19153=ORIENTED_EDGE('',*,*,#14430,.F.);
#19154=ORIENTED_EDGE('',*,*,#14433,.F.);
#19155=ORIENTED_EDGE('',*,*,#14424,.F.);
#19156=ORIENTED_EDGE('',*,*,#14428,.F.);
#19157=ORIENTED_EDGE('',*,*,#14431,.F.);
#19158=ORIENTED_EDGE('',*,*,#14434,.F.);
#19159=ORIENTED_EDGE('',*,*,#14435,.T.);
#19160=ORIENTED_EDGE('',*,*,#14436,.T.);
#19161=ORIENTED_EDGE('',*,*,#14437,.F.);
#19162=ORIENTED_EDGE('',*,*,#14438,.F.);
#19163=ORIENTED_EDGE('',*,*,#14439,.T.);
#19164=ORIENTED_EDGE('',*,*,#14440,.T.);
#19165=ORIENTED_EDGE('',*,*,#14435,.F.);
#19166=ORIENTED_EDGE('',*,*,#14441,.F.);
#19167=ORIENTED_EDGE('',*,*,#14442,.T.);
#19168=ORIENTED_EDGE('',*,*,#14443,.T.);
#19169=ORIENTED_EDGE('',*,*,#14439,.F.);
#19170=ORIENTED_EDGE('',*,*,#14444,.F.);
#19171=ORIENTED_EDGE('',*,*,#14437,.T.);
#19172=ORIENTED_EDGE('',*,*,#14445,.T.);
#19173=ORIENTED_EDGE('',*,*,#14442,.F.);
#19174=ORIENTED_EDGE('',*,*,#14445,.F.);
#19175=ORIENTED_EDGE('',*,*,#14436,.F.);
#19176=ORIENTED_EDGE('',*,*,#14440,.F.);
#19177=ORIENTED_EDGE('',*,*,#14443,.F.);
#19178=ORIENTED_EDGE('',*,*,#14446,.F.);
#19179=ORIENTED_EDGE('',*,*,#14447,.F.);
#19180=ORIENTED_EDGE('',*,*,#14448,.F.);
#19181=ORIENTED_EDGE('',*,*,#14449,.F.);
#19182=ORIENTED_EDGE('',*,*,#14450,.F.);
#19183=ORIENTED_EDGE('',*,*,#14451,.F.);
#19184=ORIENTED_EDGE('',*,*,#14452,.F.);
#19185=ORIENTED_EDGE('',*,*,#14453,.F.);
#19186=ORIENTED_EDGE('',*,*,#14454,.F.);
#19187=ORIENTED_EDGE('',*,*,#14455,.F.);
#19188=ORIENTED_EDGE('',*,*,#14456,.F.);
#19189=ORIENTED_EDGE('',*,*,#14457,.F.);
#19190=ORIENTED_EDGE('',*,*,#14458,.F.);
#19191=ORIENTED_EDGE('',*,*,#14459,.F.);
#19192=ORIENTED_EDGE('',*,*,#14460,.F.);
#19193=ORIENTED_EDGE('',*,*,#14459,.T.);
#19194=ORIENTED_EDGE('',*,*,#14461,.T.);
#19195=ORIENTED_EDGE('',*,*,#14454,.T.);
#19196=ORIENTED_EDGE('',*,*,#14462,.T.);
#19197=ORIENTED_EDGE('',*,*,#14463,.F.);
#19198=ORIENTED_EDGE('',*,*,#14464,.F.);
#19199=ORIENTED_EDGE('',*,*,#14465,.F.);
#19200=ORIENTED_EDGE('',*,*,#14466,.F.);
#19201=ORIENTED_EDGE('',*,*,#14467,.F.);
#19202=ORIENTED_EDGE('',*,*,#14468,.F.);
#19203=ORIENTED_EDGE('',*,*,#14453,.T.);
#19204=ORIENTED_EDGE('',*,*,#14469,.T.);
#19205=ORIENTED_EDGE('',*,*,#14467,.T.);
#19206=ORIENTED_EDGE('',*,*,#14470,.T.);
#19207=ORIENTED_EDGE('',*,*,#14456,.T.);
#19208=ORIENTED_EDGE('',*,*,#14471,.T.);
#19209=ORIENTED_EDGE('',*,*,#14468,.T.);
#19210=ORIENTED_EDGE('',*,*,#14472,.T.);
#19211=ORIENTED_EDGE('',*,*,#14473,.F.);
#19212=ORIENTED_EDGE('',*,*,#14474,.F.);
#19213=ORIENTED_EDGE('',*,*,#14475,.F.);
#19214=ORIENTED_EDGE('',*,*,#14474,.T.);
#19215=ORIENTED_EDGE('',*,*,#14476,.T.);
#19216=ORIENTED_EDGE('',*,*,#14460,.T.);
#19217=ORIENTED_EDGE('',*,*,#14477,.T.);
#19218=ORIENTED_EDGE('',*,*,#14466,.T.);
#19219=ORIENTED_EDGE('',*,*,#14478,.T.);
#19220=ORIENTED_EDGE('',*,*,#14475,.T.);
#19221=ORIENTED_EDGE('',*,*,#14479,.T.);
#19222=ORIENTED_EDGE('',*,*,#14464,.T.);
#19223=ORIENTED_EDGE('',*,*,#14480,.T.);
#19224=ORIENTED_EDGE('',*,*,#14473,.T.);
#19225=ORIENTED_EDGE('',*,*,#14481,.T.);
#19226=ORIENTED_EDGE('',*,*,#14455,.T.);
#19227=ORIENTED_EDGE('',*,*,#14482,.T.);
#19228=ORIENTED_EDGE('',*,*,#14465,.T.);
#19229=ORIENTED_EDGE('',*,*,#14483,.T.);
#19230=ORIENTED_EDGE('',*,*,#14463,.T.);
#19231=ORIENTED_EDGE('',*,*,#14484,.T.);
#19232=ORIENTED_EDGE('',*,*,#14451,.T.);
#19233=ORIENTED_EDGE('',*,*,#14485,.T.);
#19234=ORIENTED_EDGE('',*,*,#14450,.T.);
#19235=ORIENTED_EDGE('',*,*,#14486,.T.);
#19236=ORIENTED_EDGE('',*,*,#14458,.T.);
#19237=ORIENTED_EDGE('',*,*,#14487,.T.);
#19238=ORIENTED_EDGE('',*,*,#14446,.T.);
#19239=ORIENTED_EDGE('',*,*,#14488,.T.);
#19240=ORIENTED_EDGE('',*,*,#14457,.T.);
#19241=ORIENTED_EDGE('',*,*,#14489,.T.);
#19242=ORIENTED_EDGE('',*,*,#14447,.T.);
#19243=ORIENTED_EDGE('',*,*,#14490,.T.);
#19244=ORIENTED_EDGE('',*,*,#14452,.T.);
#19245=ORIENTED_EDGE('',*,*,#14491,.T.);
#19246=ORIENTED_EDGE('',*,*,#14449,.T.);
#19247=ORIENTED_EDGE('',*,*,#14492,.T.);
#19248=ORIENTED_EDGE('',*,*,#14448,.T.);
#19249=ORIENTED_EDGE('',*,*,#14493,.T.);
#19250=ORIENTED_EDGE('',*,*,#14461,.F.);
#19251=ORIENTED_EDGE('',*,*,#14486,.F.);
#19252=ORIENTED_EDGE('',*,*,#14493,.F.);
#19253=ORIENTED_EDGE('',*,*,#14491,.F.);
#19254=ORIENTED_EDGE('',*,*,#14462,.F.);
#19255=ORIENTED_EDGE('',*,*,#14470,.F.);
#19256=ORIENTED_EDGE('',*,*,#14479,.F.);
#19257=ORIENTED_EDGE('',*,*,#14477,.F.);
#19258=ORIENTED_EDGE('',*,*,#14469,.F.);
#19259=ORIENTED_EDGE('',*,*,#14490,.F.);
#19260=ORIENTED_EDGE('',*,*,#14489,.F.);
#19261=ORIENTED_EDGE('',*,*,#14472,.F.);
#19262=ORIENTED_EDGE('',*,*,#14471,.F.);
#19263=ORIENTED_EDGE('',*,*,#14483,.F.);
#19264=ORIENTED_EDGE('',*,*,#14481,.F.);
#19265=ORIENTED_EDGE('',*,*,#14478,.F.);
#19266=ORIENTED_EDGE('',*,*,#14476,.F.);
#19267=ORIENTED_EDGE('',*,*,#14480,.F.);
#19268=ORIENTED_EDGE('',*,*,#14485,.F.);
#19269=ORIENTED_EDGE('',*,*,#14487,.F.);
#19270=ORIENTED_EDGE('',*,*,#14422,.T.);
#19271=ORIENTED_EDGE('',*,*,#14432,.T.);
#19272=ORIENTED_EDGE('',*,*,#14429,.T.);
#19273=ORIENTED_EDGE('',*,*,#14426,.T.);
#19274=ORIENTED_EDGE('',*,*,#14434,.T.);
#19275=ORIENTED_EDGE('',*,*,#14444,.T.);
#19276=ORIENTED_EDGE('',*,*,#14441,.T.);
#19277=ORIENTED_EDGE('',*,*,#14438,.T.);
#19278=ORIENTED_EDGE('',*,*,#14482,.F.);
#19279=ORIENTED_EDGE('',*,*,#14488,.F.);
#19280=ORIENTED_EDGE('',*,*,#14492,.F.);
#19281=ORIENTED_EDGE('',*,*,#14484,.F.);
#19282=ORIENTED_EDGE('',*,*,#14494,.F.);
#19283=ORIENTED_EDGE('',*,*,#14495,.T.);
#19284=ORIENTED_EDGE('',*,*,#14496,.T.);
#19285=ORIENTED_EDGE('',*,*,#14497,.T.);
#19286=ORIENTED_EDGE('',*,*,#14498,.F.);
#19287=ORIENTED_EDGE('',*,*,#14499,.T.);
#19288=ORIENTED_EDGE('',*,*,#14494,.T.);
#19289=ORIENTED_EDGE('',*,*,#14500,.T.);
#19290=ORIENTED_EDGE('',*,*,#14501,.F.);
#19291=ORIENTED_EDGE('',*,*,#14502,.T.);
#19292=ORIENTED_EDGE('',*,*,#14498,.T.);
#19293=ORIENTED_EDGE('',*,*,#14503,.T.);
#19294=ORIENTED_EDGE('',*,*,#14504,.F.);
#19295=ORIENTED_EDGE('',*,*,#14505,.T.);
#19296=ORIENTED_EDGE('',*,*,#14501,.T.);
#19297=ORIENTED_EDGE('',*,*,#14506,.T.);
#19298=ORIENTED_EDGE('',*,*,#14507,.F.);
#19299=ORIENTED_EDGE('',*,*,#14508,.T.);
#19300=ORIENTED_EDGE('',*,*,#14504,.T.);
#19301=ORIENTED_EDGE('',*,*,#14509,.T.);
#19302=ORIENTED_EDGE('',*,*,#14510,.F.);
#19303=ORIENTED_EDGE('',*,*,#14511,.T.);
#19304=ORIENTED_EDGE('',*,*,#14507,.T.);
#19305=ORIENTED_EDGE('',*,*,#14512,.T.);
#19306=ORIENTED_EDGE('',*,*,#14513,.F.);
#19307=ORIENTED_EDGE('',*,*,#14514,.T.);
#19308=ORIENTED_EDGE('',*,*,#14510,.T.);
#19309=ORIENTED_EDGE('',*,*,#14515,.T.);
#19310=ORIENTED_EDGE('',*,*,#14516,.F.);
#19311=ORIENTED_EDGE('',*,*,#14517,.T.);
#19312=ORIENTED_EDGE('',*,*,#14513,.T.);
#19313=ORIENTED_EDGE('',*,*,#14518,.T.);
#19314=ORIENTED_EDGE('',*,*,#14519,.F.);
#19315=ORIENTED_EDGE('',*,*,#14520,.T.);
#19316=ORIENTED_EDGE('',*,*,#14516,.T.);
#19317=ORIENTED_EDGE('',*,*,#14521,.T.);
#19318=ORIENTED_EDGE('',*,*,#14522,.F.);
#19319=ORIENTED_EDGE('',*,*,#14523,.T.);
#19320=ORIENTED_EDGE('',*,*,#14519,.T.);
#19321=ORIENTED_EDGE('',*,*,#14524,.T.);
#19322=ORIENTED_EDGE('',*,*,#14525,.F.);
#19323=ORIENTED_EDGE('',*,*,#14526,.T.);
#19324=ORIENTED_EDGE('',*,*,#14522,.T.);
#19325=ORIENTED_EDGE('',*,*,#14527,.T.);
#19326=ORIENTED_EDGE('',*,*,#14528,.F.);
#19327=ORIENTED_EDGE('',*,*,#14529,.T.);
#19328=ORIENTED_EDGE('',*,*,#14525,.T.);
#19329=ORIENTED_EDGE('',*,*,#14530,.T.);
#19330=ORIENTED_EDGE('',*,*,#14531,.F.);
#19331=ORIENTED_EDGE('',*,*,#14532,.T.);
#19332=ORIENTED_EDGE('',*,*,#14528,.T.);
#19333=ORIENTED_EDGE('',*,*,#14533,.T.);
#19334=ORIENTED_EDGE('',*,*,#14534,.F.);
#19335=ORIENTED_EDGE('',*,*,#14535,.T.);
#19336=ORIENTED_EDGE('',*,*,#14531,.T.);
#19337=ORIENTED_EDGE('',*,*,#14536,.T.);
#19338=ORIENTED_EDGE('',*,*,#14537,.F.);
#19339=ORIENTED_EDGE('',*,*,#14538,.T.);
#19340=ORIENTED_EDGE('',*,*,#14534,.T.);
#19341=ORIENTED_EDGE('',*,*,#14539,.T.);
#19342=ORIENTED_EDGE('',*,*,#14540,.F.);
#19343=ORIENTED_EDGE('',*,*,#14541,.T.);
#19344=ORIENTED_EDGE('',*,*,#14537,.T.);
#19345=ORIENTED_EDGE('',*,*,#14542,.T.);
#19346=ORIENTED_EDGE('',*,*,#14543,.F.);
#19347=ORIENTED_EDGE('',*,*,#14544,.T.);
#19348=ORIENTED_EDGE('',*,*,#14540,.T.);
#19349=ORIENTED_EDGE('',*,*,#14545,.T.);
#19350=ORIENTED_EDGE('',*,*,#14546,.F.);
#19351=ORIENTED_EDGE('',*,*,#14547,.T.);
#19352=ORIENTED_EDGE('',*,*,#14543,.T.);
#19353=ORIENTED_EDGE('',*,*,#14548,.T.);
#19354=ORIENTED_EDGE('',*,*,#14549,.F.);
#19355=ORIENTED_EDGE('',*,*,#14550,.T.);
#19356=ORIENTED_EDGE('',*,*,#14546,.T.);
#19357=ORIENTED_EDGE('',*,*,#14551,.T.);
#19358=ORIENTED_EDGE('',*,*,#14552,.F.);
#19359=ORIENTED_EDGE('',*,*,#14553,.T.);
#19360=ORIENTED_EDGE('',*,*,#14549,.T.);
#19361=ORIENTED_EDGE('',*,*,#14554,.T.);
#19362=ORIENTED_EDGE('',*,*,#14555,.F.);
#19363=ORIENTED_EDGE('',*,*,#14556,.T.);
#19364=ORIENTED_EDGE('',*,*,#14552,.T.);
#19365=ORIENTED_EDGE('',*,*,#14557,.T.);
#19366=ORIENTED_EDGE('',*,*,#14558,.F.);
#19367=ORIENTED_EDGE('',*,*,#14559,.T.);
#19368=ORIENTED_EDGE('',*,*,#14555,.T.);
#19369=ORIENTED_EDGE('',*,*,#14560,.T.);
#19370=ORIENTED_EDGE('',*,*,#14561,.F.);
#19371=ORIENTED_EDGE('',*,*,#14562,.T.);
#19372=ORIENTED_EDGE('',*,*,#14558,.T.);
#19373=ORIENTED_EDGE('',*,*,#14563,.T.);
#19374=ORIENTED_EDGE('',*,*,#14564,.F.);
#19375=ORIENTED_EDGE('',*,*,#14565,.T.);
#19376=ORIENTED_EDGE('',*,*,#14561,.T.);
#19377=ORIENTED_EDGE('',*,*,#14566,.T.);
#19378=ORIENTED_EDGE('',*,*,#14567,.F.);
#19379=ORIENTED_EDGE('',*,*,#14568,.T.);
#19380=ORIENTED_EDGE('',*,*,#14564,.T.);
#19381=ORIENTED_EDGE('',*,*,#14569,.T.);
#19382=ORIENTED_EDGE('',*,*,#14570,.F.);
#19383=ORIENTED_EDGE('',*,*,#14571,.T.);
#19384=ORIENTED_EDGE('',*,*,#14567,.T.);
#19385=ORIENTED_EDGE('',*,*,#14572,.T.);
#19386=ORIENTED_EDGE('',*,*,#14573,.F.);
#19387=ORIENTED_EDGE('',*,*,#14574,.T.);
#19388=ORIENTED_EDGE('',*,*,#14570,.T.);
#19389=ORIENTED_EDGE('',*,*,#14575,.T.);
#19390=ORIENTED_EDGE('',*,*,#14576,.F.);
#19391=ORIENTED_EDGE('',*,*,#14577,.T.);
#19392=ORIENTED_EDGE('',*,*,#14573,.T.);
#19393=ORIENTED_EDGE('',*,*,#14578,.T.);
#19394=ORIENTED_EDGE('',*,*,#14579,.F.);
#19395=ORIENTED_EDGE('',*,*,#14580,.T.);
#19396=ORIENTED_EDGE('',*,*,#14576,.T.);
#19397=ORIENTED_EDGE('',*,*,#14581,.T.);
#19398=ORIENTED_EDGE('',*,*,#14582,.F.);
#19399=ORIENTED_EDGE('',*,*,#14583,.T.);
#19400=ORIENTED_EDGE('',*,*,#14584,.F.);
#19401=ORIENTED_EDGE('',*,*,#14585,.F.);
#19402=ORIENTED_EDGE('',*,*,#14586,.T.);
#19403=ORIENTED_EDGE('',*,*,#14582,.T.);
#19404=ORIENTED_EDGE('',*,*,#14587,.F.);
#19405=ORIENTED_EDGE('',*,*,#14588,.F.);
#19406=ORIENTED_EDGE('',*,*,#14589,.F.);
#19407=ORIENTED_EDGE('',*,*,#14590,.T.);
#19408=ORIENTED_EDGE('',*,*,#14585,.T.);
#19409=ORIENTED_EDGE('',*,*,#14591,.F.);
#19410=ORIENTED_EDGE('',*,*,#14592,.F.);
#19411=ORIENTED_EDGE('',*,*,#14593,.T.);
#19412=ORIENTED_EDGE('',*,*,#14589,.T.);
#19413=ORIENTED_EDGE('',*,*,#14594,.F.);
#19414=ORIENTED_EDGE('',*,*,#14595,.F.);
#19415=ORIENTED_EDGE('',*,*,#14596,.T.);
#19416=ORIENTED_EDGE('',*,*,#14592,.T.);
#19417=ORIENTED_EDGE('',*,*,#14597,.F.);
#19418=ORIENTED_EDGE('',*,*,#14598,.F.);
#19419=ORIENTED_EDGE('',*,*,#14599,.T.);
#19420=ORIENTED_EDGE('',*,*,#14595,.T.);
#19421=ORIENTED_EDGE('',*,*,#14600,.F.);
#19422=ORIENTED_EDGE('',*,*,#14601,.F.);
#19423=ORIENTED_EDGE('',*,*,#14602,.T.);
#19424=ORIENTED_EDGE('',*,*,#14598,.T.);
#19425=ORIENTED_EDGE('',*,*,#14603,.F.);
#19426=ORIENTED_EDGE('',*,*,#14604,.F.);
#19427=ORIENTED_EDGE('',*,*,#14605,.T.);
#19428=ORIENTED_EDGE('',*,*,#14601,.T.);
#19429=ORIENTED_EDGE('',*,*,#14606,.F.);
#19430=ORIENTED_EDGE('',*,*,#14607,.F.);
#19431=ORIENTED_EDGE('',*,*,#14608,.T.);
#19432=ORIENTED_EDGE('',*,*,#14604,.T.);
#19433=ORIENTED_EDGE('',*,*,#14609,.F.);
#19434=ORIENTED_EDGE('',*,*,#14610,.F.);
#19435=ORIENTED_EDGE('',*,*,#14611,.T.);
#19436=ORIENTED_EDGE('',*,*,#14607,.T.);
#19437=ORIENTED_EDGE('',*,*,#14612,.F.);
#19438=ORIENTED_EDGE('',*,*,#14613,.F.);
#19439=ORIENTED_EDGE('',*,*,#14614,.T.);
#19440=ORIENTED_EDGE('',*,*,#14610,.T.);
#19441=ORIENTED_EDGE('',*,*,#14615,.F.);
#19442=ORIENTED_EDGE('',*,*,#14616,.F.);
#19443=ORIENTED_EDGE('',*,*,#14617,.T.);
#19444=ORIENTED_EDGE('',*,*,#14613,.T.);
#19445=ORIENTED_EDGE('',*,*,#14618,.F.);
#19446=ORIENTED_EDGE('',*,*,#14619,.F.);
#19447=ORIENTED_EDGE('',*,*,#14620,.T.);
#19448=ORIENTED_EDGE('',*,*,#14616,.T.);
#19449=ORIENTED_EDGE('',*,*,#14621,.F.);
#19450=ORIENTED_EDGE('',*,*,#14622,.F.);
#19451=ORIENTED_EDGE('',*,*,#14623,.T.);
#19452=ORIENTED_EDGE('',*,*,#14619,.T.);
#19453=ORIENTED_EDGE('',*,*,#14624,.F.);
#19454=ORIENTED_EDGE('',*,*,#14625,.F.);
#19455=ORIENTED_EDGE('',*,*,#14626,.T.);
#19456=ORIENTED_EDGE('',*,*,#14622,.T.);
#19457=ORIENTED_EDGE('',*,*,#14627,.F.);
#19458=ORIENTED_EDGE('',*,*,#14628,.F.);
#19459=ORIENTED_EDGE('',*,*,#14629,.T.);
#19460=ORIENTED_EDGE('',*,*,#14625,.T.);
#19461=ORIENTED_EDGE('',*,*,#14630,.F.);
#19462=ORIENTED_EDGE('',*,*,#14631,.F.);
#19463=ORIENTED_EDGE('',*,*,#14632,.T.);
#19464=ORIENTED_EDGE('',*,*,#14628,.T.);
#19465=ORIENTED_EDGE('',*,*,#14633,.F.);
#19466=ORIENTED_EDGE('',*,*,#14634,.F.);
#19467=ORIENTED_EDGE('',*,*,#14635,.T.);
#19468=ORIENTED_EDGE('',*,*,#14631,.T.);
#19469=ORIENTED_EDGE('',*,*,#14636,.F.);
#19470=ORIENTED_EDGE('',*,*,#14637,.F.);
#19471=ORIENTED_EDGE('',*,*,#14638,.T.);
#19472=ORIENTED_EDGE('',*,*,#14634,.T.);
#19473=ORIENTED_EDGE('',*,*,#14639,.F.);
#19474=ORIENTED_EDGE('',*,*,#14640,.F.);
#19475=ORIENTED_EDGE('',*,*,#14641,.T.);
#19476=ORIENTED_EDGE('',*,*,#14637,.T.);
#19477=ORIENTED_EDGE('',*,*,#14642,.F.);
#19478=ORIENTED_EDGE('',*,*,#14643,.F.);
#19479=ORIENTED_EDGE('',*,*,#14644,.T.);
#19480=ORIENTED_EDGE('',*,*,#14640,.T.);
#19481=ORIENTED_EDGE('',*,*,#14645,.F.);
#19482=ORIENTED_EDGE('',*,*,#14646,.F.);
#19483=ORIENTED_EDGE('',*,*,#14647,.T.);
#19484=ORIENTED_EDGE('',*,*,#14643,.T.);
#19485=ORIENTED_EDGE('',*,*,#14648,.F.);
#19486=ORIENTED_EDGE('',*,*,#14649,.F.);
#19487=ORIENTED_EDGE('',*,*,#14650,.T.);
#19488=ORIENTED_EDGE('',*,*,#14646,.T.);
#19489=ORIENTED_EDGE('',*,*,#14651,.F.);
#19490=ORIENTED_EDGE('',*,*,#14652,.F.);
#19491=ORIENTED_EDGE('',*,*,#14653,.T.);
#19492=ORIENTED_EDGE('',*,*,#14649,.T.);
#19493=ORIENTED_EDGE('',*,*,#14654,.F.);
#19494=ORIENTED_EDGE('',*,*,#14655,.F.);
#19495=ORIENTED_EDGE('',*,*,#14656,.T.);
#19496=ORIENTED_EDGE('',*,*,#14652,.T.);
#19497=ORIENTED_EDGE('',*,*,#14657,.F.);
#19498=ORIENTED_EDGE('',*,*,#14658,.F.);
#19499=ORIENTED_EDGE('',*,*,#14659,.T.);
#19500=ORIENTED_EDGE('',*,*,#14655,.T.);
#19501=ORIENTED_EDGE('',*,*,#14660,.F.);
#19502=ORIENTED_EDGE('',*,*,#14661,.F.);
#19503=ORIENTED_EDGE('',*,*,#14662,.T.);
#19504=ORIENTED_EDGE('',*,*,#14658,.T.);
#19505=ORIENTED_EDGE('',*,*,#14663,.F.);
#19506=ORIENTED_EDGE('',*,*,#14664,.F.);
#19507=ORIENTED_EDGE('',*,*,#14665,.T.);
#19508=ORIENTED_EDGE('',*,*,#14661,.T.);
#19509=ORIENTED_EDGE('',*,*,#14666,.F.);
#19510=ORIENTED_EDGE('',*,*,#14667,.F.);
#19511=ORIENTED_EDGE('',*,*,#14668,.T.);
#19512=ORIENTED_EDGE('',*,*,#14664,.T.);
#19513=ORIENTED_EDGE('',*,*,#14669,.F.);
#19514=ORIENTED_EDGE('',*,*,#14587,.T.);
#19515=ORIENTED_EDGE('',*,*,#14584,.T.);
#19516=ORIENTED_EDGE('',*,*,#14670,.T.);
#19517=ORIENTED_EDGE('',*,*,#14671,.F.);
#19518=ORIENTED_EDGE('',*,*,#14672,.F.);
#19519=ORIENTED_EDGE('',*,*,#14673,.T.);
#19520=ORIENTED_EDGE('',*,*,#14673,.F.);
#19521=ORIENTED_EDGE('',*,*,#14674,.F.);
#19522=ORIENTED_EDGE('',*,*,#14581,.F.);
#19523=ORIENTED_EDGE('',*,*,#14578,.F.);
#19524=ORIENTED_EDGE('',*,*,#14575,.F.);
#19525=ORIENTED_EDGE('',*,*,#14572,.F.);
#19526=ORIENTED_EDGE('',*,*,#14569,.F.);
#19527=ORIENTED_EDGE('',*,*,#14566,.F.);
#19528=ORIENTED_EDGE('',*,*,#14563,.F.);
#19529=ORIENTED_EDGE('',*,*,#14560,.F.);
#19530=ORIENTED_EDGE('',*,*,#14557,.F.);
#19531=ORIENTED_EDGE('',*,*,#14554,.F.);
#19532=ORIENTED_EDGE('',*,*,#14551,.F.);
#19533=ORIENTED_EDGE('',*,*,#14548,.F.);
#19534=ORIENTED_EDGE('',*,*,#14545,.F.);
#19535=ORIENTED_EDGE('',*,*,#14542,.F.);
#19536=ORIENTED_EDGE('',*,*,#14539,.F.);
#19537=ORIENTED_EDGE('',*,*,#14536,.F.);
#19538=ORIENTED_EDGE('',*,*,#14533,.F.);
#19539=ORIENTED_EDGE('',*,*,#14530,.F.);
#19540=ORIENTED_EDGE('',*,*,#14527,.F.);
#19541=ORIENTED_EDGE('',*,*,#14524,.F.);
#19542=ORIENTED_EDGE('',*,*,#14521,.F.);
#19543=ORIENTED_EDGE('',*,*,#14518,.F.);
#19544=ORIENTED_EDGE('',*,*,#14515,.F.);
#19545=ORIENTED_EDGE('',*,*,#14512,.F.);
#19546=ORIENTED_EDGE('',*,*,#14509,.F.);
#19547=ORIENTED_EDGE('',*,*,#14506,.F.);
#19548=ORIENTED_EDGE('',*,*,#14503,.F.);
#19549=ORIENTED_EDGE('',*,*,#14500,.F.);
#19550=ORIENTED_EDGE('',*,*,#14497,.F.);
#19551=ORIENTED_EDGE('',*,*,#14675,.F.);
#19552=ORIENTED_EDGE('',*,*,#14676,.T.);
#19553=ORIENTED_EDGE('',*,*,#14669,.T.);
#19554=ORIENTED_EDGE('',*,*,#14666,.T.);
#19555=ORIENTED_EDGE('',*,*,#14663,.T.);
#19556=ORIENTED_EDGE('',*,*,#14660,.T.);
#19557=ORIENTED_EDGE('',*,*,#14657,.T.);
#19558=ORIENTED_EDGE('',*,*,#14654,.T.);
#19559=ORIENTED_EDGE('',*,*,#14651,.T.);
#19560=ORIENTED_EDGE('',*,*,#14648,.T.);
#19561=ORIENTED_EDGE('',*,*,#14645,.T.);
#19562=ORIENTED_EDGE('',*,*,#14642,.T.);
#19563=ORIENTED_EDGE('',*,*,#14639,.T.);
#19564=ORIENTED_EDGE('',*,*,#14636,.T.);
#19565=ORIENTED_EDGE('',*,*,#14633,.T.);
#19566=ORIENTED_EDGE('',*,*,#14630,.T.);
#19567=ORIENTED_EDGE('',*,*,#14627,.T.);
#19568=ORIENTED_EDGE('',*,*,#14624,.T.);
#19569=ORIENTED_EDGE('',*,*,#14621,.T.);
#19570=ORIENTED_EDGE('',*,*,#14618,.T.);
#19571=ORIENTED_EDGE('',*,*,#14615,.T.);
#19572=ORIENTED_EDGE('',*,*,#14612,.T.);
#19573=ORIENTED_EDGE('',*,*,#14609,.T.);
#19574=ORIENTED_EDGE('',*,*,#14606,.T.);
#19575=ORIENTED_EDGE('',*,*,#14603,.T.);
#19576=ORIENTED_EDGE('',*,*,#14600,.T.);
#19577=ORIENTED_EDGE('',*,*,#14597,.T.);
#19578=ORIENTED_EDGE('',*,*,#14594,.T.);
#19579=ORIENTED_EDGE('',*,*,#14591,.T.);
#19580=ORIENTED_EDGE('',*,*,#14588,.T.);
#19581=ORIENTED_EDGE('',*,*,#14677,.T.);
#19582=ORIENTED_EDGE('',*,*,#14678,.T.);
#19583=ORIENTED_EDGE('',*,*,#14679,.T.);
#19584=ORIENTED_EDGE('',*,*,#14680,.T.);
#19585=ORIENTED_EDGE('',*,*,#14675,.T.);
#19586=ORIENTED_EDGE('',*,*,#14667,.T.);
#19587=ORIENTED_EDGE('',*,*,#14676,.F.);
#19588=ORIENTED_EDGE('',*,*,#14680,.F.);
#19589=ORIENTED_EDGE('',*,*,#14681,.T.);
#19590=ORIENTED_EDGE('',*,*,#14670,.F.);
#19591=ORIENTED_EDGE('',*,*,#14583,.F.);
#19592=ORIENTED_EDGE('',*,*,#14586,.F.);
#19593=ORIENTED_EDGE('',*,*,#14590,.F.);
#19594=ORIENTED_EDGE('',*,*,#14593,.F.);
#19595=ORIENTED_EDGE('',*,*,#14596,.F.);
#19596=ORIENTED_EDGE('',*,*,#14599,.F.);
#19597=ORIENTED_EDGE('',*,*,#14602,.F.);
#19598=ORIENTED_EDGE('',*,*,#14605,.F.);
#19599=ORIENTED_EDGE('',*,*,#14608,.F.);
#19600=ORIENTED_EDGE('',*,*,#14611,.F.);
#19601=ORIENTED_EDGE('',*,*,#14614,.F.);
#19602=ORIENTED_EDGE('',*,*,#14617,.F.);
#19603=ORIENTED_EDGE('',*,*,#14620,.F.);
#19604=ORIENTED_EDGE('',*,*,#14623,.F.);
#19605=ORIENTED_EDGE('',*,*,#14626,.F.);
#19606=ORIENTED_EDGE('',*,*,#14629,.F.);
#19607=ORIENTED_EDGE('',*,*,#14632,.F.);
#19608=ORIENTED_EDGE('',*,*,#14635,.F.);
#19609=ORIENTED_EDGE('',*,*,#14638,.F.);
#19610=ORIENTED_EDGE('',*,*,#14641,.F.);
#19611=ORIENTED_EDGE('',*,*,#14644,.F.);
#19612=ORIENTED_EDGE('',*,*,#14647,.F.);
#19613=ORIENTED_EDGE('',*,*,#14650,.F.);
#19614=ORIENTED_EDGE('',*,*,#14653,.F.);
#19615=ORIENTED_EDGE('',*,*,#14656,.F.);
#19616=ORIENTED_EDGE('',*,*,#14659,.F.);
#19617=ORIENTED_EDGE('',*,*,#14662,.F.);
#19618=ORIENTED_EDGE('',*,*,#14665,.F.);
#19619=ORIENTED_EDGE('',*,*,#14668,.F.);
#19620=ORIENTED_EDGE('',*,*,#14681,.F.);
#19621=ORIENTED_EDGE('',*,*,#14679,.F.);
#19622=ORIENTED_EDGE('',*,*,#14495,.F.);
#19623=ORIENTED_EDGE('',*,*,#14499,.F.);
#19624=ORIENTED_EDGE('',*,*,#14502,.F.);
#19625=ORIENTED_EDGE('',*,*,#14505,.F.);
#19626=ORIENTED_EDGE('',*,*,#14508,.F.);
#19627=ORIENTED_EDGE('',*,*,#14511,.F.);
#19628=ORIENTED_EDGE('',*,*,#14514,.F.);
#19629=ORIENTED_EDGE('',*,*,#14517,.F.);
#19630=ORIENTED_EDGE('',*,*,#14520,.F.);
#19631=ORIENTED_EDGE('',*,*,#14523,.F.);
#19632=ORIENTED_EDGE('',*,*,#14526,.F.);
#19633=ORIENTED_EDGE('',*,*,#14529,.F.);
#19634=ORIENTED_EDGE('',*,*,#14532,.F.);
#19635=ORIENTED_EDGE('',*,*,#14535,.F.);
#19636=ORIENTED_EDGE('',*,*,#14538,.F.);
#19637=ORIENTED_EDGE('',*,*,#14541,.F.);
#19638=ORIENTED_EDGE('',*,*,#14544,.F.);
#19639=ORIENTED_EDGE('',*,*,#14547,.F.);
#19640=ORIENTED_EDGE('',*,*,#14550,.F.);
#19641=ORIENTED_EDGE('',*,*,#14553,.F.);
#19642=ORIENTED_EDGE('',*,*,#14556,.F.);
#19643=ORIENTED_EDGE('',*,*,#14559,.F.);
#19644=ORIENTED_EDGE('',*,*,#14562,.F.);
#19645=ORIENTED_EDGE('',*,*,#14565,.F.);
#19646=ORIENTED_EDGE('',*,*,#14568,.F.);
#19647=ORIENTED_EDGE('',*,*,#14571,.F.);
#19648=ORIENTED_EDGE('',*,*,#14574,.F.);
#19649=ORIENTED_EDGE('',*,*,#14577,.F.);
#19650=ORIENTED_EDGE('',*,*,#14580,.F.);
#19651=ORIENTED_EDGE('',*,*,#14682,.F.);
#19652=ORIENTED_EDGE('',*,*,#14683,.F.);
#19653=ORIENTED_EDGE('',*,*,#14684,.F.);
#19654=ORIENTED_EDGE('',*,*,#14685,.F.);
#19655=ORIENTED_EDGE('',*,*,#14686,.F.);
#19656=ORIENTED_EDGE('',*,*,#14687,.F.);
#19657=ORIENTED_EDGE('',*,*,#14688,.F.);
#19658=ORIENTED_EDGE('',*,*,#14689,.F.);
#19659=ORIENTED_EDGE('',*,*,#14690,.F.);
#19660=ORIENTED_EDGE('',*,*,#14691,.F.);
#19661=ORIENTED_EDGE('',*,*,#14692,.F.);
#19662=ORIENTED_EDGE('',*,*,#14693,.F.);
#19663=ORIENTED_EDGE('',*,*,#14694,.F.);
#19664=ORIENTED_EDGE('',*,*,#14695,.T.);
#19665=ORIENTED_EDGE('',*,*,#14696,.F.);
#19666=ORIENTED_EDGE('',*,*,#14697,.F.);
#19667=ORIENTED_EDGE('',*,*,#14686,.T.);
#19668=ORIENTED_EDGE('',*,*,#14698,.F.);
#19669=ORIENTED_EDGE('',*,*,#14699,.F.);
#19670=ORIENTED_EDGE('',*,*,#14700,.F.);
#19671=ORIENTED_EDGE('',*,*,#14684,.T.);
#19672=ORIENTED_EDGE('',*,*,#14701,.F.);
#19673=ORIENTED_EDGE('',*,*,#14702,.F.);
#19674=ORIENTED_EDGE('',*,*,#14703,.F.);
#19675=ORIENTED_EDGE('',*,*,#14694,.T.);
#19676=ORIENTED_EDGE('',*,*,#14704,.F.);
#19677=ORIENTED_EDGE('',*,*,#14705,.F.);
#19678=ORIENTED_EDGE('',*,*,#14706,.F.);
#19679=ORIENTED_EDGE('',*,*,#14692,.T.);
#19680=ORIENTED_EDGE('',*,*,#14707,.F.);
#19681=ORIENTED_EDGE('',*,*,#14708,.F.);
#19682=ORIENTED_EDGE('',*,*,#14709,.F.);
#19683=ORIENTED_EDGE('',*,*,#14690,.T.);
#19684=ORIENTED_EDGE('',*,*,#14710,.F.);
#19685=ORIENTED_EDGE('',*,*,#14711,.F.);
#19686=ORIENTED_EDGE('',*,*,#14712,.F.);
#19687=ORIENTED_EDGE('',*,*,#14688,.T.);
#19688=ORIENTED_EDGE('',*,*,#14713,.F.);
#19689=ORIENTED_EDGE('',*,*,#14714,.F.);
#19690=ORIENTED_EDGE('',*,*,#14695,.F.);
#19691=ORIENTED_EDGE('',*,*,#14687,.T.);
#19692=ORIENTED_EDGE('',*,*,#14715,.F.);
#19693=ORIENTED_EDGE('',*,*,#14716,.F.);
#19694=ORIENTED_EDGE('',*,*,#14717,.T.);
#19695=ORIENTED_EDGE('',*,*,#14713,.T.);
#19696=ORIENTED_EDGE('',*,*,#14718,.T.);
#19697=ORIENTED_EDGE('',*,*,#14719,.T.);
#19698=ORIENTED_EDGE('',*,*,#14689,.T.);
#19699=ORIENTED_EDGE('',*,*,#14720,.F.);
#19700=ORIENTED_EDGE('',*,*,#14721,.F.);
#19701=ORIENTED_EDGE('',*,*,#14715,.T.);
#19702=ORIENTED_EDGE('',*,*,#14709,.T.);
#19703=ORIENTED_EDGE('',*,*,#14722,.T.);
#19704=ORIENTED_EDGE('',*,*,#14723,.F.);
#19705=ORIENTED_EDGE('',*,*,#14710,.T.);
#19706=ORIENTED_EDGE('',*,*,#14724,.T.);
#19707=ORIENTED_EDGE('',*,*,#14725,.T.);
#19708=ORIENTED_EDGE('',*,*,#14685,.T.);
#19709=ORIENTED_EDGE('',*,*,#14717,.F.);
#19710=ORIENTED_EDGE('',*,*,#14726,.F.);
#19711=ORIENTED_EDGE('',*,*,#14727,.T.);
#19712=ORIENTED_EDGE('',*,*,#14698,.T.);
#19713=ORIENTED_EDGE('',*,*,#14728,.T.);
#19714=ORIENTED_EDGE('',*,*,#14729,.T.);
#19715=ORIENTED_EDGE('',*,*,#14691,.T.);
#19716=ORIENTED_EDGE('',*,*,#14730,.F.);
#19717=ORIENTED_EDGE('',*,*,#14731,.F.);
#19718=ORIENTED_EDGE('',*,*,#14720,.T.);
#19719=ORIENTED_EDGE('',*,*,#14706,.T.);
#19720=ORIENTED_EDGE('',*,*,#14732,.T.);
#19721=ORIENTED_EDGE('',*,*,#14733,.F.);
#19722=ORIENTED_EDGE('',*,*,#14707,.T.);
#19723=ORIENTED_EDGE('',*,*,#14723,.T.);
#19724=ORIENTED_EDGE('',*,*,#14734,.T.);
#19725=ORIENTED_EDGE('',*,*,#14711,.T.);
#19726=ORIENTED_EDGE('',*,*,#14725,.F.);
#19727=ORIENTED_EDGE('',*,*,#14735,.F.);
#19728=ORIENTED_EDGE('',*,*,#14708,.T.);
#19729=ORIENTED_EDGE('',*,*,#14734,.F.);
#19730=ORIENTED_EDGE('',*,*,#14722,.F.);
#19731=ORIENTED_EDGE('',*,*,#14705,.T.);
#19732=ORIENTED_EDGE('',*,*,#14736,.F.);
#19733=ORIENTED_EDGE('',*,*,#14732,.F.);
#19734=ORIENTED_EDGE('',*,*,#14702,.T.);
#19735=ORIENTED_EDGE('',*,*,#14737,.F.);
#19736=ORIENTED_EDGE('',*,*,#14738,.F.);
#19737=ORIENTED_EDGE('',*,*,#14699,.T.);
#19738=ORIENTED_EDGE('',*,*,#14729,.F.);
#19739=ORIENTED_EDGE('',*,*,#14739,.F.);
#19740=ORIENTED_EDGE('',*,*,#14696,.T.);
#19741=ORIENTED_EDGE('',*,*,#14714,.T.);
#19742=ORIENTED_EDGE('',*,*,#14719,.F.);
#19743=ORIENTED_EDGE('',*,*,#14740,.F.);
#19744=ORIENTED_EDGE('',*,*,#14693,.T.);
#19745=ORIENTED_EDGE('',*,*,#14741,.F.);
#19746=ORIENTED_EDGE('',*,*,#14742,.F.);
#19747=ORIENTED_EDGE('',*,*,#14730,.T.);
#19748=ORIENTED_EDGE('',*,*,#14703,.T.);
#19749=ORIENTED_EDGE('',*,*,#14738,.T.);
#19750=ORIENTED_EDGE('',*,*,#14743,.F.);
#19751=ORIENTED_EDGE('',*,*,#14704,.T.);
#19752=ORIENTED_EDGE('',*,*,#14733,.T.);
#19753=ORIENTED_EDGE('',*,*,#14736,.T.);
#19754=ORIENTED_EDGE('',*,*,#14701,.T.);
#19755=ORIENTED_EDGE('',*,*,#14743,.T.);
#19756=ORIENTED_EDGE('',*,*,#14737,.T.);
#19757=ORIENTED_EDGE('',*,*,#14683,.T.);
#19758=ORIENTED_EDGE('',*,*,#14727,.F.);
#19759=ORIENTED_EDGE('',*,*,#14744,.F.);
#19760=ORIENTED_EDGE('',*,*,#14741,.T.);
#19761=ORIENTED_EDGE('',*,*,#14712,.T.);
#19762=ORIENTED_EDGE('',*,*,#14735,.T.);
#19763=ORIENTED_EDGE('',*,*,#14724,.F.);
#19764=ORIENTED_EDGE('',*,*,#14697,.T.);
#19765=ORIENTED_EDGE('',*,*,#14740,.T.);
#19766=ORIENTED_EDGE('',*,*,#14718,.F.);
#19767=ORIENTED_EDGE('',*,*,#14700,.T.);
#19768=ORIENTED_EDGE('',*,*,#14739,.T.);
#19769=ORIENTED_EDGE('',*,*,#14728,.F.);
#19770=ORIENTED_EDGE('',*,*,#14745,.F.);
#19771=ORIENTED_EDGE('',*,*,#14677,.F.);
#19772=ORIENTED_EDGE('',*,*,#14496,.F.);
#19773=ORIENTED_EDGE('',*,*,#14678,.F.);
#19774=ORIENTED_EDGE('',*,*,#14746,.T.);
#19775=ORIENTED_EDGE('',*,*,#14745,.T.);
#19776=ORIENTED_EDGE('',*,*,#14746,.F.);
#19777=ORIENTED_EDGE('',*,*,#14579,.T.);
#19778=ORIENTED_EDGE('',*,*,#14674,.T.);
#19779=ORIENTED_EDGE('',*,*,#14747,.F.);
#19780=ORIENTED_EDGE('',*,*,#14682,.T.);
#19781=ORIENTED_EDGE('',*,*,#14748,.F.);
#19782=ORIENTED_EDGE('',*,*,#14749,.T.);
#19783=ORIENTED_EDGE('',*,*,#14671,.T.);
#19784=ORIENTED_EDGE('',*,*,#14747,.T.);
#19785=ORIENTED_EDGE('',*,*,#14672,.T.);
#19786=ORIENTED_EDGE('',*,*,#14749,.F.);
#19787=ORIENTED_EDGE('',*,*,#14748,.T.);
#19788=ORIENTED_EDGE('',*,*,#14731,.T.);
#19789=ORIENTED_EDGE('',*,*,#14742,.T.);
#19790=ORIENTED_EDGE('',*,*,#14744,.T.);
#19791=ORIENTED_EDGE('',*,*,#14726,.T.);
#19792=ORIENTED_EDGE('',*,*,#14716,.T.);
#19793=ORIENTED_EDGE('',*,*,#14721,.T.);
#19794=ORIENTED_EDGE('',*,*,#14750,.T.);
#19795=ORIENTED_EDGE('',*,*,#14751,.T.);
#19796=ORIENTED_EDGE('',*,*,#14752,.T.);
#19797=ORIENTED_EDGE('',*,*,#14751,.F.);
#19798=ORIENTED_EDGE('',*,*,#14753,.F.);
#19799=ORIENTED_EDGE('',*,*,#14754,.T.);
#19800=ORIENTED_EDGE('',*,*,#14750,.F.);
#19801=ORIENTED_EDGE('',*,*,#14754,.F.);
#19802=ORIENTED_EDGE('',*,*,#14755,.T.);
#19803=ORIENTED_EDGE('',*,*,#14752,.F.);
#19804=ORIENTED_EDGE('',*,*,#14756,.T.);
#19805=ORIENTED_EDGE('',*,*,#14757,.T.);
#19806=ORIENTED_EDGE('',*,*,#14753,.T.);
#19807=ORIENTED_EDGE('',*,*,#14757,.F.);
#19808=ORIENTED_EDGE('',*,*,#14758,.T.);
#19809=ORIENTED_EDGE('',*,*,#14756,.F.);
#19810=ORIENTED_EDGE('',*,*,#14755,.F.);
#19811=ORIENTED_EDGE('',*,*,#14759,.T.);
#19812=ORIENTED_EDGE('',*,*,#14760,.F.);
#19813=ORIENTED_EDGE('',*,*,#14761,.F.);
#19814=ORIENTED_EDGE('',*,*,#14762,.F.);
#19815=ORIENTED_EDGE('',*,*,#14763,.F.);
#19816=ORIENTED_EDGE('',*,*,#14764,.F.);
#19817=ORIENTED_EDGE('',*,*,#14765,.F.);
#19818=ORIENTED_EDGE('',*,*,#14766,.F.);
#19819=ORIENTED_EDGE('',*,*,#14759,.F.);
#19820=ORIENTED_EDGE('',*,*,#14764,.T.);
#19821=ORIENTED_EDGE('',*,*,#14767,.T.);
#19822=ORIENTED_EDGE('',*,*,#14768,.T.);
#19823=ORIENTED_EDGE('',*,*,#14769,.F.);
#19824=ORIENTED_EDGE('',*,*,#14763,.T.);
#19825=ORIENTED_EDGE('',*,*,#14770,.T.);
#19826=ORIENTED_EDGE('',*,*,#14771,.T.);
#19827=ORIENTED_EDGE('',*,*,#14767,.F.);
#19828=ORIENTED_EDGE('',*,*,#14762,.T.);
#19829=ORIENTED_EDGE('',*,*,#14772,.T.);
#19830=ORIENTED_EDGE('',*,*,#14773,.T.);
#19831=ORIENTED_EDGE('',*,*,#14770,.F.);
#19832=ORIENTED_EDGE('',*,*,#14768,.F.);
#19833=ORIENTED_EDGE('',*,*,#14771,.F.);
#19834=ORIENTED_EDGE('',*,*,#14773,.F.);
#19835=ORIENTED_EDGE('',*,*,#14774,.F.);
#19836=ORIENTED_EDGE('',*,*,#14775,.F.);
#19837=ORIENTED_EDGE('',*,*,#14776,.T.);
#19838=ORIENTED_EDGE('',*,*,#14758,.F.);
#19839=ORIENTED_EDGE('',*,*,#14776,.F.);
#19840=ORIENTED_EDGE('',*,*,#14777,.F.);
#19841=ORIENTED_EDGE('',*,*,#14778,.F.);
#19842=ORIENTED_EDGE('',*,*,#14761,.T.);
#19843=ORIENTED_EDGE('',*,*,#14779,.T.);
#19844=ORIENTED_EDGE('',*,*,#14774,.T.);
#19845=ORIENTED_EDGE('',*,*,#14772,.F.);
#19846=ORIENTED_EDGE('',*,*,#14765,.T.);
#19847=ORIENTED_EDGE('',*,*,#14769,.T.);
#19848=ORIENTED_EDGE('',*,*,#14778,.T.);
#19849=ORIENTED_EDGE('',*,*,#14780,.F.);
#19850=ORIENTED_EDGE('',*,*,#14760,.T.);
#19851=ORIENTED_EDGE('',*,*,#14766,.T.);
#19852=ORIENTED_EDGE('',*,*,#14780,.T.);
#19853=ORIENTED_EDGE('',*,*,#14777,.T.);
#19854=ORIENTED_EDGE('',*,*,#14775,.T.);
#19855=ORIENTED_EDGE('',*,*,#14779,.F.);
#19856=ORIENTED_EDGE('',*,*,#14781,.F.);
#19857=ORIENTED_EDGE('',*,*,#14782,.T.);
#19858=ORIENTED_EDGE('',*,*,#14783,.T.);
#19859=ORIENTED_EDGE('',*,*,#14784,.T.);
#19860=ORIENTED_EDGE('',*,*,#14785,.F.);
#19861=ORIENTED_EDGE('',*,*,#14786,.T.);
#19862=ORIENTED_EDGE('',*,*,#14781,.T.);
#19863=ORIENTED_EDGE('',*,*,#14787,.T.);
#19864=ORIENTED_EDGE('',*,*,#14788,.F.);
#19865=ORIENTED_EDGE('',*,*,#14789,.T.);
#19866=ORIENTED_EDGE('',*,*,#14785,.T.);
#19867=ORIENTED_EDGE('',*,*,#14790,.T.);
#19868=ORIENTED_EDGE('',*,*,#14791,.F.);
#19869=ORIENTED_EDGE('',*,*,#14792,.T.);
#19870=ORIENTED_EDGE('',*,*,#14788,.T.);
#19871=ORIENTED_EDGE('',*,*,#14793,.T.);
#19872=ORIENTED_EDGE('',*,*,#14794,.F.);
#19873=ORIENTED_EDGE('',*,*,#14795,.T.);
#19874=ORIENTED_EDGE('',*,*,#14791,.T.);
#19875=ORIENTED_EDGE('',*,*,#14796,.T.);
#19876=ORIENTED_EDGE('',*,*,#14797,.F.);
#19877=ORIENTED_EDGE('',*,*,#14798,.T.);
#19878=ORIENTED_EDGE('',*,*,#14794,.T.);
#19879=ORIENTED_EDGE('',*,*,#14799,.T.);
#19880=ORIENTED_EDGE('',*,*,#14800,.F.);
#19881=ORIENTED_EDGE('',*,*,#14801,.T.);
#19882=ORIENTED_EDGE('',*,*,#14797,.T.);
#19883=ORIENTED_EDGE('',*,*,#14802,.T.);
#19884=ORIENTED_EDGE('',*,*,#14803,.F.);
#19885=ORIENTED_EDGE('',*,*,#14804,.T.);
#19886=ORIENTED_EDGE('',*,*,#14800,.T.);
#19887=ORIENTED_EDGE('',*,*,#14805,.T.);
#19888=ORIENTED_EDGE('',*,*,#14806,.F.);
#19889=ORIENTED_EDGE('',*,*,#14807,.T.);
#19890=ORIENTED_EDGE('',*,*,#14803,.T.);
#19891=ORIENTED_EDGE('',*,*,#14808,.T.);
#19892=ORIENTED_EDGE('',*,*,#14809,.F.);
#19893=ORIENTED_EDGE('',*,*,#14810,.T.);
#19894=ORIENTED_EDGE('',*,*,#14806,.T.);
#19895=ORIENTED_EDGE('',*,*,#14811,.T.);
#19896=ORIENTED_EDGE('',*,*,#14812,.F.);
#19897=ORIENTED_EDGE('',*,*,#14813,.T.);
#19898=ORIENTED_EDGE('',*,*,#14809,.T.);
#19899=ORIENTED_EDGE('',*,*,#14814,.T.);
#19900=ORIENTED_EDGE('',*,*,#14815,.F.);
#19901=ORIENTED_EDGE('',*,*,#14816,.T.);
#19902=ORIENTED_EDGE('',*,*,#14812,.T.);
#19903=ORIENTED_EDGE('',*,*,#14817,.T.);
#19904=ORIENTED_EDGE('',*,*,#14818,.F.);
#19905=ORIENTED_EDGE('',*,*,#14819,.T.);
#19906=ORIENTED_EDGE('',*,*,#14815,.T.);
#19907=ORIENTED_EDGE('',*,*,#14820,.T.);
#19908=ORIENTED_EDGE('',*,*,#14821,.F.);
#19909=ORIENTED_EDGE('',*,*,#14822,.T.);
#19910=ORIENTED_EDGE('',*,*,#14818,.T.);
#19911=ORIENTED_EDGE('',*,*,#14823,.T.);
#19912=ORIENTED_EDGE('',*,*,#14824,.F.);
#19913=ORIENTED_EDGE('',*,*,#14825,.T.);
#19914=ORIENTED_EDGE('',*,*,#14821,.T.);
#19915=ORIENTED_EDGE('',*,*,#14826,.T.);
#19916=ORIENTED_EDGE('',*,*,#14827,.F.);
#19917=ORIENTED_EDGE('',*,*,#14828,.T.);
#19918=ORIENTED_EDGE('',*,*,#14824,.T.);
#19919=ORIENTED_EDGE('',*,*,#14829,.T.);
#19920=ORIENTED_EDGE('',*,*,#14830,.F.);
#19921=ORIENTED_EDGE('',*,*,#14831,.T.);
#19922=ORIENTED_EDGE('',*,*,#14827,.T.);
#19923=ORIENTED_EDGE('',*,*,#14832,.T.);
#19924=ORIENTED_EDGE('',*,*,#14833,.F.);
#19925=ORIENTED_EDGE('',*,*,#14834,.T.);
#19926=ORIENTED_EDGE('',*,*,#14830,.T.);
#19927=ORIENTED_EDGE('',*,*,#14835,.T.);
#19928=ORIENTED_EDGE('',*,*,#14836,.F.);
#19929=ORIENTED_EDGE('',*,*,#14837,.T.);
#19930=ORIENTED_EDGE('',*,*,#14833,.T.);
#19931=ORIENTED_EDGE('',*,*,#14838,.T.);
#19932=ORIENTED_EDGE('',*,*,#14839,.F.);
#19933=ORIENTED_EDGE('',*,*,#14840,.T.);
#19934=ORIENTED_EDGE('',*,*,#14841,.F.);
#19935=ORIENTED_EDGE('',*,*,#14842,.F.);
#19936=ORIENTED_EDGE('',*,*,#14843,.T.);
#19937=ORIENTED_EDGE('',*,*,#14839,.T.);
#19938=ORIENTED_EDGE('',*,*,#14844,.F.);
#19939=ORIENTED_EDGE('',*,*,#14845,.F.);
#19940=ORIENTED_EDGE('',*,*,#14846,.F.);
#19941=ORIENTED_EDGE('',*,*,#14847,.T.);
#19942=ORIENTED_EDGE('',*,*,#14842,.T.);
#19943=ORIENTED_EDGE('',*,*,#14848,.F.);
#19944=ORIENTED_EDGE('',*,*,#14849,.F.);
#19945=ORIENTED_EDGE('',*,*,#14850,.T.);
#19946=ORIENTED_EDGE('',*,*,#14846,.T.);
#19947=ORIENTED_EDGE('',*,*,#14851,.F.);
#19948=ORIENTED_EDGE('',*,*,#14852,.F.);
#19949=ORIENTED_EDGE('',*,*,#14853,.T.);
#19950=ORIENTED_EDGE('',*,*,#14849,.T.);
#19951=ORIENTED_EDGE('',*,*,#14854,.F.);
#19952=ORIENTED_EDGE('',*,*,#14855,.F.);
#19953=ORIENTED_EDGE('',*,*,#14856,.T.);
#19954=ORIENTED_EDGE('',*,*,#14852,.T.);
#19955=ORIENTED_EDGE('',*,*,#14857,.F.);
#19956=ORIENTED_EDGE('',*,*,#14858,.F.);
#19957=ORIENTED_EDGE('',*,*,#14859,.T.);
#19958=ORIENTED_EDGE('',*,*,#14855,.T.);
#19959=ORIENTED_EDGE('',*,*,#14860,.F.);
#19960=ORIENTED_EDGE('',*,*,#14861,.F.);
#19961=ORIENTED_EDGE('',*,*,#14862,.T.);
#19962=ORIENTED_EDGE('',*,*,#14858,.T.);
#19963=ORIENTED_EDGE('',*,*,#14863,.F.);
#19964=ORIENTED_EDGE('',*,*,#14864,.F.);
#19965=ORIENTED_EDGE('',*,*,#14865,.T.);
#19966=ORIENTED_EDGE('',*,*,#14861,.T.);
#19967=ORIENTED_EDGE('',*,*,#14866,.F.);
#19968=ORIENTED_EDGE('',*,*,#14867,.F.);
#19969=ORIENTED_EDGE('',*,*,#14868,.T.);
#19970=ORIENTED_EDGE('',*,*,#14864,.T.);
#19971=ORIENTED_EDGE('',*,*,#14869,.F.);
#19972=ORIENTED_EDGE('',*,*,#14870,.F.);
#19973=ORIENTED_EDGE('',*,*,#14871,.T.);
#19974=ORIENTED_EDGE('',*,*,#14867,.T.);
#19975=ORIENTED_EDGE('',*,*,#14872,.F.);
#19976=ORIENTED_EDGE('',*,*,#14873,.F.);
#19977=ORIENTED_EDGE('',*,*,#14874,.T.);
#19978=ORIENTED_EDGE('',*,*,#14870,.T.);
#19979=ORIENTED_EDGE('',*,*,#14875,.F.);
#19980=ORIENTED_EDGE('',*,*,#14876,.F.);
#19981=ORIENTED_EDGE('',*,*,#14877,.T.);
#19982=ORIENTED_EDGE('',*,*,#14873,.T.);
#19983=ORIENTED_EDGE('',*,*,#14878,.F.);
#19984=ORIENTED_EDGE('',*,*,#14879,.F.);
#19985=ORIENTED_EDGE('',*,*,#14880,.T.);
#19986=ORIENTED_EDGE('',*,*,#14876,.T.);
#19987=ORIENTED_EDGE('',*,*,#14881,.F.);
#19988=ORIENTED_EDGE('',*,*,#14882,.F.);
#19989=ORIENTED_EDGE('',*,*,#14883,.T.);
#19990=ORIENTED_EDGE('',*,*,#14879,.T.);
#19991=ORIENTED_EDGE('',*,*,#14884,.F.);
#19992=ORIENTED_EDGE('',*,*,#14885,.F.);
#19993=ORIENTED_EDGE('',*,*,#14886,.T.);
#19994=ORIENTED_EDGE('',*,*,#14882,.T.);
#19995=ORIENTED_EDGE('',*,*,#14887,.F.);
#19996=ORIENTED_EDGE('',*,*,#14888,.F.);
#19997=ORIENTED_EDGE('',*,*,#14889,.T.);
#19998=ORIENTED_EDGE('',*,*,#14885,.T.);
#19999=ORIENTED_EDGE('',*,*,#14890,.F.);
#20000=ORIENTED_EDGE('',*,*,#14891,.F.);
#20001=ORIENTED_EDGE('',*,*,#14892,.T.);
#20002=ORIENTED_EDGE('',*,*,#14888,.T.);
#20003=ORIENTED_EDGE('',*,*,#14893,.F.);
#20004=ORIENTED_EDGE('',*,*,#14894,.F.);
#20005=ORIENTED_EDGE('',*,*,#14895,.T.);
#20006=ORIENTED_EDGE('',*,*,#14891,.T.);
#20007=ORIENTED_EDGE('',*,*,#14896,.F.);
#20008=ORIENTED_EDGE('',*,*,#14844,.T.);
#20009=ORIENTED_EDGE('',*,*,#14841,.T.);
#20010=ORIENTED_EDGE('',*,*,#14897,.T.);
#20011=ORIENTED_EDGE('',*,*,#14898,.F.);
#20012=ORIENTED_EDGE('',*,*,#14899,.F.);
#20013=ORIENTED_EDGE('',*,*,#14900,.T.);
#20014=ORIENTED_EDGE('',*,*,#14900,.F.);
#20015=ORIENTED_EDGE('',*,*,#14901,.F.);
#20016=ORIENTED_EDGE('',*,*,#14838,.F.);
#20017=ORIENTED_EDGE('',*,*,#14835,.F.);
#20018=ORIENTED_EDGE('',*,*,#14832,.F.);
#20019=ORIENTED_EDGE('',*,*,#14829,.F.);
#20020=ORIENTED_EDGE('',*,*,#14826,.F.);
#20021=ORIENTED_EDGE('',*,*,#14823,.F.);
#20022=ORIENTED_EDGE('',*,*,#14820,.F.);
#20023=ORIENTED_EDGE('',*,*,#14817,.F.);
#20024=ORIENTED_EDGE('',*,*,#14814,.F.);
#20025=ORIENTED_EDGE('',*,*,#14811,.F.);
#20026=ORIENTED_EDGE('',*,*,#14808,.F.);
#20027=ORIENTED_EDGE('',*,*,#14805,.F.);
#20028=ORIENTED_EDGE('',*,*,#14802,.F.);
#20029=ORIENTED_EDGE('',*,*,#14799,.F.);
#20030=ORIENTED_EDGE('',*,*,#14796,.F.);
#20031=ORIENTED_EDGE('',*,*,#14793,.F.);
#20032=ORIENTED_EDGE('',*,*,#14790,.F.);
#20033=ORIENTED_EDGE('',*,*,#14787,.F.);
#20034=ORIENTED_EDGE('',*,*,#14784,.F.);
#20035=ORIENTED_EDGE('',*,*,#14902,.F.);
#20036=ORIENTED_EDGE('',*,*,#14903,.T.);
#20037=ORIENTED_EDGE('',*,*,#14896,.T.);
#20038=ORIENTED_EDGE('',*,*,#14893,.T.);
#20039=ORIENTED_EDGE('',*,*,#14890,.T.);
#20040=ORIENTED_EDGE('',*,*,#14887,.T.);
#20041=ORIENTED_EDGE('',*,*,#14884,.T.);
#20042=ORIENTED_EDGE('',*,*,#14881,.T.);
#20043=ORIENTED_EDGE('',*,*,#14878,.T.);
#20044=ORIENTED_EDGE('',*,*,#14875,.T.);
#20045=ORIENTED_EDGE('',*,*,#14872,.T.);
#20046=ORIENTED_EDGE('',*,*,#14869,.T.);
#20047=ORIENTED_EDGE('',*,*,#14866,.T.);
#20048=ORIENTED_EDGE('',*,*,#14863,.T.);
#20049=ORIENTED_EDGE('',*,*,#14860,.T.);
#20050=ORIENTED_EDGE('',*,*,#14857,.T.);
#20051=ORIENTED_EDGE('',*,*,#14854,.T.);
#20052=ORIENTED_EDGE('',*,*,#14851,.T.);
#20053=ORIENTED_EDGE('',*,*,#14848,.T.);
#20054=ORIENTED_EDGE('',*,*,#14845,.T.);
#20055=ORIENTED_EDGE('',*,*,#14904,.T.);
#20056=ORIENTED_EDGE('',*,*,#14905,.T.);
#20057=ORIENTED_EDGE('',*,*,#14906,.T.);
#20058=ORIENTED_EDGE('',*,*,#14907,.T.);
#20059=ORIENTED_EDGE('',*,*,#14902,.T.);
#20060=ORIENTED_EDGE('',*,*,#14894,.T.);
#20061=ORIENTED_EDGE('',*,*,#14903,.F.);
#20062=ORIENTED_EDGE('',*,*,#14907,.F.);
#20063=ORIENTED_EDGE('',*,*,#14908,.T.);
#20064=ORIENTED_EDGE('',*,*,#14897,.F.);
#20065=ORIENTED_EDGE('',*,*,#14840,.F.);
#20066=ORIENTED_EDGE('',*,*,#14843,.F.);
#20067=ORIENTED_EDGE('',*,*,#14847,.F.);
#20068=ORIENTED_EDGE('',*,*,#14850,.F.);
#20069=ORIENTED_EDGE('',*,*,#14853,.F.);
#20070=ORIENTED_EDGE('',*,*,#14856,.F.);
#20071=ORIENTED_EDGE('',*,*,#14859,.F.);
#20072=ORIENTED_EDGE('',*,*,#14862,.F.);
#20073=ORIENTED_EDGE('',*,*,#14865,.F.);
#20074=ORIENTED_EDGE('',*,*,#14868,.F.);
#20075=ORIENTED_EDGE('',*,*,#14871,.F.);
#20076=ORIENTED_EDGE('',*,*,#14874,.F.);
#20077=ORIENTED_EDGE('',*,*,#14877,.F.);
#20078=ORIENTED_EDGE('',*,*,#14880,.F.);
#20079=ORIENTED_EDGE('',*,*,#14883,.F.);
#20080=ORIENTED_EDGE('',*,*,#14886,.F.);
#20081=ORIENTED_EDGE('',*,*,#14889,.F.);
#20082=ORIENTED_EDGE('',*,*,#14892,.F.);
#20083=ORIENTED_EDGE('',*,*,#14895,.F.);
#20084=ORIENTED_EDGE('',*,*,#14908,.F.);
#20085=ORIENTED_EDGE('',*,*,#14906,.F.);
#20086=ORIENTED_EDGE('',*,*,#14782,.F.);
#20087=ORIENTED_EDGE('',*,*,#14786,.F.);
#20088=ORIENTED_EDGE('',*,*,#14789,.F.);
#20089=ORIENTED_EDGE('',*,*,#14792,.F.);
#20090=ORIENTED_EDGE('',*,*,#14795,.F.);
#20091=ORIENTED_EDGE('',*,*,#14798,.F.);
#20092=ORIENTED_EDGE('',*,*,#14801,.F.);
#20093=ORIENTED_EDGE('',*,*,#14804,.F.);
#20094=ORIENTED_EDGE('',*,*,#14807,.F.);
#20095=ORIENTED_EDGE('',*,*,#14810,.F.);
#20096=ORIENTED_EDGE('',*,*,#14813,.F.);
#20097=ORIENTED_EDGE('',*,*,#14816,.F.);
#20098=ORIENTED_EDGE('',*,*,#14819,.F.);
#20099=ORIENTED_EDGE('',*,*,#14822,.F.);
#20100=ORIENTED_EDGE('',*,*,#14825,.F.);
#20101=ORIENTED_EDGE('',*,*,#14828,.F.);
#20102=ORIENTED_EDGE('',*,*,#14831,.F.);
#20103=ORIENTED_EDGE('',*,*,#14834,.F.);
#20104=ORIENTED_EDGE('',*,*,#14837,.F.);
#20105=ORIENTED_EDGE('',*,*,#14909,.F.);
#20106=ORIENTED_EDGE('',*,*,#14910,.F.);
#20107=ORIENTED_EDGE('',*,*,#14911,.F.);
#20108=ORIENTED_EDGE('',*,*,#14912,.F.);
#20109=ORIENTED_EDGE('',*,*,#14913,.F.);
#20110=ORIENTED_EDGE('',*,*,#14914,.F.);
#20111=ORIENTED_EDGE('',*,*,#14915,.F.);
#20112=ORIENTED_EDGE('',*,*,#14916,.F.);
#20113=ORIENTED_EDGE('',*,*,#14917,.F.);
#20114=ORIENTED_EDGE('',*,*,#14918,.F.);
#20115=ORIENTED_EDGE('',*,*,#14919,.F.);
#20116=ORIENTED_EDGE('',*,*,#14920,.F.);
#20117=ORIENTED_EDGE('',*,*,#14921,.F.);
#20118=ORIENTED_EDGE('',*,*,#14922,.T.);
#20119=ORIENTED_EDGE('',*,*,#14923,.F.);
#20120=ORIENTED_EDGE('',*,*,#14924,.F.);
#20121=ORIENTED_EDGE('',*,*,#14913,.T.);
#20122=ORIENTED_EDGE('',*,*,#14925,.F.);
#20123=ORIENTED_EDGE('',*,*,#14926,.F.);
#20124=ORIENTED_EDGE('',*,*,#14927,.F.);
#20125=ORIENTED_EDGE('',*,*,#14911,.T.);
#20126=ORIENTED_EDGE('',*,*,#14928,.F.);
#20127=ORIENTED_EDGE('',*,*,#14929,.F.);
#20128=ORIENTED_EDGE('',*,*,#14930,.F.);
#20129=ORIENTED_EDGE('',*,*,#14921,.T.);
#20130=ORIENTED_EDGE('',*,*,#14931,.F.);
#20131=ORIENTED_EDGE('',*,*,#14932,.F.);
#20132=ORIENTED_EDGE('',*,*,#14933,.F.);
#20133=ORIENTED_EDGE('',*,*,#14919,.T.);
#20134=ORIENTED_EDGE('',*,*,#14934,.F.);
#20135=ORIENTED_EDGE('',*,*,#14935,.F.);
#20136=ORIENTED_EDGE('',*,*,#14936,.F.);
#20137=ORIENTED_EDGE('',*,*,#14917,.T.);
#20138=ORIENTED_EDGE('',*,*,#14937,.F.);
#20139=ORIENTED_EDGE('',*,*,#14938,.F.);
#20140=ORIENTED_EDGE('',*,*,#14939,.F.);
#20141=ORIENTED_EDGE('',*,*,#14915,.T.);
#20142=ORIENTED_EDGE('',*,*,#14940,.F.);
#20143=ORIENTED_EDGE('',*,*,#14941,.F.);
#20144=ORIENTED_EDGE('',*,*,#14922,.F.);
#20145=ORIENTED_EDGE('',*,*,#14914,.T.);
#20146=ORIENTED_EDGE('',*,*,#14942,.F.);
#20147=ORIENTED_EDGE('',*,*,#14943,.F.);
#20148=ORIENTED_EDGE('',*,*,#14944,.T.);
#20149=ORIENTED_EDGE('',*,*,#14940,.T.);
#20150=ORIENTED_EDGE('',*,*,#14945,.T.);
#20151=ORIENTED_EDGE('',*,*,#14946,.T.);
#20152=ORIENTED_EDGE('',*,*,#14916,.T.);
#20153=ORIENTED_EDGE('',*,*,#14947,.F.);
#20154=ORIENTED_EDGE('',*,*,#14948,.F.);
#20155=ORIENTED_EDGE('',*,*,#14942,.T.);
#20156=ORIENTED_EDGE('',*,*,#14936,.T.);
#20157=ORIENTED_EDGE('',*,*,#14949,.T.);
#20158=ORIENTED_EDGE('',*,*,#14950,.F.);
#20159=ORIENTED_EDGE('',*,*,#14937,.T.);
#20160=ORIENTED_EDGE('',*,*,#14951,.T.);
#20161=ORIENTED_EDGE('',*,*,#14952,.T.);
#20162=ORIENTED_EDGE('',*,*,#14912,.T.);
#20163=ORIENTED_EDGE('',*,*,#14944,.F.);
#20164=ORIENTED_EDGE('',*,*,#14953,.F.);
#20165=ORIENTED_EDGE('',*,*,#14954,.T.);
#20166=ORIENTED_EDGE('',*,*,#14925,.T.);
#20167=ORIENTED_EDGE('',*,*,#14955,.T.);
#20168=ORIENTED_EDGE('',*,*,#14956,.T.);
#20169=ORIENTED_EDGE('',*,*,#14918,.T.);
#20170=ORIENTED_EDGE('',*,*,#14957,.F.);
#20171=ORIENTED_EDGE('',*,*,#14958,.F.);
#20172=ORIENTED_EDGE('',*,*,#14947,.T.);
#20173=ORIENTED_EDGE('',*,*,#14933,.T.);
#20174=ORIENTED_EDGE('',*,*,#14959,.T.);
#20175=ORIENTED_EDGE('',*,*,#14960,.F.);
#20176=ORIENTED_EDGE('',*,*,#14934,.T.);
#20177=ORIENTED_EDGE('',*,*,#14950,.T.);
#20178=ORIENTED_EDGE('',*,*,#14961,.T.);
#20179=ORIENTED_EDGE('',*,*,#14938,.T.);
#20180=ORIENTED_EDGE('',*,*,#14952,.F.);
#20181=ORIENTED_EDGE('',*,*,#14962,.F.);
#20182=ORIENTED_EDGE('',*,*,#14935,.T.);
#20183=ORIENTED_EDGE('',*,*,#14961,.F.);
#20184=ORIENTED_EDGE('',*,*,#14949,.F.);
#20185=ORIENTED_EDGE('',*,*,#14932,.T.);
#20186=ORIENTED_EDGE('',*,*,#14963,.F.);
#20187=ORIENTED_EDGE('',*,*,#14959,.F.);
#20188=ORIENTED_EDGE('',*,*,#14929,.T.);
#20189=ORIENTED_EDGE('',*,*,#14964,.F.);
#20190=ORIENTED_EDGE('',*,*,#14965,.F.);
#20191=ORIENTED_EDGE('',*,*,#14926,.T.);
#20192=ORIENTED_EDGE('',*,*,#14956,.F.);
#20193=ORIENTED_EDGE('',*,*,#14966,.F.);
#20194=ORIENTED_EDGE('',*,*,#14923,.T.);
#20195=ORIENTED_EDGE('',*,*,#14941,.T.);
#20196=ORIENTED_EDGE('',*,*,#14946,.F.);
#20197=ORIENTED_EDGE('',*,*,#14967,.F.);
#20198=ORIENTED_EDGE('',*,*,#14920,.T.);
#20199=ORIENTED_EDGE('',*,*,#14968,.F.);
#20200=ORIENTED_EDGE('',*,*,#14969,.F.);
#20201=ORIENTED_EDGE('',*,*,#14957,.T.);
#20202=ORIENTED_EDGE('',*,*,#14930,.T.);
#20203=ORIENTED_EDGE('',*,*,#14965,.T.);
#20204=ORIENTED_EDGE('',*,*,#14970,.F.);
#20205=ORIENTED_EDGE('',*,*,#14931,.T.);
#20206=ORIENTED_EDGE('',*,*,#14960,.T.);
#20207=ORIENTED_EDGE('',*,*,#14963,.T.);
#20208=ORIENTED_EDGE('',*,*,#14928,.T.);
#20209=ORIENTED_EDGE('',*,*,#14970,.T.);
#20210=ORIENTED_EDGE('',*,*,#14964,.T.);
#20211=ORIENTED_EDGE('',*,*,#14910,.T.);
#20212=ORIENTED_EDGE('',*,*,#14954,.F.);
#20213=ORIENTED_EDGE('',*,*,#14971,.F.);
#20214=ORIENTED_EDGE('',*,*,#14968,.T.);
#20215=ORIENTED_EDGE('',*,*,#14939,.T.);
#20216=ORIENTED_EDGE('',*,*,#14962,.T.);
#20217=ORIENTED_EDGE('',*,*,#14951,.F.);
#20218=ORIENTED_EDGE('',*,*,#14924,.T.);
#20219=ORIENTED_EDGE('',*,*,#14967,.T.);
#20220=ORIENTED_EDGE('',*,*,#14945,.F.);
#20221=ORIENTED_EDGE('',*,*,#14927,.T.);
#20222=ORIENTED_EDGE('',*,*,#14966,.T.);
#20223=ORIENTED_EDGE('',*,*,#14955,.F.);
#20224=ORIENTED_EDGE('',*,*,#14972,.F.);
#20225=ORIENTED_EDGE('',*,*,#14904,.F.);
#20226=ORIENTED_EDGE('',*,*,#14783,.F.);
#20227=ORIENTED_EDGE('',*,*,#14905,.F.);
#20228=ORIENTED_EDGE('',*,*,#14973,.T.);
#20229=ORIENTED_EDGE('',*,*,#14972,.T.);
#20230=ORIENTED_EDGE('',*,*,#14973,.F.);
#20231=ORIENTED_EDGE('',*,*,#14836,.T.);
#20232=ORIENTED_EDGE('',*,*,#14901,.T.);
#20233=ORIENTED_EDGE('',*,*,#14974,.F.);
#20234=ORIENTED_EDGE('',*,*,#14909,.T.);
#20235=ORIENTED_EDGE('',*,*,#14975,.F.);
#20236=ORIENTED_EDGE('',*,*,#14976,.T.);
#20237=ORIENTED_EDGE('',*,*,#14898,.T.);
#20238=ORIENTED_EDGE('',*,*,#14974,.T.);
#20239=ORIENTED_EDGE('',*,*,#14899,.T.);
#20240=ORIENTED_EDGE('',*,*,#14976,.F.);
#20241=ORIENTED_EDGE('',*,*,#14975,.T.);
#20242=ORIENTED_EDGE('',*,*,#14958,.T.);
#20243=ORIENTED_EDGE('',*,*,#14969,.T.);
#20244=ORIENTED_EDGE('',*,*,#14971,.T.);
#20245=ORIENTED_EDGE('',*,*,#14953,.T.);
#20246=ORIENTED_EDGE('',*,*,#14943,.T.);
#20247=ORIENTED_EDGE('',*,*,#14948,.T.);
#20248=ORIENTED_EDGE('',*,*,#14977,.T.);
#20249=ORIENTED_EDGE('',*,*,#14978,.T.);
#20250=ORIENTED_EDGE('',*,*,#14977,.F.);
#20251=ORIENTED_EDGE('',*,*,#14979,.T.);
#20252=ORIENTED_EDGE('',*,*,#14980,.F.);
#20253=ORIENTED_EDGE('',*,*,#14981,.T.);
#20254=ORIENTED_EDGE('',*,*,#14982,.T.);
#20255=ORIENTED_EDGE('',*,*,#14981,.F.);
#20256=ORIENTED_EDGE('',*,*,#14983,.F.);
#20257=ORIENTED_EDGE('',*,*,#14984,.F.);
#20258=ORIENTED_EDGE('',*,*,#14979,.F.);
#20259=ORIENTED_EDGE('',*,*,#14978,.F.);
#20260=ORIENTED_EDGE('',*,*,#14985,.T.);
#20261=ORIENTED_EDGE('',*,*,#14986,.F.);
#20262=ORIENTED_EDGE('',*,*,#14985,.F.);
#20263=ORIENTED_EDGE('',*,*,#14987,.T.);
#20264=ORIENTED_EDGE('',*,*,#14988,.F.);
#20265=ORIENTED_EDGE('',*,*,#14989,.T.);
#20266=ORIENTED_EDGE('',*,*,#14990,.F.);
#20267=ORIENTED_EDGE('',*,*,#14991,.T.);
#20268=ORIENTED_EDGE('',*,*,#14986,.T.);
#20269=ORIENTED_EDGE('',*,*,#14991,.F.);
#20270=ORIENTED_EDGE('',*,*,#14983,.T.);
#20271=ORIENTED_EDGE('',*,*,#14992,.T.);
#20272=ORIENTED_EDGE('',*,*,#14993,.T.);
#20273=ORIENTED_EDGE('',*,*,#14994,.T.);
#20274=ORIENTED_EDGE('',*,*,#14993,.F.);
#20275=ORIENTED_EDGE('',*,*,#14995,.F.);
#20276=ORIENTED_EDGE('',*,*,#14996,.F.);
#20277=ORIENTED_EDGE('',*,*,#14997,.F.);
#20278=ORIENTED_EDGE('',*,*,#14998,.F.);
#20279=ORIENTED_EDGE('',*,*,#14999,.T.);
#20280=ORIENTED_EDGE('',*,*,#14994,.F.);
#20281=ORIENTED_EDGE('',*,*,#14999,.F.);
#20282=ORIENTED_EDGE('',*,*,#15000,.F.);
#20283=ORIENTED_EDGE('',*,*,#15001,.T.);
#20284=ORIENTED_EDGE('',*,*,#14992,.F.);
#20285=ORIENTED_EDGE('',*,*,#15002,.T.);
#20286=ORIENTED_EDGE('',*,*,#14995,.T.);
#20287=ORIENTED_EDGE('',*,*,#15003,.T.);
#20288=ORIENTED_EDGE('',*,*,#14990,.T.);
#20289=ORIENTED_EDGE('',*,*,#15004,.T.);
#20290=ORIENTED_EDGE('',*,*,#14997,.T.);
#20291=ORIENTED_EDGE('',*,*,#15005,.T.);
#20292=ORIENTED_EDGE('',*,*,#14988,.T.);
#20293=ORIENTED_EDGE('',*,*,#15006,.T.);
#20294=ORIENTED_EDGE('',*,*,#15007,.T.);
#20295=ORIENTED_EDGE('',*,*,#15008,.T.);
#20296=ORIENTED_EDGE('',*,*,#15006,.F.);
#20297=ORIENTED_EDGE('',*,*,#15009,.T.);
#20298=ORIENTED_EDGE('',*,*,#15010,.T.);
#20299=ORIENTED_EDGE('',*,*,#15011,.T.);
#20300=ORIENTED_EDGE('',*,*,#15012,.F.);
#20301=ORIENTED_EDGE('',*,*,#15013,.T.);
#20302=ORIENTED_EDGE('',*,*,#15007,.F.);
#20303=ORIENTED_EDGE('',*,*,#15008,.F.);
#20304=ORIENTED_EDGE('',*,*,#15013,.F.);
#20305=ORIENTED_EDGE('',*,*,#15014,.T.);
#20306=ORIENTED_EDGE('',*,*,#15015,.T.);
#20307=ORIENTED_EDGE('',*,*,#15016,.F.);
#20308=ORIENTED_EDGE('',*,*,#15015,.F.);
#20309=ORIENTED_EDGE('',*,*,#15011,.F.);
#20310=ORIENTED_EDGE('',*,*,#15010,.F.);
#20311=ORIENTED_EDGE('',*,*,#15009,.F.);
#20312=ORIENTED_EDGE('',*,*,#15017,.T.);
#20313=ORIENTED_EDGE('',*,*,#15012,.T.);
#20314=ORIENTED_EDGE('',*,*,#15017,.F.);
#20315=ORIENTED_EDGE('',*,*,#14984,.T.);
#20316=ORIENTED_EDGE('',*,*,#14987,.F.);
#20317=ORIENTED_EDGE('',*,*,#15003,.F.);
#20318=ORIENTED_EDGE('',*,*,#15000,.T.);
#20319=ORIENTED_EDGE('',*,*,#14998,.T.);
#20320=ORIENTED_EDGE('',*,*,#15004,.F.);
#20321=ORIENTED_EDGE('',*,*,#14989,.F.);
#20322=ORIENTED_EDGE('',*,*,#15005,.F.);
#20323=ORIENTED_EDGE('',*,*,#14996,.T.);
#20324=ORIENTED_EDGE('',*,*,#15002,.F.);
#20325=ORIENTED_EDGE('',*,*,#15014,.F.);
#20326=ORIENTED_EDGE('',*,*,#15016,.T.);
#20327=ORIENTED_EDGE('',*,*,#15018,.T.);
#20328=ORIENTED_EDGE('',*,*,#15019,.F.);
#20329=ORIENTED_EDGE('',*,*,#15018,.F.);
#20330=ORIENTED_EDGE('',*,*,#15020,.F.);
#20331=ORIENTED_EDGE('',*,*,#15019,.T.);
#20332=ORIENTED_EDGE('',*,*,#14982,.F.);
#20333=ORIENTED_EDGE('',*,*,#15021,.T.);
#20334=ORIENTED_EDGE('',*,*,#15020,.T.);
#20335=ORIENTED_EDGE('',*,*,#15021,.F.);
#20336=ORIENTED_EDGE('',*,*,#15001,.F.);
#20337=ORIENTED_EDGE('',*,*,#15022,.T.);
#20338=ORIENTED_EDGE('',*,*,#14980,.T.);
#20339=ORIENTED_EDGE('',*,*,#15022,.F.);
#20340=ORIENTED_EDGE('',*,*,#15023,.T.);
#20341=ORIENTED_EDGE('',*,*,#15024,.T.);
#20342=ORIENTED_EDGE('',*,*,#15025,.T.);
#20343=ORIENTED_EDGE('',*,*,#15026,.T.);
#20344=ORIENTED_EDGE('',*,*,#15027,.T.);
#20345=ORIENTED_EDGE('',*,*,#15028,.T.);
#20346=ORIENTED_EDGE('',*,*,#15028,.F.);
#20347=ORIENTED_EDGE('',*,*,#15029,.T.);
#20348=ORIENTED_EDGE('',*,*,#15030,.F.);
#20349=ORIENTED_EDGE('',*,*,#15031,.T.);
#20350=ORIENTED_EDGE('',*,*,#15032,.T.);
#20351=ORIENTED_EDGE('',*,*,#15027,.F.);
#20352=ORIENTED_EDGE('',*,*,#15033,.F.);
#20353=ORIENTED_EDGE('',*,*,#15034,.T.);
#20354=ORIENTED_EDGE('',*,*,#15029,.F.);
#20355=ORIENTED_EDGE('',*,*,#15026,.F.);
#20356=ORIENTED_EDGE('',*,*,#15035,.T.);
#20357=ORIENTED_EDGE('',*,*,#15036,.T.);
#20358=ORIENTED_EDGE('',*,*,#15037,.T.);
#20359=ORIENTED_EDGE('',*,*,#15033,.T.);
#20360=ORIENTED_EDGE('',*,*,#15038,.T.);
#20361=ORIENTED_EDGE('',*,*,#15039,.T.);
#20362=ORIENTED_EDGE('',*,*,#15040,.T.);
#20363=ORIENTED_EDGE('',*,*,#15041,.T.);
#20364=ORIENTED_EDGE('',*,*,#15042,.T.);
#20365=ORIENTED_EDGE('',*,*,#15043,.T.);
#20366=ORIENTED_EDGE('',*,*,#15043,.F.);
#20367=ORIENTED_EDGE('',*,*,#15044,.T.);
#20368=ORIENTED_EDGE('',*,*,#15045,.F.);
#20369=ORIENTED_EDGE('',*,*,#15046,.T.);
#20370=ORIENTED_EDGE('',*,*,#15047,.T.);
#20371=ORIENTED_EDGE('',*,*,#15042,.F.);
#20372=ORIENTED_EDGE('',*,*,#15048,.F.);
#20373=ORIENTED_EDGE('',*,*,#15049,.T.);
#20374=ORIENTED_EDGE('',*,*,#15044,.F.);
#20375=ORIENTED_EDGE('',*,*,#15041,.F.);
#20376=ORIENTED_EDGE('',*,*,#15050,.T.);
#20377=ORIENTED_EDGE('',*,*,#15051,.T.);
#20378=ORIENTED_EDGE('',*,*,#15052,.T.);
#20379=ORIENTED_EDGE('',*,*,#15048,.T.);
#20380=ORIENTED_EDGE('',*,*,#15053,.T.);
#20381=ORIENTED_EDGE('',*,*,#15054,.T.);
#20382=ORIENTED_EDGE('',*,*,#15055,.T.);
#20383=ORIENTED_EDGE('',*,*,#15056,.T.);
#20384=ORIENTED_EDGE('',*,*,#15057,.T.);
#20385=ORIENTED_EDGE('',*,*,#15058,.T.);
#20386=ORIENTED_EDGE('',*,*,#15057,.F.);
#20387=ORIENTED_EDGE('',*,*,#15059,.F.);
#20388=ORIENTED_EDGE('',*,*,#15060,.T.);
#20389=ORIENTED_EDGE('',*,*,#15061,.F.);
#20390=ORIENTED_EDGE('',*,*,#15056,.F.);
#20391=ORIENTED_EDGE('',*,*,#15062,.T.);
#20392=ORIENTED_EDGE('',*,*,#15063,.T.);
#20393=ORIENTED_EDGE('',*,*,#15064,.T.);
#20394=ORIENTED_EDGE('',*,*,#15059,.T.);
#20395=ORIENTED_EDGE('',*,*,#15055,.F.);
#20396=ORIENTED_EDGE('',*,*,#15065,.T.);
#20397=ORIENTED_EDGE('',*,*,#15066,.F.);
#20398=ORIENTED_EDGE('',*,*,#15067,.F.);
#20399=ORIENTED_EDGE('',*,*,#15068,.T.);
#20400=ORIENTED_EDGE('',*,*,#15062,.F.);
#20401=ORIENTED_EDGE('',*,*,#15069,.T.);
#20402=ORIENTED_EDGE('',*,*,#15070,.T.);
#20403=ORIENTED_EDGE('',*,*,#15071,.T.);
#20404=ORIENTED_EDGE('',*,*,#15072,.T.);
#20405=ORIENTED_EDGE('',*,*,#15073,.T.);
#20406=ORIENTED_EDGE('',*,*,#15074,.T.);
#20407=ORIENTED_EDGE('',*,*,#15074,.F.);
#20408=ORIENTED_EDGE('',*,*,#15075,.T.);
#20409=ORIENTED_EDGE('',*,*,#15076,.F.);
#20410=ORIENTED_EDGE('',*,*,#15077,.T.);
#20411=ORIENTED_EDGE('',*,*,#15078,.T.);
#20412=ORIENTED_EDGE('',*,*,#15073,.F.);
#20413=ORIENTED_EDGE('',*,*,#15079,.F.);
#20414=ORIENTED_EDGE('',*,*,#15080,.T.);
#20415=ORIENTED_EDGE('',*,*,#15075,.F.);
#20416=ORIENTED_EDGE('',*,*,#15072,.F.);
#20417=ORIENTED_EDGE('',*,*,#15081,.T.);
#20418=ORIENTED_EDGE('',*,*,#15082,.T.);
#20419=ORIENTED_EDGE('',*,*,#15083,.T.);
#20420=ORIENTED_EDGE('',*,*,#15079,.T.);
#20421=ORIENTED_EDGE('',*,*,#15084,.T.);
#20422=ORIENTED_EDGE('',*,*,#15085,.T.);
#20423=ORIENTED_EDGE('',*,*,#15086,.T.);
#20424=ORIENTED_EDGE('',*,*,#15087,.T.);
#20425=ORIENTED_EDGE('',*,*,#15088,.T.);
#20426=ORIENTED_EDGE('',*,*,#15089,.T.);
#20427=ORIENTED_EDGE('',*,*,#15085,.F.);
#20428=ORIENTED_EDGE('',*,*,#15090,.F.);
#20429=ORIENTED_EDGE('',*,*,#15091,.F.);
#20430=ORIENTED_EDGE('',*,*,#15092,.F.);
#20431=ORIENTED_EDGE('',*,*,#15084,.F.);
#20432=ORIENTED_EDGE('',*,*,#15093,.F.);
#20433=ORIENTED_EDGE('',*,*,#15094,.T.);
#20434=ORIENTED_EDGE('',*,*,#15095,.F.);
#20435=ORIENTED_EDGE('',*,*,#15096,.F.);
#20436=ORIENTED_EDGE('',*,*,#15090,.T.);
#20437=ORIENTED_EDGE('',*,*,#15089,.F.);
#20438=ORIENTED_EDGE('',*,*,#15097,.T.);
#20439=ORIENTED_EDGE('',*,*,#15098,.T.);
#20440=ORIENTED_EDGE('',*,*,#15099,.T.);
#20441=ORIENTED_EDGE('',*,*,#15093,.T.);
#20442=ORIENTED_EDGE('',*,*,#15100,.T.);
#20443=ORIENTED_EDGE('',*,*,#15101,.T.);
#20444=ORIENTED_EDGE('',*,*,#15102,.T.);
#20445=ORIENTED_EDGE('',*,*,#15103,.T.);
#20446=ORIENTED_EDGE('',*,*,#15104,.T.);
#20447=ORIENTED_EDGE('',*,*,#15105,.T.);
#20448=ORIENTED_EDGE('',*,*,#15103,.F.);
#20449=ORIENTED_EDGE('',*,*,#15106,.T.);
#20450=ORIENTED_EDGE('',*,*,#15107,.T.);
#20451=ORIENTED_EDGE('',*,*,#15108,.F.);
#20452=ORIENTED_EDGE('',*,*,#15109,.T.);
#20453=ORIENTED_EDGE('',*,*,#15102,.F.);
#20454=ORIENTED_EDGE('',*,*,#15110,.T.);
#20455=ORIENTED_EDGE('',*,*,#15111,.F.);
#20456=ORIENTED_EDGE('',*,*,#15112,.F.);
#20457=ORIENTED_EDGE('',*,*,#15113,.T.);
#20458=ORIENTED_EDGE('',*,*,#15106,.F.);
#20459=ORIENTED_EDGE('',*,*,#15101,.F.);
#20460=ORIENTED_EDGE('',*,*,#15114,.F.);
#20461=ORIENTED_EDGE('',*,*,#15115,.F.);
#20462=ORIENTED_EDGE('',*,*,#15110,.F.);
#20463=ORIENTED_EDGE('',*,*,#15111,.T.);
#20464=ORIENTED_EDGE('',*,*,#15115,.T.);
#20465=ORIENTED_EDGE('',*,*,#15116,.T.);
#20466=ORIENTED_EDGE('',*,*,#15117,.T.);
#20467=ORIENTED_EDGE('',*,*,#15118,.T.);
#20468=ORIENTED_EDGE('',*,*,#15119,.T.);
#20469=ORIENTED_EDGE('',*,*,#15119,.F.);
#20470=ORIENTED_EDGE('',*,*,#15120,.T.);
#20471=ORIENTED_EDGE('',*,*,#15121,.T.);
#20472=ORIENTED_EDGE('',*,*,#15122,.T.);
#20473=ORIENTED_EDGE('',*,*,#15112,.T.);
#20474=ORIENTED_EDGE('',*,*,#15123,.T.);
#20475=ORIENTED_EDGE('',*,*,#15124,.T.);
#20476=ORIENTED_EDGE('',*,*,#15125,.T.);
#20477=ORIENTED_EDGE('',*,*,#15126,.T.);
#20478=ORIENTED_EDGE('',*,*,#15127,.T.);
#20479=ORIENTED_EDGE('',*,*,#15128,.T.);
#20480=ORIENTED_EDGE('',*,*,#15127,.F.);
#20481=ORIENTED_EDGE('',*,*,#15129,.F.);
#20482=ORIENTED_EDGE('',*,*,#15130,.F.);
#20483=ORIENTED_EDGE('',*,*,#15131,.F.);
#20484=ORIENTED_EDGE('',*,*,#15126,.F.);
#20485=ORIENTED_EDGE('',*,*,#15132,.T.);
#20486=ORIENTED_EDGE('',*,*,#15133,.T.);
#20487=ORIENTED_EDGE('',*,*,#15134,.F.);
#20488=ORIENTED_EDGE('',*,*,#15129,.T.);
#20489=ORIENTED_EDGE('',*,*,#15038,.F.);
#20490=ORIENTED_EDGE('',*,*,#15047,.F.);
#20491=ORIENTED_EDGE('',*,*,#15135,.T.);
#20492=ORIENTED_EDGE('',*,*,#15132,.F.);
#20493=ORIENTED_EDGE('',*,*,#15125,.F.);
#20494=ORIENTED_EDGE('',*,*,#15136,.T.);
#20495=ORIENTED_EDGE('',*,*,#15137,.T.);
#20496=ORIENTED_EDGE('',*,*,#15138,.T.);
#20497=ORIENTED_EDGE('',*,*,#15139,.T.);
#20498=ORIENTED_EDGE('',*,*,#15140,.T.);
#20499=ORIENTED_EDGE('',*,*,#15141,.T.);
#20500=ORIENTED_EDGE('',*,*,#15142,.T.);
#20501=ORIENTED_EDGE('',*,*,#15138,.F.);
#20502=ORIENTED_EDGE('',*,*,#15143,.F.);
#20503=ORIENTED_EDGE('',*,*,#15144,.F.);
#20504=ORIENTED_EDGE('',*,*,#15145,.F.);
#20505=ORIENTED_EDGE('',*,*,#15137,.F.);
#20506=ORIENTED_EDGE('',*,*,#15146,.F.);
#20507=ORIENTED_EDGE('',*,*,#15147,.T.);
#20508=ORIENTED_EDGE('',*,*,#15148,.F.);
#20509=ORIENTED_EDGE('',*,*,#15149,.F.);
#20510=ORIENTED_EDGE('',*,*,#15143,.T.);
#20511=ORIENTED_EDGE('',*,*,#15142,.F.);
#20512=ORIENTED_EDGE('',*,*,#15150,.T.);
#20513=ORIENTED_EDGE('',*,*,#15151,.T.);
#20514=ORIENTED_EDGE('',*,*,#15152,.T.);
#20515=ORIENTED_EDGE('',*,*,#15146,.T.);
#20516=ORIENTED_EDGE('',*,*,#15153,.T.);
#20517=ORIENTED_EDGE('',*,*,#15154,.T.);
#20518=ORIENTED_EDGE('',*,*,#15155,.T.);
#20519=ORIENTED_EDGE('',*,*,#15156,.T.);
#20520=ORIENTED_EDGE('',*,*,#15157,.T.);
#20521=ORIENTED_EDGE('',*,*,#15158,.T.);
#20522=ORIENTED_EDGE('',*,*,#15156,.F.);
#20523=ORIENTED_EDGE('',*,*,#15159,.T.);
#20524=ORIENTED_EDGE('',*,*,#15160,.T.);
#20525=ORIENTED_EDGE('',*,*,#15161,.F.);
#20526=ORIENTED_EDGE('',*,*,#15162,.T.);
#20527=ORIENTED_EDGE('',*,*,#15155,.F.);
#20528=ORIENTED_EDGE('',*,*,#15163,.T.);
#20529=ORIENTED_EDGE('',*,*,#15164,.F.);
#20530=ORIENTED_EDGE('',*,*,#15165,.F.);
#20531=ORIENTED_EDGE('',*,*,#15166,.T.);
#20532=ORIENTED_EDGE('',*,*,#15159,.F.);
#20533=ORIENTED_EDGE('',*,*,#15154,.F.);
#20534=ORIENTED_EDGE('',*,*,#15167,.F.);
#20535=ORIENTED_EDGE('',*,*,#15168,.F.);
#20536=ORIENTED_EDGE('',*,*,#15163,.F.);
#20537=ORIENTED_EDGE('',*,*,#15164,.T.);
#20538=ORIENTED_EDGE('',*,*,#15168,.T.);
#20539=ORIENTED_EDGE('',*,*,#15169,.T.);
#20540=ORIENTED_EDGE('',*,*,#15170,.T.);
#20541=ORIENTED_EDGE('',*,*,#15171,.T.);
#20542=ORIENTED_EDGE('',*,*,#15172,.T.);
#20543=ORIENTED_EDGE('',*,*,#15172,.F.);
#20544=ORIENTED_EDGE('',*,*,#15173,.T.);
#20545=ORIENTED_EDGE('',*,*,#15174,.T.);
#20546=ORIENTED_EDGE('',*,*,#15175,.T.);
#20547=ORIENTED_EDGE('',*,*,#15165,.T.);
#20548=ORIENTED_EDGE('',*,*,#15176,.T.);
#20549=ORIENTED_EDGE('',*,*,#15177,.T.);
#20550=ORIENTED_EDGE('',*,*,#15178,.T.);
#20551=ORIENTED_EDGE('',*,*,#15179,.T.);
#20552=ORIENTED_EDGE('',*,*,#15180,.T.);
#20553=ORIENTED_EDGE('',*,*,#15181,.T.);
#20554=ORIENTED_EDGE('',*,*,#15180,.F.);
#20555=ORIENTED_EDGE('',*,*,#15182,.F.);
#20556=ORIENTED_EDGE('',*,*,#15183,.F.);
#20557=ORIENTED_EDGE('',*,*,#15184,.F.);
#20558=ORIENTED_EDGE('',*,*,#15179,.F.);
#20559=ORIENTED_EDGE('',*,*,#15185,.T.);
#20560=ORIENTED_EDGE('',*,*,#15186,.T.);
#20561=ORIENTED_EDGE('',*,*,#15187,.F.);
#20562=ORIENTED_EDGE('',*,*,#15182,.T.);
#20563=ORIENTED_EDGE('',*,*,#15023,.F.);
#20564=ORIENTED_EDGE('',*,*,#15032,.F.);
#20565=ORIENTED_EDGE('',*,*,#15188,.T.);
#20566=ORIENTED_EDGE('',*,*,#15185,.F.);
#20567=ORIENTED_EDGE('',*,*,#15178,.F.);
#20568=ORIENTED_EDGE('',*,*,#15189,.T.);
#20569=ORIENTED_EDGE('',*,*,#15190,.T.);
#20570=ORIENTED_EDGE('',*,*,#15191,.T.);
#20571=ORIENTED_EDGE('',*,*,#15192,.T.);
#20572=ORIENTED_EDGE('',*,*,#15193,.T.);
#20573=ORIENTED_EDGE('',*,*,#15194,.T.);
#20574=ORIENTED_EDGE('',*,*,#15195,.T.);
#20575=ORIENTED_EDGE('',*,*,#15193,.F.);
#20576=ORIENTED_EDGE('',*,*,#15196,.T.);
#20577=ORIENTED_EDGE('',*,*,#15197,.T.);
#20578=ORIENTED_EDGE('',*,*,#15198,.F.);
#20579=ORIENTED_EDGE('',*,*,#15199,.T.);
#20580=ORIENTED_EDGE('',*,*,#15192,.F.);
#20581=ORIENTED_EDGE('',*,*,#15200,.T.);
#20582=ORIENTED_EDGE('',*,*,#15201,.F.);
#20583=ORIENTED_EDGE('',*,*,#15202,.F.);
#20584=ORIENTED_EDGE('',*,*,#15203,.T.);
#20585=ORIENTED_EDGE('',*,*,#15196,.F.);
#20586=ORIENTED_EDGE('',*,*,#15191,.F.);
#20587=ORIENTED_EDGE('',*,*,#15204,.F.);
#20588=ORIENTED_EDGE('',*,*,#15205,.F.);
#20589=ORIENTED_EDGE('',*,*,#15200,.F.);
#20590=ORIENTED_EDGE('',*,*,#15201,.T.);
#20591=ORIENTED_EDGE('',*,*,#15205,.T.);
#20592=ORIENTED_EDGE('',*,*,#15206,.T.);
#20593=ORIENTED_EDGE('',*,*,#15207,.T.);
#20594=ORIENTED_EDGE('',*,*,#15208,.T.);
#20595=ORIENTED_EDGE('',*,*,#15209,.T.);
#20596=ORIENTED_EDGE('',*,*,#15209,.F.);
#20597=ORIENTED_EDGE('',*,*,#15210,.T.);
#20598=ORIENTED_EDGE('',*,*,#15211,.T.);
#20599=ORIENTED_EDGE('',*,*,#15212,.T.);
#20600=ORIENTED_EDGE('',*,*,#15202,.T.);
#20601=ORIENTED_EDGE('',*,*,#15213,.T.);
#20602=ORIENTED_EDGE('',*,*,#15214,.T.);
#20603=ORIENTED_EDGE('',*,*,#15215,.T.);
#20604=ORIENTED_EDGE('',*,*,#15216,.T.);
#20605=ORIENTED_EDGE('',*,*,#15217,.T.);
#20606=ORIENTED_EDGE('',*,*,#15218,.T.);
#20607=ORIENTED_EDGE('',*,*,#15217,.F.);
#20608=ORIENTED_EDGE('',*,*,#15219,.F.);
#20609=ORIENTED_EDGE('',*,*,#15220,.F.);
#20610=ORIENTED_EDGE('',*,*,#15221,.F.);
#20611=ORIENTED_EDGE('',*,*,#15216,.F.);
#20612=ORIENTED_EDGE('',*,*,#15222,.T.);
#20613=ORIENTED_EDGE('',*,*,#15223,.T.);
#20614=ORIENTED_EDGE('',*,*,#15224,.F.);
#20615=ORIENTED_EDGE('',*,*,#15219,.T.);
#20616=ORIENTED_EDGE('',*,*,#15215,.F.);
#20617=ORIENTED_EDGE('',*,*,#15225,.T.);
#20618=ORIENTED_EDGE('',*,*,#15226,.F.);
#20619=ORIENTED_EDGE('',*,*,#15227,.F.);
#20620=ORIENTED_EDGE('',*,*,#15228,.T.);
#20621=ORIENTED_EDGE('',*,*,#15222,.F.);
#20622=ORIENTED_EDGE('',*,*,#15226,.T.);
#20623=ORIENTED_EDGE('',*,*,#15229,.T.);
#20624=ORIENTED_EDGE('',*,*,#15230,.T.);
#20625=ORIENTED_EDGE('',*,*,#15231,.T.);
#20626=ORIENTED_EDGE('',*,*,#15232,.T.);
#20627=ORIENTED_EDGE('',*,*,#15233,.T.);
#20628=ORIENTED_EDGE('',*,*,#15232,.F.);
#20629=ORIENTED_EDGE('',*,*,#15234,.F.);
#20630=ORIENTED_EDGE('',*,*,#15235,.T.);
#20631=ORIENTED_EDGE('',*,*,#15236,.F.);
#20632=ORIENTED_EDGE('',*,*,#15231,.F.);
#20633=ORIENTED_EDGE('',*,*,#15237,.T.);
#20634=ORIENTED_EDGE('',*,*,#15238,.T.);
#20635=ORIENTED_EDGE('',*,*,#15239,.T.);
#20636=ORIENTED_EDGE('',*,*,#15234,.T.);
#20637=ORIENTED_EDGE('',*,*,#15213,.F.);
#20638=ORIENTED_EDGE('',*,*,#15240,.F.);
#20639=ORIENTED_EDGE('',*,*,#15241,.T.);
#20640=ORIENTED_EDGE('',*,*,#15237,.F.);
#20641=ORIENTED_EDGE('',*,*,#15230,.F.);
#20642=ORIENTED_EDGE('',*,*,#15242,.T.);
#20643=ORIENTED_EDGE('',*,*,#15243,.T.);
#20644=ORIENTED_EDGE('',*,*,#15244,.T.);
#20645=ORIENTED_EDGE('',*,*,#15245,.T.);
#20646=ORIENTED_EDGE('',*,*,#15246,.T.);
#20647=ORIENTED_EDGE('',*,*,#15247,.T.);
#20648=ORIENTED_EDGE('',*,*,#15248,.T.);
#20649=ORIENTED_EDGE('',*,*,#15246,.F.);
#20650=ORIENTED_EDGE('',*,*,#15249,.T.);
#20651=ORIENTED_EDGE('',*,*,#15250,.T.);
#20652=ORIENTED_EDGE('',*,*,#15251,.F.);
#20653=ORIENTED_EDGE('',*,*,#15252,.T.);
#20654=ORIENTED_EDGE('',*,*,#15245,.F.);
#20655=ORIENTED_EDGE('',*,*,#15253,.T.);
#20656=ORIENTED_EDGE('',*,*,#15254,.F.);
#20657=ORIENTED_EDGE('',*,*,#15255,.F.);
#20658=ORIENTED_EDGE('',*,*,#15256,.T.);
#20659=ORIENTED_EDGE('',*,*,#15249,.F.);
#20660=ORIENTED_EDGE('',*,*,#15244,.F.);
#20661=ORIENTED_EDGE('',*,*,#15257,.F.);
#20662=ORIENTED_EDGE('',*,*,#15258,.F.);
#20663=ORIENTED_EDGE('',*,*,#15253,.F.);
#20664=ORIENTED_EDGE('',*,*,#15254,.T.);
#20665=ORIENTED_EDGE('',*,*,#15258,.T.);
#20666=ORIENTED_EDGE('',*,*,#15259,.T.);
#20667=ORIENTED_EDGE('',*,*,#15260,.T.);
#20668=ORIENTED_EDGE('',*,*,#15261,.T.);
#20669=ORIENTED_EDGE('',*,*,#15262,.T.);
#20670=ORIENTED_EDGE('',*,*,#15262,.F.);
#20671=ORIENTED_EDGE('',*,*,#15263,.T.);
#20672=ORIENTED_EDGE('',*,*,#15264,.T.);
#20673=ORIENTED_EDGE('',*,*,#15265,.T.);
#20674=ORIENTED_EDGE('',*,*,#15255,.T.);
#20675=ORIENTED_EDGE('',*,*,#15266,.T.);
#20676=ORIENTED_EDGE('',*,*,#15267,.T.);
#20677=ORIENTED_EDGE('',*,*,#15268,.T.);
#20678=ORIENTED_EDGE('',*,*,#15269,.T.);
#20679=ORIENTED_EDGE('',*,*,#15270,.T.);
#20680=ORIENTED_EDGE('',*,*,#15271,.T.);
#20681=ORIENTED_EDGE('',*,*,#15269,.F.);
#20682=ORIENTED_EDGE('',*,*,#15272,.T.);
#20683=ORIENTED_EDGE('',*,*,#15273,.T.);
#20684=ORIENTED_EDGE('',*,*,#15274,.F.);
#20685=ORIENTED_EDGE('',*,*,#15275,.T.);
#20686=ORIENTED_EDGE('',*,*,#15268,.F.);
#20687=ORIENTED_EDGE('',*,*,#15276,.T.);
#20688=ORIENTED_EDGE('',*,*,#15277,.F.);
#20689=ORIENTED_EDGE('',*,*,#15278,.F.);
#20690=ORIENTED_EDGE('',*,*,#15279,.T.);
#20691=ORIENTED_EDGE('',*,*,#15272,.F.);
#20692=ORIENTED_EDGE('',*,*,#15267,.F.);
#20693=ORIENTED_EDGE('',*,*,#15280,.F.);
#20694=ORIENTED_EDGE('',*,*,#15281,.F.);
#20695=ORIENTED_EDGE('',*,*,#15276,.F.);
#20696=ORIENTED_EDGE('',*,*,#15277,.T.);
#20697=ORIENTED_EDGE('',*,*,#15281,.T.);
#20698=ORIENTED_EDGE('',*,*,#15282,.T.);
#20699=ORIENTED_EDGE('',*,*,#15283,.T.);
#20700=ORIENTED_EDGE('',*,*,#15284,.T.);
#20701=ORIENTED_EDGE('',*,*,#15285,.T.);
#20702=ORIENTED_EDGE('',*,*,#15285,.F.);
#20703=ORIENTED_EDGE('',*,*,#15286,.T.);
#20704=ORIENTED_EDGE('',*,*,#15287,.T.);
#20705=ORIENTED_EDGE('',*,*,#15288,.T.);
#20706=ORIENTED_EDGE('',*,*,#15278,.T.);
#20707=ORIENTED_EDGE('',*,*,#15289,.T.);
#20708=ORIENTED_EDGE('',*,*,#15290,.T.);
#20709=ORIENTED_EDGE('',*,*,#15291,.T.);
#20710=ORIENTED_EDGE('',*,*,#15292,.T.);
#20711=ORIENTED_EDGE('',*,*,#15293,.T.);
#20712=ORIENTED_EDGE('',*,*,#15294,.T.);
#20713=ORIENTED_EDGE('',*,*,#15294,.F.);
#20714=ORIENTED_EDGE('',*,*,#15295,.T.);
#20715=ORIENTED_EDGE('',*,*,#15296,.F.);
#20716=ORIENTED_EDGE('',*,*,#15297,.T.);
#20717=ORIENTED_EDGE('',*,*,#15298,.T.);
#20718=ORIENTED_EDGE('',*,*,#15293,.F.);
#20719=ORIENTED_EDGE('',*,*,#15299,.F.);
#20720=ORIENTED_EDGE('',*,*,#15300,.F.);
#20721=ORIENTED_EDGE('',*,*,#15295,.F.);
#20722=ORIENTED_EDGE('',*,*,#15292,.F.);
#20723=ORIENTED_EDGE('',*,*,#15301,.T.);
#20724=ORIENTED_EDGE('',*,*,#15302,.T.);
#20725=ORIENTED_EDGE('',*,*,#15303,.F.);
#20726=ORIENTED_EDGE('',*,*,#15299,.T.);
#20727=ORIENTED_EDGE('',*,*,#15304,.T.);
#20728=ORIENTED_EDGE('',*,*,#15305,.T.);
#20729=ORIENTED_EDGE('',*,*,#15306,.T.);
#20730=ORIENTED_EDGE('',*,*,#15307,.T.);
#20731=ORIENTED_EDGE('',*,*,#15308,.T.);
#20732=ORIENTED_EDGE('',*,*,#15309,.T.);
#20733=ORIENTED_EDGE('',*,*,#15307,.F.);
#20734=ORIENTED_EDGE('',*,*,#15310,.T.);
#20735=ORIENTED_EDGE('',*,*,#15311,.T.);
#20736=ORIENTED_EDGE('',*,*,#15312,.F.);
#20737=ORIENTED_EDGE('',*,*,#15313,.T.);
#20738=ORIENTED_EDGE('',*,*,#15306,.F.);
#20739=ORIENTED_EDGE('',*,*,#15314,.T.);
#20740=ORIENTED_EDGE('',*,*,#15315,.F.);
#20741=ORIENTED_EDGE('',*,*,#15316,.F.);
#20742=ORIENTED_EDGE('',*,*,#15317,.T.);
#20743=ORIENTED_EDGE('',*,*,#15310,.F.);
#20744=ORIENTED_EDGE('',*,*,#15305,.F.);
#20745=ORIENTED_EDGE('',*,*,#15318,.F.);
#20746=ORIENTED_EDGE('',*,*,#15319,.F.);
#20747=ORIENTED_EDGE('',*,*,#15314,.F.);
#20748=ORIENTED_EDGE('',*,*,#15315,.T.);
#20749=ORIENTED_EDGE('',*,*,#15319,.T.);
#20750=ORIENTED_EDGE('',*,*,#15320,.T.);
#20751=ORIENTED_EDGE('',*,*,#15321,.T.);
#20752=ORIENTED_EDGE('',*,*,#15322,.T.);
#20753=ORIENTED_EDGE('',*,*,#15323,.T.);
#20754=ORIENTED_EDGE('',*,*,#15323,.F.);
#20755=ORIENTED_EDGE('',*,*,#15324,.T.);
#20756=ORIENTED_EDGE('',*,*,#15325,.T.);
#20757=ORIENTED_EDGE('',*,*,#15326,.T.);
#20758=ORIENTED_EDGE('',*,*,#15316,.T.);
#20759=ORIENTED_EDGE('',*,*,#15327,.T.);
#20760=ORIENTED_EDGE('',*,*,#15328,.T.);
#20761=ORIENTED_EDGE('',*,*,#15329,.T.);
#20762=ORIENTED_EDGE('',*,*,#15330,.T.);
#20763=ORIENTED_EDGE('',*,*,#15331,.T.);
#20764=ORIENTED_EDGE('',*,*,#15332,.T.);
#20765=ORIENTED_EDGE('',*,*,#15330,.F.);
#20766=ORIENTED_EDGE('',*,*,#15333,.T.);
#20767=ORIENTED_EDGE('',*,*,#15334,.T.);
#20768=ORIENTED_EDGE('',*,*,#15335,.F.);
#20769=ORIENTED_EDGE('',*,*,#15336,.T.);
#20770=ORIENTED_EDGE('',*,*,#15329,.F.);
#20771=ORIENTED_EDGE('',*,*,#15337,.T.);
#20772=ORIENTED_EDGE('',*,*,#15338,.F.);
#20773=ORIENTED_EDGE('',*,*,#15339,.F.);
#20774=ORIENTED_EDGE('',*,*,#15340,.T.);
#20775=ORIENTED_EDGE('',*,*,#15333,.F.);
#20776=ORIENTED_EDGE('',*,*,#15328,.F.);
#20777=ORIENTED_EDGE('',*,*,#15341,.F.);
#20778=ORIENTED_EDGE('',*,*,#15342,.F.);
#20779=ORIENTED_EDGE('',*,*,#15337,.F.);
#20780=ORIENTED_EDGE('',*,*,#15338,.T.);
#20781=ORIENTED_EDGE('',*,*,#15342,.T.);
#20782=ORIENTED_EDGE('',*,*,#15343,.T.);
#20783=ORIENTED_EDGE('',*,*,#15344,.T.);
#20784=ORIENTED_EDGE('',*,*,#15345,.T.);
#20785=ORIENTED_EDGE('',*,*,#15346,.T.);
#20786=ORIENTED_EDGE('',*,*,#15346,.F.);
#20787=ORIENTED_EDGE('',*,*,#15347,.T.);
#20788=ORIENTED_EDGE('',*,*,#15348,.T.);
#20789=ORIENTED_EDGE('',*,*,#15349,.T.);
#20790=ORIENTED_EDGE('',*,*,#15339,.T.);
#20791=ORIENTED_EDGE('',*,*,#15066,.T.);
#20792=ORIENTED_EDGE('',*,*,#15350,.T.);
#20793=ORIENTED_EDGE('',*,*,#15351,.T.);
#20794=ORIENTED_EDGE('',*,*,#15352,.T.);
#20795=ORIENTED_EDGE('',*,*,#15353,.T.);
#20796=ORIENTED_EDGE('',*,*,#15354,.T.);
#20797=ORIENTED_EDGE('',*,*,#15354,.F.);
#20798=ORIENTED_EDGE('',*,*,#15355,.T.);
#20799=ORIENTED_EDGE('',*,*,#15356,.F.);
#20800=ORIENTED_EDGE('',*,*,#15357,.T.);
#20801=ORIENTED_EDGE('',*,*,#15067,.T.);
#20802=ORIENTED_EDGE('',*,*,#15353,.F.);
#20803=ORIENTED_EDGE('',*,*,#15358,.F.);
#20804=ORIENTED_EDGE('',*,*,#15359,.F.);
#20805=ORIENTED_EDGE('',*,*,#15355,.F.);
#20806=ORIENTED_EDGE('',*,*,#15352,.F.);
#20807=ORIENTED_EDGE('',*,*,#15360,.T.);
#20808=ORIENTED_EDGE('',*,*,#15361,.T.);
#20809=ORIENTED_EDGE('',*,*,#15362,.F.);
#20810=ORIENTED_EDGE('',*,*,#15358,.T.);
#20811=ORIENTED_EDGE('',*,*,#15363,.T.);
#20812=ORIENTED_EDGE('',*,*,#15364,.T.);
#20813=ORIENTED_EDGE('',*,*,#15365,.T.);
#20814=ORIENTED_EDGE('',*,*,#15366,.T.);
#20815=ORIENTED_EDGE('',*,*,#15366,.F.);
#20816=ORIENTED_EDGE('',*,*,#15367,.F.);
#20817=ORIENTED_EDGE('',*,*,#15368,.F.);
#20818=ORIENTED_EDGE('',*,*,#15369,.F.);
#20819=ORIENTED_EDGE('',*,*,#15370,.F.);
#20820=ORIENTED_EDGE('',*,*,#15365,.F.);
#20821=ORIENTED_EDGE('',*,*,#15371,.T.);
#20822=ORIENTED_EDGE('',*,*,#15372,.F.);
#20823=ORIENTED_EDGE('',*,*,#15373,.F.);
#20824=ORIENTED_EDGE('',*,*,#15374,.F.);
#20825=ORIENTED_EDGE('',*,*,#15367,.T.);
#20826=ORIENTED_EDGE('',*,*,#15375,.T.);
#20827=ORIENTED_EDGE('',*,*,#15376,.T.);
#20828=ORIENTED_EDGE('',*,*,#15377,.T.);
#20829=ORIENTED_EDGE('',*,*,#15378,.T.);
#20830=ORIENTED_EDGE('',*,*,#15379,.T.);
#20831=ORIENTED_EDGE('',*,*,#15380,.T.);
#20832=ORIENTED_EDGE('',*,*,#15376,.F.);
#20833=ORIENTED_EDGE('',*,*,#15381,.T.);
#20834=ORIENTED_EDGE('',*,*,#15382,.F.);
#20835=ORIENTED_EDGE('',*,*,#15373,.T.);
#20836=ORIENTED_EDGE('',*,*,#15375,.F.);
#20837=ORIENTED_EDGE('',*,*,#15383,.T.);
#20838=ORIENTED_EDGE('',*,*,#15384,.T.);
#20839=ORIENTED_EDGE('',*,*,#15385,.T.);
#20840=ORIENTED_EDGE('',*,*,#15386,.T.);
#20841=ORIENTED_EDGE('',*,*,#15387,.T.);
#20842=ORIENTED_EDGE('',*,*,#15380,.F.);
#20843=ORIENTED_EDGE('',*,*,#15388,.T.);
#20844=ORIENTED_EDGE('',*,*,#15389,.F.);
#20845=ORIENTED_EDGE('',*,*,#15390,.F.);
#20846=ORIENTED_EDGE('',*,*,#15391,.T.);
#20847=ORIENTED_EDGE('',*,*,#15383,.F.);
#20848=ORIENTED_EDGE('',*,*,#15374,.T.);
#20849=ORIENTED_EDGE('',*,*,#15382,.T.);
#20850=ORIENTED_EDGE('',*,*,#15392,.T.);
#20851=ORIENTED_EDGE('',*,*,#15368,.T.);
#20852=ORIENTED_EDGE('',*,*,#15393,.T.);
#20853=ORIENTED_EDGE('',*,*,#15394,.T.);
#20854=ORIENTED_EDGE('',*,*,#15395,.T.);
#20855=ORIENTED_EDGE('',*,*,#15396,.T.);
#20856=ORIENTED_EDGE('',*,*,#15397,.T.);
#20857=ORIENTED_EDGE('',*,*,#15398,.T.);
#20858=ORIENTED_EDGE('',*,*,#15393,.F.);
#20859=ORIENTED_EDGE('',*,*,#15399,.T.);
#20860=ORIENTED_EDGE('',*,*,#15400,.T.);
#20861=ORIENTED_EDGE('',*,*,#15390,.T.);
#20862=ORIENTED_EDGE('',*,*,#15401,.F.);
#20863=ORIENTED_EDGE('',*,*,#15402,.T.);
#20864=ORIENTED_EDGE('',*,*,#15398,.F.);
#20865=ORIENTED_EDGE('',*,*,#15403,.T.);
#20866=ORIENTED_EDGE('',*,*,#15404,.F.);
#20867=ORIENTED_EDGE('',*,*,#15405,.F.);
#20868=ORIENTED_EDGE('',*,*,#15406,.T.);
#20869=ORIENTED_EDGE('',*,*,#15399,.F.);
#20870=ORIENTED_EDGE('',*,*,#15397,.F.);
#20871=ORIENTED_EDGE('',*,*,#15407,.F.);
#20872=ORIENTED_EDGE('',*,*,#15408,.F.);
#20873=ORIENTED_EDGE('',*,*,#15403,.F.);
#20874=ORIENTED_EDGE('',*,*,#15409,.T.);
#20875=ORIENTED_EDGE('',*,*,#15410,.T.);
#20876=ORIENTED_EDGE('',*,*,#15411,.T.);
#20877=ORIENTED_EDGE('',*,*,#15412,.T.);
#20878=ORIENTED_EDGE('',*,*,#15413,.T.);
#20879=ORIENTED_EDGE('',*,*,#15414,.T.);
#20880=ORIENTED_EDGE('',*,*,#15412,.F.);
#20881=ORIENTED_EDGE('',*,*,#15415,.T.);
#20882=ORIENTED_EDGE('',*,*,#15416,.T.);
#20883=ORIENTED_EDGE('',*,*,#15417,.F.);
#20884=ORIENTED_EDGE('',*,*,#15418,.T.);
#20885=ORIENTED_EDGE('',*,*,#15411,.F.);
#20886=ORIENTED_EDGE('',*,*,#15419,.T.);
#20887=ORIENTED_EDGE('',*,*,#15420,.F.);
#20888=ORIENTED_EDGE('',*,*,#15421,.F.);
#20889=ORIENTED_EDGE('',*,*,#15422,.T.);
#20890=ORIENTED_EDGE('',*,*,#15415,.F.);
#20891=ORIENTED_EDGE('',*,*,#15410,.F.);
#20892=ORIENTED_EDGE('',*,*,#15423,.F.);
#20893=ORIENTED_EDGE('',*,*,#15424,.F.);
#20894=ORIENTED_EDGE('',*,*,#15419,.F.);
#20895=ORIENTED_EDGE('',*,*,#15420,.T.);
#20896=ORIENTED_EDGE('',*,*,#15424,.T.);
#20897=ORIENTED_EDGE('',*,*,#15425,.T.);
#20898=ORIENTED_EDGE('',*,*,#15426,.T.);
#20899=ORIENTED_EDGE('',*,*,#15427,.T.);
#20900=ORIENTED_EDGE('',*,*,#15428,.T.);
#20901=ORIENTED_EDGE('',*,*,#15428,.F.);
#20902=ORIENTED_EDGE('',*,*,#15429,.T.);
#20903=ORIENTED_EDGE('',*,*,#15430,.T.);
#20904=ORIENTED_EDGE('',*,*,#15431,.T.);
#20905=ORIENTED_EDGE('',*,*,#15421,.T.);
#20906=ORIENTED_EDGE('',*,*,#15432,.T.);
#20907=ORIENTED_EDGE('',*,*,#15433,.T.);
#20908=ORIENTED_EDGE('',*,*,#15434,.T.);
#20909=ORIENTED_EDGE('',*,*,#15435,.T.);
#20910=ORIENTED_EDGE('',*,*,#15436,.T.);
#20911=ORIENTED_EDGE('',*,*,#15437,.T.);
#20912=ORIENTED_EDGE('',*,*,#15435,.F.);
#20913=ORIENTED_EDGE('',*,*,#15438,.T.);
#20914=ORIENTED_EDGE('',*,*,#15439,.T.);
#20915=ORIENTED_EDGE('',*,*,#15440,.F.);
#20916=ORIENTED_EDGE('',*,*,#15441,.T.);
#20917=ORIENTED_EDGE('',*,*,#15434,.F.);
#20918=ORIENTED_EDGE('',*,*,#15442,.T.);
#20919=ORIENTED_EDGE('',*,*,#15443,.F.);
#20920=ORIENTED_EDGE('',*,*,#15444,.F.);
#20921=ORIENTED_EDGE('',*,*,#15445,.T.);
#20922=ORIENTED_EDGE('',*,*,#15438,.F.);
#20923=ORIENTED_EDGE('',*,*,#15433,.F.);
#20924=ORIENTED_EDGE('',*,*,#15446,.F.);
#20925=ORIENTED_EDGE('',*,*,#15447,.F.);
#20926=ORIENTED_EDGE('',*,*,#15442,.F.);
#20927=ORIENTED_EDGE('',*,*,#15443,.T.);
#20928=ORIENTED_EDGE('',*,*,#15447,.T.);
#20929=ORIENTED_EDGE('',*,*,#15448,.T.);
#20930=ORIENTED_EDGE('',*,*,#15449,.T.);
#20931=ORIENTED_EDGE('',*,*,#15450,.T.);
#20932=ORIENTED_EDGE('',*,*,#15451,.T.);
#20933=ORIENTED_EDGE('',*,*,#15451,.F.);
#20934=ORIENTED_EDGE('',*,*,#15452,.T.);
#20935=ORIENTED_EDGE('',*,*,#15453,.T.);
#20936=ORIENTED_EDGE('',*,*,#15454,.T.);
#20937=ORIENTED_EDGE('',*,*,#15444,.T.);
#20938=ORIENTED_EDGE('',*,*,#15455,.T.);
#20939=ORIENTED_EDGE('',*,*,#15456,.T.);
#20940=ORIENTED_EDGE('',*,*,#15457,.T.);
#20941=ORIENTED_EDGE('',*,*,#15458,.T.);
#20942=ORIENTED_EDGE('',*,*,#15459,.T.);
#20943=ORIENTED_EDGE('',*,*,#15460,.T.);
#20944=ORIENTED_EDGE('',*,*,#15458,.F.);
#20945=ORIENTED_EDGE('',*,*,#15461,.T.);
#20946=ORIENTED_EDGE('',*,*,#15462,.T.);
#20947=ORIENTED_EDGE('',*,*,#15463,.F.);
#20948=ORIENTED_EDGE('',*,*,#15464,.T.);
#20949=ORIENTED_EDGE('',*,*,#15457,.F.);
#20950=ORIENTED_EDGE('',*,*,#15465,.T.);
#20951=ORIENTED_EDGE('',*,*,#15466,.F.);
#20952=ORIENTED_EDGE('',*,*,#15467,.F.);
#20953=ORIENTED_EDGE('',*,*,#15468,.T.);
#20954=ORIENTED_EDGE('',*,*,#15461,.F.);
#20955=ORIENTED_EDGE('',*,*,#15456,.F.);
#20956=ORIENTED_EDGE('',*,*,#15469,.F.);
#20957=ORIENTED_EDGE('',*,*,#15470,.F.);
#20958=ORIENTED_EDGE('',*,*,#15465,.F.);
#20959=ORIENTED_EDGE('',*,*,#15466,.T.);
#20960=ORIENTED_EDGE('',*,*,#15470,.T.);
#20961=ORIENTED_EDGE('',*,*,#15471,.T.);
#20962=ORIENTED_EDGE('',*,*,#15472,.T.);
#20963=ORIENTED_EDGE('',*,*,#15473,.T.);
#20964=ORIENTED_EDGE('',*,*,#15474,.T.);
#20965=ORIENTED_EDGE('',*,*,#15474,.F.);
#20966=ORIENTED_EDGE('',*,*,#15475,.T.);
#20967=ORIENTED_EDGE('',*,*,#15476,.T.);
#20968=ORIENTED_EDGE('',*,*,#15477,.T.);
#20969=ORIENTED_EDGE('',*,*,#15467,.T.);
#20970=ORIENTED_EDGE('',*,*,#15478,.T.);
#20971=ORIENTED_EDGE('',*,*,#15479,.T.);
#20972=ORIENTED_EDGE('',*,*,#15480,.T.);
#20973=ORIENTED_EDGE('',*,*,#15481,.T.);
#20974=ORIENTED_EDGE('',*,*,#15482,.T.);
#20975=ORIENTED_EDGE('',*,*,#15483,.T.);
#20976=ORIENTED_EDGE('',*,*,#15481,.F.);
#20977=ORIENTED_EDGE('',*,*,#15484,.T.);
#20978=ORIENTED_EDGE('',*,*,#15485,.T.);
#20979=ORIENTED_EDGE('',*,*,#15486,.F.);
#20980=ORIENTED_EDGE('',*,*,#15487,.T.);
#20981=ORIENTED_EDGE('',*,*,#15480,.F.);
#20982=ORIENTED_EDGE('',*,*,#15488,.T.);
#20983=ORIENTED_EDGE('',*,*,#15489,.F.);
#20984=ORIENTED_EDGE('',*,*,#15490,.F.);
#20985=ORIENTED_EDGE('',*,*,#15491,.T.);
#20986=ORIENTED_EDGE('',*,*,#15484,.F.);
#20987=ORIENTED_EDGE('',*,*,#15479,.F.);
#20988=ORIENTED_EDGE('',*,*,#15492,.F.);
#20989=ORIENTED_EDGE('',*,*,#15493,.F.);
#20990=ORIENTED_EDGE('',*,*,#15488,.F.);
#20991=ORIENTED_EDGE('',*,*,#15489,.T.);
#20992=ORIENTED_EDGE('',*,*,#15493,.T.);
#20993=ORIENTED_EDGE('',*,*,#15494,.T.);
#20994=ORIENTED_EDGE('',*,*,#15495,.T.);
#20995=ORIENTED_EDGE('',*,*,#15496,.T.);
#20996=ORIENTED_EDGE('',*,*,#15497,.T.);
#20997=ORIENTED_EDGE('',*,*,#15497,.F.);
#20998=ORIENTED_EDGE('',*,*,#15498,.T.);
#20999=ORIENTED_EDGE('',*,*,#15499,.T.);
#21000=ORIENTED_EDGE('',*,*,#15500,.T.);
#21001=ORIENTED_EDGE('',*,*,#15490,.T.);
#21002=ORIENTED_EDGE('',*,*,#15501,.T.);
#21003=ORIENTED_EDGE('',*,*,#15502,.T.);
#21004=ORIENTED_EDGE('',*,*,#15503,.T.);
#21005=ORIENTED_EDGE('',*,*,#15504,.T.);
#21006=ORIENTED_EDGE('',*,*,#15505,.T.);
#21007=ORIENTED_EDGE('',*,*,#15506,.T.);
#21008=ORIENTED_EDGE('',*,*,#15505,.F.);
#21009=ORIENTED_EDGE('',*,*,#15507,.F.);
#21010=ORIENTED_EDGE('',*,*,#15508,.F.);
#21011=ORIENTED_EDGE('',*,*,#15509,.F.);
#21012=ORIENTED_EDGE('',*,*,#15504,.F.);
#21013=ORIENTED_EDGE('',*,*,#15510,.T.);
#21014=ORIENTED_EDGE('',*,*,#15511,.T.);
#21015=ORIENTED_EDGE('',*,*,#15512,.F.);
#21016=ORIENTED_EDGE('',*,*,#15507,.T.);
#21017=ORIENTED_EDGE('',*,*,#15069,.F.);
#21018=ORIENTED_EDGE('',*,*,#15078,.F.);
#21019=ORIENTED_EDGE('',*,*,#15513,.T.);
#21020=ORIENTED_EDGE('',*,*,#15510,.F.);
#21021=ORIENTED_EDGE('',*,*,#15503,.F.);
#21022=ORIENTED_EDGE('',*,*,#15514,.T.);
#21023=ORIENTED_EDGE('',*,*,#15515,.T.);
#21024=ORIENTED_EDGE('',*,*,#15348,.F.);
#21025=ORIENTED_EDGE('',*,*,#15516,.T.);
#21026=ORIENTED_EDGE('',*,*,#15362,.T.);
#21027=ORIENTED_EDGE('',*,*,#15516,.F.);
#21028=ORIENTED_EDGE('',*,*,#15517,.F.);
#21029=ORIENTED_EDGE('',*,*,#15518,.F.);
#21030=ORIENTED_EDGE('',*,*,#15359,.T.);
#21031=ORIENTED_EDGE('',*,*,#15345,.F.);
#21032=ORIENTED_EDGE('',*,*,#15519,.F.);
#21033=ORIENTED_EDGE('',*,*,#15517,.T.);
#21034=ORIENTED_EDGE('',*,*,#15347,.F.);
#21035=ORIENTED_EDGE('',*,*,#15520,.T.);
#21036=ORIENTED_EDGE('',*,*,#15325,.F.);
#21037=ORIENTED_EDGE('',*,*,#15521,.T.);
#21038=ORIENTED_EDGE('',*,*,#15335,.T.);
#21039=ORIENTED_EDGE('',*,*,#15331,.F.);
#21040=ORIENTED_EDGE('',*,*,#15336,.F.);
#21041=ORIENTED_EDGE('',*,*,#15522,.F.);
#21042=ORIENTED_EDGE('',*,*,#15523,.F.);
#21043=ORIENTED_EDGE('',*,*,#15521,.F.);
#21044=ORIENTED_EDGE('',*,*,#15524,.F.);
#21045=ORIENTED_EDGE('',*,*,#15525,.F.);
#21046=ORIENTED_EDGE('',*,*,#15522,.T.);
#21047=ORIENTED_EDGE('',*,*,#15322,.F.);
#21048=ORIENTED_EDGE('',*,*,#15526,.F.);
#21049=ORIENTED_EDGE('',*,*,#15524,.T.);
#21050=ORIENTED_EDGE('',*,*,#15324,.F.);
#21051=ORIENTED_EDGE('',*,*,#15527,.T.);
#21052=ORIENTED_EDGE('',*,*,#15076,.T.);
#21053=ORIENTED_EDGE('',*,*,#15528,.T.);
#21054=ORIENTED_EDGE('',*,*,#15312,.T.);
#21055=ORIENTED_EDGE('',*,*,#15308,.F.);
#21056=ORIENTED_EDGE('',*,*,#15313,.F.);
#21057=ORIENTED_EDGE('',*,*,#15529,.F.);
#21058=ORIENTED_EDGE('',*,*,#15530,.F.);
#21059=ORIENTED_EDGE('',*,*,#15528,.F.);
#21060=ORIENTED_EDGE('',*,*,#15080,.F.);
#21061=ORIENTED_EDGE('',*,*,#15531,.F.);
#21062=ORIENTED_EDGE('',*,*,#15529,.T.);
#21063=ORIENTED_EDGE('',*,*,#15361,.F.);
#21064=ORIENTED_EDGE('',*,*,#15532,.F.);
#21065=ORIENTED_EDGE('',*,*,#15533,.F.);
#21066=ORIENTED_EDGE('',*,*,#15534,.F.);
#21067=ORIENTED_EDGE('',*,*,#15535,.F.);
#21068=ORIENTED_EDGE('',*,*,#15536,.F.);
#21069=ORIENTED_EDGE('',*,*,#15537,.F.);
#21070=ORIENTED_EDGE('',*,*,#15538,.F.);
#21071=ORIENTED_EDGE('',*,*,#15539,.F.);
#21072=ORIENTED_EDGE('',*,*,#15540,.F.);
#21073=ORIENTED_EDGE('',*,*,#15541,.F.);
#21074=ORIENTED_EDGE('',*,*,#15542,.F.);
#21075=ORIENTED_EDGE('',*,*,#15543,.F.);
#21076=ORIENTED_EDGE('',*,*,#15544,.F.);
#21077=ORIENTED_EDGE('',*,*,#15545,.F.);
#21078=ORIENTED_EDGE('',*,*,#15546,.F.);
#21079=ORIENTED_EDGE('',*,*,#15547,.F.);
#21080=ORIENTED_EDGE('',*,*,#15548,.F.);
#21081=ORIENTED_EDGE('',*,*,#15549,.F.);
#21082=ORIENTED_EDGE('',*,*,#15550,.F.);
#21083=ORIENTED_EDGE('',*,*,#15551,.F.);
#21084=ORIENTED_EDGE('',*,*,#15552,.F.);
#21085=ORIENTED_EDGE('',*,*,#15553,.F.);
#21086=ORIENTED_EDGE('',*,*,#15554,.F.);
#21087=ORIENTED_EDGE('',*,*,#15555,.F.);
#21088=ORIENTED_EDGE('',*,*,#15556,.F.);
#21089=ORIENTED_EDGE('',*,*,#15557,.F.);
#21090=ORIENTED_EDGE('',*,*,#15558,.F.);
#21091=ORIENTED_EDGE('',*,*,#15559,.F.);
#21092=ORIENTED_EDGE('',*,*,#15094,.F.);
#21093=ORIENTED_EDGE('',*,*,#15099,.F.);
#21094=ORIENTED_EDGE('',*,*,#15560,.F.);
#21095=ORIENTED_EDGE('',*,*,#15107,.F.);
#21096=ORIENTED_EDGE('',*,*,#15113,.F.);
#21097=ORIENTED_EDGE('',*,*,#15122,.F.);
#21098=ORIENTED_EDGE('',*,*,#15561,.F.);
#21099=ORIENTED_EDGE('',*,*,#15133,.F.);
#21100=ORIENTED_EDGE('',*,*,#15135,.F.);
#21101=ORIENTED_EDGE('',*,*,#15046,.F.);
#21102=ORIENTED_EDGE('',*,*,#15562,.F.);
#21103=ORIENTED_EDGE('',*,*,#15563,.F.);
#21104=ORIENTED_EDGE('',*,*,#15564,.F.);
#21105=ORIENTED_EDGE('',*,*,#15565,.F.);
#21106=ORIENTED_EDGE('',*,*,#15566,.F.);
#21107=ORIENTED_EDGE('',*,*,#15567,.F.);
#21108=ORIENTED_EDGE('',*,*,#15568,.F.);
#21109=ORIENTED_EDGE('',*,*,#15569,.F.);
#21110=ORIENTED_EDGE('',*,*,#15570,.F.);
#21111=ORIENTED_EDGE('',*,*,#15571,.F.);
#21112=ORIENTED_EDGE('',*,*,#15572,.F.);
#21113=ORIENTED_EDGE('',*,*,#15573,.F.);
#21114=ORIENTED_EDGE('',*,*,#15574,.F.);
#21115=ORIENTED_EDGE('',*,*,#15575,.F.);
#21116=ORIENTED_EDGE('',*,*,#15576,.F.);
#21117=ORIENTED_EDGE('',*,*,#15577,.F.);
#21118=ORIENTED_EDGE('',*,*,#15578,.F.);
#21119=ORIENTED_EDGE('',*,*,#15579,.F.);
#21120=ORIENTED_EDGE('',*,*,#15580,.F.);
#21121=ORIENTED_EDGE('',*,*,#15581,.F.);
#21122=ORIENTED_EDGE('',*,*,#15582,.F.);
#21123=ORIENTED_EDGE('',*,*,#15583,.F.);
#21124=ORIENTED_EDGE('',*,*,#15584,.F.);
#21125=ORIENTED_EDGE('',*,*,#15585,.F.);
#21126=ORIENTED_EDGE('',*,*,#15586,.F.);
#21127=ORIENTED_EDGE('',*,*,#15587,.F.);
#21128=ORIENTED_EDGE('',*,*,#15147,.F.);
#21129=ORIENTED_EDGE('',*,*,#15152,.F.);
#21130=ORIENTED_EDGE('',*,*,#15588,.F.);
#21131=ORIENTED_EDGE('',*,*,#15160,.F.);
#21132=ORIENTED_EDGE('',*,*,#15166,.F.);
#21133=ORIENTED_EDGE('',*,*,#15175,.F.);
#21134=ORIENTED_EDGE('',*,*,#15589,.F.);
#21135=ORIENTED_EDGE('',*,*,#15186,.F.);
#21136=ORIENTED_EDGE('',*,*,#15188,.F.);
#21137=ORIENTED_EDGE('',*,*,#15031,.F.);
#21138=ORIENTED_EDGE('',*,*,#15590,.F.);
#21139=ORIENTED_EDGE('',*,*,#15197,.F.);
#21140=ORIENTED_EDGE('',*,*,#15203,.F.);
#21141=ORIENTED_EDGE('',*,*,#15212,.F.);
#21142=ORIENTED_EDGE('',*,*,#15591,.F.);
#21143=ORIENTED_EDGE('',*,*,#15223,.F.);
#21144=ORIENTED_EDGE('',*,*,#15228,.F.);
#21145=ORIENTED_EDGE('',*,*,#15592,.F.);
#21146=ORIENTED_EDGE('',*,*,#15593,.F.);
#21147=ORIENTED_EDGE('',*,*,#15250,.F.);
#21148=ORIENTED_EDGE('',*,*,#15256,.F.);
#21149=ORIENTED_EDGE('',*,*,#15265,.F.);
#21150=ORIENTED_EDGE('',*,*,#15594,.F.);
#21151=ORIENTED_EDGE('',*,*,#15273,.F.);
#21152=ORIENTED_EDGE('',*,*,#15279,.F.);
#21153=ORIENTED_EDGE('',*,*,#15288,.F.);
#21154=ORIENTED_EDGE('',*,*,#15595,.F.);
#21155=ORIENTED_EDGE('',*,*,#15302,.F.);
#21156=ORIENTED_EDGE('',*,*,#15596,.F.);
#21157=ORIENTED_EDGE('',*,*,#15384,.F.);
#21158=ORIENTED_EDGE('',*,*,#15391,.F.);
#21159=ORIENTED_EDGE('',*,*,#15400,.F.);
#21160=ORIENTED_EDGE('',*,*,#15406,.F.);
#21161=ORIENTED_EDGE('',*,*,#15597,.F.);
#21162=ORIENTED_EDGE('',*,*,#15598,.F.);
#21163=ORIENTED_EDGE('',*,*,#15599,.F.);
#21164=ORIENTED_EDGE('',*,*,#15600,.F.);
#21165=ORIENTED_EDGE('',*,*,#15601,.F.);
#21166=ORIENTED_EDGE('',*,*,#15602,.F.);
#21167=ORIENTED_EDGE('',*,*,#15416,.F.);
#21168=ORIENTED_EDGE('',*,*,#15422,.F.);
#21169=ORIENTED_EDGE('',*,*,#15431,.F.);
#21170=ORIENTED_EDGE('',*,*,#15603,.F.);
#21171=ORIENTED_EDGE('',*,*,#15439,.F.);
#21172=ORIENTED_EDGE('',*,*,#15445,.F.);
#21173=ORIENTED_EDGE('',*,*,#15454,.F.);
#21174=ORIENTED_EDGE('',*,*,#15604,.F.);
#21175=ORIENTED_EDGE('',*,*,#15462,.F.);
#21176=ORIENTED_EDGE('',*,*,#15468,.F.);
#21177=ORIENTED_EDGE('',*,*,#15477,.F.);
#21178=ORIENTED_EDGE('',*,*,#15605,.F.);
#21179=ORIENTED_EDGE('',*,*,#15485,.F.);
#21180=ORIENTED_EDGE('',*,*,#15491,.F.);
#21181=ORIENTED_EDGE('',*,*,#15500,.F.);
#21182=ORIENTED_EDGE('',*,*,#15606,.F.);
#21183=ORIENTED_EDGE('',*,*,#15511,.F.);
#21184=ORIENTED_EDGE('',*,*,#15513,.F.);
#21185=ORIENTED_EDGE('',*,*,#15077,.F.);
#21186=ORIENTED_EDGE('',*,*,#15527,.F.);
#21187=ORIENTED_EDGE('',*,*,#15311,.F.);
#21188=ORIENTED_EDGE('',*,*,#15317,.F.);
#21189=ORIENTED_EDGE('',*,*,#15326,.F.);
#21190=ORIENTED_EDGE('',*,*,#15520,.F.);
#21191=ORIENTED_EDGE('',*,*,#15334,.F.);
#21192=ORIENTED_EDGE('',*,*,#15340,.F.);
#21193=ORIENTED_EDGE('',*,*,#15349,.F.);
#21194=ORIENTED_EDGE('',*,*,#15515,.F.);
#21195=ORIENTED_EDGE('',*,*,#15606,.T.);
#21196=ORIENTED_EDGE('',*,*,#15499,.F.);
#21197=ORIENTED_EDGE('',*,*,#15607,.T.);
#21198=ORIENTED_EDGE('',*,*,#15512,.T.);
#21199=ORIENTED_EDGE('',*,*,#15607,.F.);
#21200=ORIENTED_EDGE('',*,*,#15608,.F.);
#21201=ORIENTED_EDGE('',*,*,#15609,.F.);
#21202=ORIENTED_EDGE('',*,*,#15508,.T.);
#21203=ORIENTED_EDGE('',*,*,#15496,.F.);
#21204=ORIENTED_EDGE('',*,*,#15610,.F.);
#21205=ORIENTED_EDGE('',*,*,#15608,.T.);
#21206=ORIENTED_EDGE('',*,*,#15498,.F.);
#21207=ORIENTED_EDGE('',*,*,#15605,.T.);
#21208=ORIENTED_EDGE('',*,*,#15476,.F.);
#21209=ORIENTED_EDGE('',*,*,#15611,.T.);
#21210=ORIENTED_EDGE('',*,*,#15486,.T.);
#21211=ORIENTED_EDGE('',*,*,#15482,.F.);
#21212=ORIENTED_EDGE('',*,*,#15487,.F.);
#21213=ORIENTED_EDGE('',*,*,#15612,.F.);
#21214=ORIENTED_EDGE('',*,*,#15613,.F.);
#21215=ORIENTED_EDGE('',*,*,#15611,.F.);
#21216=ORIENTED_EDGE('',*,*,#15614,.F.);
#21217=ORIENTED_EDGE('',*,*,#15615,.F.);
#21218=ORIENTED_EDGE('',*,*,#15612,.T.);
#21219=ORIENTED_EDGE('',*,*,#15473,.F.);
#21220=ORIENTED_EDGE('',*,*,#15616,.F.);
#21221=ORIENTED_EDGE('',*,*,#15614,.T.);
#21222=ORIENTED_EDGE('',*,*,#15475,.F.);
#21223=ORIENTED_EDGE('',*,*,#15604,.T.);
#21224=ORIENTED_EDGE('',*,*,#15453,.F.);
#21225=ORIENTED_EDGE('',*,*,#15617,.T.);
#21226=ORIENTED_EDGE('',*,*,#15463,.T.);
#21227=ORIENTED_EDGE('',*,*,#15459,.F.);
#21228=ORIENTED_EDGE('',*,*,#15464,.F.);
#21229=ORIENTED_EDGE('',*,*,#15618,.F.);
#21230=ORIENTED_EDGE('',*,*,#15619,.F.);
#21231=ORIENTED_EDGE('',*,*,#15617,.F.);
#21232=ORIENTED_EDGE('',*,*,#15620,.F.);
#21233=ORIENTED_EDGE('',*,*,#15621,.F.);
#21234=ORIENTED_EDGE('',*,*,#15618,.T.);
#21235=ORIENTED_EDGE('',*,*,#15450,.F.);
#21236=ORIENTED_EDGE('',*,*,#15622,.F.);
#21237=ORIENTED_EDGE('',*,*,#15620,.T.);
#21238=ORIENTED_EDGE('',*,*,#15452,.F.);
#21239=ORIENTED_EDGE('',*,*,#15603,.T.);
#21240=ORIENTED_EDGE('',*,*,#15430,.F.);
#21241=ORIENTED_EDGE('',*,*,#15623,.T.);
#21242=ORIENTED_EDGE('',*,*,#15440,.T.);
#21243=ORIENTED_EDGE('',*,*,#15436,.F.);
#21244=ORIENTED_EDGE('',*,*,#15441,.F.);
#21245=ORIENTED_EDGE('',*,*,#15624,.F.);
#21246=ORIENTED_EDGE('',*,*,#15625,.F.);
#21247=ORIENTED_EDGE('',*,*,#15623,.F.);
#21248=ORIENTED_EDGE('',*,*,#15626,.F.);
#21249=ORIENTED_EDGE('',*,*,#15627,.F.);
#21250=ORIENTED_EDGE('',*,*,#15624,.T.);
#21251=ORIENTED_EDGE('',*,*,#15427,.F.);
#21252=ORIENTED_EDGE('',*,*,#15628,.F.);
#21253=ORIENTED_EDGE('',*,*,#15626,.T.);
#21254=ORIENTED_EDGE('',*,*,#15429,.F.);
#21255=ORIENTED_EDGE('',*,*,#15602,.T.);
#21256=ORIENTED_EDGE('',*,*,#15629,.T.);
#21257=ORIENTED_EDGE('',*,*,#15630,.T.);
#21258=ORIENTED_EDGE('',*,*,#15417,.T.);
#21259=ORIENTED_EDGE('',*,*,#15413,.F.);
#21260=ORIENTED_EDGE('',*,*,#15418,.F.);
#21261=ORIENTED_EDGE('',*,*,#15631,.F.);
#21262=ORIENTED_EDGE('',*,*,#15632,.F.);
#21263=ORIENTED_EDGE('',*,*,#15630,.F.);
#21264=ORIENTED_EDGE('',*,*,#15633,.F.);
#21265=ORIENTED_EDGE('',*,*,#15634,.F.);
#21266=ORIENTED_EDGE('',*,*,#15631,.T.);
#21267=ORIENTED_EDGE('',*,*,#15635,.T.);
#21268=ORIENTED_EDGE('',*,*,#15636,.T.);
#21269=ORIENTED_EDGE('',*,*,#15637,.T.);
#21270=ORIENTED_EDGE('',*,*,#15638,.T.);
#21271=ORIENTED_EDGE('',*,*,#15637,.F.);
#21272=ORIENTED_EDGE('',*,*,#15639,.T.);
#21273=ORIENTED_EDGE('',*,*,#15640,.F.);
#21274=ORIENTED_EDGE('',*,*,#15641,.F.);
#21275=ORIENTED_EDGE('',*,*,#15642,.T.);
#21276=ORIENTED_EDGE('',*,*,#15636,.F.);
#21277=ORIENTED_EDGE('',*,*,#15643,.T.);
#21278=ORIENTED_EDGE('',*,*,#15644,.F.);
#21279=ORIENTED_EDGE('',*,*,#15639,.F.);
#21280=ORIENTED_EDGE('',*,*,#15645,.T.);
#21281=ORIENTED_EDGE('',*,*,#15644,.T.);
#21282=ORIENTED_EDGE('',*,*,#15401,.T.);
#21283=ORIENTED_EDGE('',*,*,#15389,.T.);
#21284=ORIENTED_EDGE('',*,*,#15646,.T.);
#21285=ORIENTED_EDGE('',*,*,#15647,.T.);
#21286=ORIENTED_EDGE('',*,*,#15395,.F.);
#21287=ORIENTED_EDGE('',*,*,#15640,.T.);
#21288=ORIENTED_EDGE('',*,*,#15645,.F.);
#21289=ORIENTED_EDGE('',*,*,#15648,.T.);
#21290=ORIENTED_EDGE('',*,*,#15649,.T.);
#21291=ORIENTED_EDGE('',*,*,#15650,.T.);
#21292=ORIENTED_EDGE('',*,*,#15378,.F.);
#21293=ORIENTED_EDGE('',*,*,#15651,.F.);
#21294=ORIENTED_EDGE('',*,*,#15652,.T.);
#21295=ORIENTED_EDGE('',*,*,#15648,.F.);
#21296=ORIENTED_EDGE('',*,*,#15647,.F.);
#21297=ORIENTED_EDGE('',*,*,#15653,.T.);
#21298=ORIENTED_EDGE('',*,*,#15404,.T.);
#21299=ORIENTED_EDGE('',*,*,#15408,.T.);
#21300=ORIENTED_EDGE('',*,*,#15654,.T.);
#21301=ORIENTED_EDGE('',*,*,#15655,.T.);
#21302=ORIENTED_EDGE('',*,*,#15656,.T.);
#21303=ORIENTED_EDGE('',*,*,#15657,.T.);
#21304=ORIENTED_EDGE('',*,*,#15657,.F.);
#21305=ORIENTED_EDGE('',*,*,#15658,.T.);
#21306=ORIENTED_EDGE('',*,*,#15659,.T.);
#21307=ORIENTED_EDGE('',*,*,#15597,.T.);
#21308=ORIENTED_EDGE('',*,*,#15405,.T.);
#21309=ORIENTED_EDGE('',*,*,#15660,.T.);
#21310=ORIENTED_EDGE('',*,*,#15661,.T.);
#21311=ORIENTED_EDGE('',*,*,#15662,.T.);
#21312=ORIENTED_EDGE('',*,*,#15663,.T.);
#21313=ORIENTED_EDGE('',*,*,#15664,.T.);
#21314=ORIENTED_EDGE('',*,*,#15665,.T.);
#21315=ORIENTED_EDGE('',*,*,#15663,.F.);
#21316=ORIENTED_EDGE('',*,*,#15666,.T.);
#21317=ORIENTED_EDGE('',*,*,#15599,.T.);
#21318=ORIENTED_EDGE('',*,*,#15667,.F.);
#21319=ORIENTED_EDGE('',*,*,#15668,.T.);
#21320=ORIENTED_EDGE('',*,*,#15662,.F.);
#21321=ORIENTED_EDGE('',*,*,#15669,.T.);
#21322=ORIENTED_EDGE('',*,*,#15670,.F.);
#21323=ORIENTED_EDGE('',*,*,#15671,.F.);
#21324=ORIENTED_EDGE('',*,*,#15600,.T.);
#21325=ORIENTED_EDGE('',*,*,#15666,.F.);
#21326=ORIENTED_EDGE('',*,*,#15661,.F.);
#21327=ORIENTED_EDGE('',*,*,#15672,.F.);
#21328=ORIENTED_EDGE('',*,*,#15673,.F.);
#21329=ORIENTED_EDGE('',*,*,#15669,.F.);
#21330=ORIENTED_EDGE('',*,*,#15670,.T.);
#21331=ORIENTED_EDGE('',*,*,#15673,.T.);
#21332=ORIENTED_EDGE('',*,*,#15674,.T.);
#21333=ORIENTED_EDGE('',*,*,#15675,.T.);
#21334=ORIENTED_EDGE('',*,*,#15676,.T.);
#21335=ORIENTED_EDGE('',*,*,#15677,.T.);
#21336=ORIENTED_EDGE('',*,*,#15677,.F.);
#21337=ORIENTED_EDGE('',*,*,#15678,.T.);
#21338=ORIENTED_EDGE('',*,*,#15629,.F.);
#21339=ORIENTED_EDGE('',*,*,#15601,.T.);
#21340=ORIENTED_EDGE('',*,*,#15671,.T.);
#21341=ORIENTED_EDGE('',*,*,#15676,.F.);
#21342=ORIENTED_EDGE('',*,*,#15679,.F.);
#21343=ORIENTED_EDGE('',*,*,#15633,.T.);
#21344=ORIENTED_EDGE('',*,*,#15678,.F.);
#21345=ORIENTED_EDGE('',*,*,#15598,.T.);
#21346=ORIENTED_EDGE('',*,*,#15659,.F.);
#21347=ORIENTED_EDGE('',*,*,#15680,.T.);
#21348=ORIENTED_EDGE('',*,*,#15667,.T.);
#21349=ORIENTED_EDGE('',*,*,#15664,.F.);
#21350=ORIENTED_EDGE('',*,*,#15668,.F.);
#21351=ORIENTED_EDGE('',*,*,#15681,.F.);
#21352=ORIENTED_EDGE('',*,*,#15682,.F.);
#21353=ORIENTED_EDGE('',*,*,#15680,.F.);
#21354=ORIENTED_EDGE('',*,*,#15683,.F.);
#21355=ORIENTED_EDGE('',*,*,#15684,.F.);
#21356=ORIENTED_EDGE('',*,*,#15681,.T.);
#21357=ORIENTED_EDGE('',*,*,#15656,.F.);
#21358=ORIENTED_EDGE('',*,*,#15685,.F.);
#21359=ORIENTED_EDGE('',*,*,#15683,.T.);
#21360=ORIENTED_EDGE('',*,*,#15658,.F.);
#21361=ORIENTED_EDGE('',*,*,#15595,.T.);
#21362=ORIENTED_EDGE('',*,*,#15287,.F.);
#21363=ORIENTED_EDGE('',*,*,#15686,.T.);
#21364=ORIENTED_EDGE('',*,*,#15303,.T.);
#21365=ORIENTED_EDGE('',*,*,#15686,.F.);
#21366=ORIENTED_EDGE('',*,*,#15687,.F.);
#21367=ORIENTED_EDGE('',*,*,#15688,.F.);
#21368=ORIENTED_EDGE('',*,*,#15300,.T.);
#21369=ORIENTED_EDGE('',*,*,#15284,.F.);
#21370=ORIENTED_EDGE('',*,*,#15689,.F.);
#21371=ORIENTED_EDGE('',*,*,#15687,.T.);
#21372=ORIENTED_EDGE('',*,*,#15286,.F.);
#21373=ORIENTED_EDGE('',*,*,#15594,.T.);
#21374=ORIENTED_EDGE('',*,*,#15264,.F.);
#21375=ORIENTED_EDGE('',*,*,#15690,.T.);
#21376=ORIENTED_EDGE('',*,*,#15274,.T.);
#21377=ORIENTED_EDGE('',*,*,#15270,.F.);
#21378=ORIENTED_EDGE('',*,*,#15275,.F.);
#21379=ORIENTED_EDGE('',*,*,#15691,.F.);
#21380=ORIENTED_EDGE('',*,*,#15692,.F.);
#21381=ORIENTED_EDGE('',*,*,#15690,.F.);
#21382=ORIENTED_EDGE('',*,*,#15693,.F.);
#21383=ORIENTED_EDGE('',*,*,#15694,.F.);
#21384=ORIENTED_EDGE('',*,*,#15691,.T.);
#21385=ORIENTED_EDGE('',*,*,#15261,.F.);
#21386=ORIENTED_EDGE('',*,*,#15695,.F.);
#21387=ORIENTED_EDGE('',*,*,#15693,.T.);
#21388=ORIENTED_EDGE('',*,*,#15263,.F.);
#21389=ORIENTED_EDGE('',*,*,#15233,.F.);
#21390=ORIENTED_EDGE('',*,*,#15236,.T.);
#21391=ORIENTED_EDGE('',*,*,#15696,.T.);
#21392=ORIENTED_EDGE('',*,*,#15592,.T.);
#21393=ORIENTED_EDGE('',*,*,#15227,.T.);
#21394=ORIENTED_EDGE('',*,*,#15593,.T.);
#21395=ORIENTED_EDGE('',*,*,#15696,.F.);
#21396=ORIENTED_EDGE('',*,*,#15697,.T.);
#21397=ORIENTED_EDGE('',*,*,#15251,.T.);
#21398=ORIENTED_EDGE('',*,*,#15247,.F.);
#21399=ORIENTED_EDGE('',*,*,#15252,.F.);
#21400=ORIENTED_EDGE('',*,*,#15698,.F.);
#21401=ORIENTED_EDGE('',*,*,#15699,.F.);
#21402=ORIENTED_EDGE('',*,*,#15697,.F.);
#21403=ORIENTED_EDGE('',*,*,#15235,.F.);
#21404=ORIENTED_EDGE('',*,*,#15700,.F.);
#21405=ORIENTED_EDGE('',*,*,#15698,.T.);
#21406=ORIENTED_EDGE('',*,*,#15591,.T.);
#21407=ORIENTED_EDGE('',*,*,#15211,.F.);
#21408=ORIENTED_EDGE('',*,*,#15701,.T.);
#21409=ORIENTED_EDGE('',*,*,#15224,.T.);
#21410=ORIENTED_EDGE('',*,*,#15701,.F.);
#21411=ORIENTED_EDGE('',*,*,#15702,.F.);
#21412=ORIENTED_EDGE('',*,*,#15703,.F.);
#21413=ORIENTED_EDGE('',*,*,#15220,.T.);
#21414=ORIENTED_EDGE('',*,*,#15208,.F.);
#21415=ORIENTED_EDGE('',*,*,#15704,.F.);
#21416=ORIENTED_EDGE('',*,*,#15702,.T.);
#21417=ORIENTED_EDGE('',*,*,#15210,.F.);
#21418=ORIENTED_EDGE('',*,*,#15590,.T.);
#21419=ORIENTED_EDGE('',*,*,#15030,.T.);
#21420=ORIENTED_EDGE('',*,*,#15705,.T.);
#21421=ORIENTED_EDGE('',*,*,#15198,.T.);
#21422=ORIENTED_EDGE('',*,*,#15194,.F.);
#21423=ORIENTED_EDGE('',*,*,#15199,.F.);
#21424=ORIENTED_EDGE('',*,*,#15706,.F.);
#21425=ORIENTED_EDGE('',*,*,#15707,.F.);
#21426=ORIENTED_EDGE('',*,*,#15705,.F.);
#21427=ORIENTED_EDGE('',*,*,#15034,.F.);
#21428=ORIENTED_EDGE('',*,*,#15708,.F.);
#21429=ORIENTED_EDGE('',*,*,#15706,.T.);
#21430=ORIENTED_EDGE('',*,*,#15589,.T.);
#21431=ORIENTED_EDGE('',*,*,#15174,.F.);
#21432=ORIENTED_EDGE('',*,*,#15709,.T.);
#21433=ORIENTED_EDGE('',*,*,#15187,.T.);
#21434=ORIENTED_EDGE('',*,*,#15709,.F.);
#21435=ORIENTED_EDGE('',*,*,#15710,.F.);
#21436=ORIENTED_EDGE('',*,*,#15711,.F.);
#21437=ORIENTED_EDGE('',*,*,#15183,.T.);
#21438=ORIENTED_EDGE('',*,*,#15171,.F.);
#21439=ORIENTED_EDGE('',*,*,#15712,.F.);
#21440=ORIENTED_EDGE('',*,*,#15710,.T.);
#21441=ORIENTED_EDGE('',*,*,#15173,.F.);
#21442=ORIENTED_EDGE('',*,*,#15588,.T.);
#21443=ORIENTED_EDGE('',*,*,#15151,.F.);
#21444=ORIENTED_EDGE('',*,*,#15713,.T.);
#21445=ORIENTED_EDGE('',*,*,#15161,.T.);
#21446=ORIENTED_EDGE('',*,*,#15157,.F.);
#21447=ORIENTED_EDGE('',*,*,#15162,.F.);
#21448=ORIENTED_EDGE('',*,*,#15714,.F.);
#21449=ORIENTED_EDGE('',*,*,#15715,.F.);
#21450=ORIENTED_EDGE('',*,*,#15713,.F.);
#21451=ORIENTED_EDGE('',*,*,#15716,.F.);
#21452=ORIENTED_EDGE('',*,*,#15717,.F.);
#21453=ORIENTED_EDGE('',*,*,#15714,.T.);
#21454=ORIENTED_EDGE('',*,*,#15141,.F.);
#21455=ORIENTED_EDGE('',*,*,#15718,.F.);
#21456=ORIENTED_EDGE('',*,*,#15716,.T.);
#21457=ORIENTED_EDGE('',*,*,#15150,.F.);
#21458=ORIENTED_EDGE('',*,*,#15719,.T.);
#21459=ORIENTED_EDGE('',*,*,#15720,.T.);
#21460=ORIENTED_EDGE('',*,*,#15721,.T.);
#21461=ORIENTED_EDGE('',*,*,#15722,.T.);
#21462=ORIENTED_EDGE('',*,*,#15723,.T.);
#21463=ORIENTED_EDGE('',*,*,#15724,.T.);
#21464=ORIENTED_EDGE('',*,*,#15722,.F.);
#21465=ORIENTED_EDGE('',*,*,#15725,.T.);
#21466=ORIENTED_EDGE('',*,*,#15563,.T.);
#21467=ORIENTED_EDGE('',*,*,#15726,.F.);
#21468=ORIENTED_EDGE('',*,*,#15727,.T.);
#21469=ORIENTED_EDGE('',*,*,#15721,.F.);
#21470=ORIENTED_EDGE('',*,*,#15728,.T.);
#21471=ORIENTED_EDGE('',*,*,#15729,.F.);
#21472=ORIENTED_EDGE('',*,*,#15730,.F.);
#21473=ORIENTED_EDGE('',*,*,#15564,.T.);
#21474=ORIENTED_EDGE('',*,*,#15725,.F.);
#21475=ORIENTED_EDGE('',*,*,#15720,.F.);
#21476=ORIENTED_EDGE('',*,*,#15731,.F.);
#21477=ORIENTED_EDGE('',*,*,#15732,.F.);
#21478=ORIENTED_EDGE('',*,*,#15728,.F.);
#21479=ORIENTED_EDGE('',*,*,#15729,.T.);
#21480=ORIENTED_EDGE('',*,*,#15732,.T.);
#21481=ORIENTED_EDGE('',*,*,#15733,.T.);
#21482=ORIENTED_EDGE('',*,*,#15734,.T.);
#21483=ORIENTED_EDGE('',*,*,#15735,.T.);
#21484=ORIENTED_EDGE('',*,*,#15736,.T.);
#21485=ORIENTED_EDGE('',*,*,#15736,.F.);
#21486=ORIENTED_EDGE('',*,*,#15737,.T.);
#21487=ORIENTED_EDGE('',*,*,#15738,.T.);
#21488=ORIENTED_EDGE('',*,*,#15565,.T.);
#21489=ORIENTED_EDGE('',*,*,#15730,.T.);
#21490=ORIENTED_EDGE('',*,*,#15739,.T.);
#21491=ORIENTED_EDGE('',*,*,#15740,.T.);
#21492=ORIENTED_EDGE('',*,*,#15741,.T.);
#21493=ORIENTED_EDGE('',*,*,#15742,.T.);
#21494=ORIENTED_EDGE('',*,*,#15743,.T.);
#21495=ORIENTED_EDGE('',*,*,#15744,.T.);
#21496=ORIENTED_EDGE('',*,*,#15742,.F.);
#21497=ORIENTED_EDGE('',*,*,#15745,.T.);
#21498=ORIENTED_EDGE('',*,*,#15567,.T.);
#21499=ORIENTED_EDGE('',*,*,#15746,.F.);
#21500=ORIENTED_EDGE('',*,*,#15747,.T.);
#21501=ORIENTED_EDGE('',*,*,#15741,.F.);
#21502=ORIENTED_EDGE('',*,*,#15748,.T.);
#21503=ORIENTED_EDGE('',*,*,#15749,.F.);
#21504=ORIENTED_EDGE('',*,*,#15750,.F.);
#21505=ORIENTED_EDGE('',*,*,#15568,.T.);
#21506=ORIENTED_EDGE('',*,*,#15745,.F.);
#21507=ORIENTED_EDGE('',*,*,#15740,.F.);
#21508=ORIENTED_EDGE('',*,*,#15751,.F.);
#21509=ORIENTED_EDGE('',*,*,#15752,.F.);
#21510=ORIENTED_EDGE('',*,*,#15748,.F.);
#21511=ORIENTED_EDGE('',*,*,#15749,.T.);
#21512=ORIENTED_EDGE('',*,*,#15752,.T.);
#21513=ORIENTED_EDGE('',*,*,#15753,.T.);
#21514=ORIENTED_EDGE('',*,*,#15754,.T.);
#21515=ORIENTED_EDGE('',*,*,#15755,.T.);
#21516=ORIENTED_EDGE('',*,*,#15756,.T.);
#21517=ORIENTED_EDGE('',*,*,#15756,.F.);
#21518=ORIENTED_EDGE('',*,*,#15757,.T.);
#21519=ORIENTED_EDGE('',*,*,#15758,.T.);
#21520=ORIENTED_EDGE('',*,*,#15569,.T.);
#21521=ORIENTED_EDGE('',*,*,#15750,.T.);
#21522=ORIENTED_EDGE('',*,*,#15759,.T.);
#21523=ORIENTED_EDGE('',*,*,#15760,.T.);
#21524=ORIENTED_EDGE('',*,*,#15761,.T.);
#21525=ORIENTED_EDGE('',*,*,#15762,.T.);
#21526=ORIENTED_EDGE('',*,*,#15763,.T.);
#21527=ORIENTED_EDGE('',*,*,#15764,.T.);
#21528=ORIENTED_EDGE('',*,*,#15762,.F.);
#21529=ORIENTED_EDGE('',*,*,#15765,.T.);
#21530=ORIENTED_EDGE('',*,*,#15571,.T.);
#21531=ORIENTED_EDGE('',*,*,#15766,.F.);
#21532=ORIENTED_EDGE('',*,*,#15767,.T.);
#21533=ORIENTED_EDGE('',*,*,#15761,.F.);
#21534=ORIENTED_EDGE('',*,*,#15768,.T.);
#21535=ORIENTED_EDGE('',*,*,#15769,.F.);
#21536=ORIENTED_EDGE('',*,*,#15770,.F.);
#21537=ORIENTED_EDGE('',*,*,#15572,.T.);
#21538=ORIENTED_EDGE('',*,*,#15765,.F.);
#21539=ORIENTED_EDGE('',*,*,#15760,.F.);
#21540=ORIENTED_EDGE('',*,*,#15771,.F.);
#21541=ORIENTED_EDGE('',*,*,#15772,.F.);
#21542=ORIENTED_EDGE('',*,*,#15768,.F.);
#21543=ORIENTED_EDGE('',*,*,#15769,.T.);
#21544=ORIENTED_EDGE('',*,*,#15772,.T.);
#21545=ORIENTED_EDGE('',*,*,#15773,.T.);
#21546=ORIENTED_EDGE('',*,*,#15774,.T.);
#21547=ORIENTED_EDGE('',*,*,#15775,.T.);
#21548=ORIENTED_EDGE('',*,*,#15776,.T.);
#21549=ORIENTED_EDGE('',*,*,#15776,.F.);
#21550=ORIENTED_EDGE('',*,*,#15777,.T.);
#21551=ORIENTED_EDGE('',*,*,#15778,.T.);
#21552=ORIENTED_EDGE('',*,*,#15573,.T.);
#21553=ORIENTED_EDGE('',*,*,#15770,.T.);
#21554=ORIENTED_EDGE('',*,*,#15779,.T.);
#21555=ORIENTED_EDGE('',*,*,#15780,.T.);
#21556=ORIENTED_EDGE('',*,*,#15781,.T.);
#21557=ORIENTED_EDGE('',*,*,#15782,.T.);
#21558=ORIENTED_EDGE('',*,*,#15783,.T.);
#21559=ORIENTED_EDGE('',*,*,#15784,.T.);
#21560=ORIENTED_EDGE('',*,*,#15783,.F.);
#21561=ORIENTED_EDGE('',*,*,#15785,.F.);
#21562=ORIENTED_EDGE('',*,*,#15786,.F.);
#21563=ORIENTED_EDGE('',*,*,#15787,.F.);
#21564=ORIENTED_EDGE('',*,*,#15782,.F.);
#21565=ORIENTED_EDGE('',*,*,#15788,.T.);
#21566=ORIENTED_EDGE('',*,*,#15575,.T.);
#21567=ORIENTED_EDGE('',*,*,#15789,.F.);
#21568=ORIENTED_EDGE('',*,*,#15785,.T.);
#21569=ORIENTED_EDGE('',*,*,#15781,.F.);
#21570=ORIENTED_EDGE('',*,*,#15790,.T.);
#21571=ORIENTED_EDGE('',*,*,#15791,.F.);
#21572=ORIENTED_EDGE('',*,*,#15792,.F.);
#21573=ORIENTED_EDGE('',*,*,#15576,.T.);
#21574=ORIENTED_EDGE('',*,*,#15788,.F.);
#21575=ORIENTED_EDGE('',*,*,#15791,.T.);
#21576=ORIENTED_EDGE('',*,*,#15793,.T.);
#21577=ORIENTED_EDGE('',*,*,#15794,.T.);
#21578=ORIENTED_EDGE('',*,*,#15795,.T.);
#21579=ORIENTED_EDGE('',*,*,#15796,.T.);
#21580=ORIENTED_EDGE('',*,*,#15797,.T.);
#21581=ORIENTED_EDGE('',*,*,#15796,.F.);
#21582=ORIENTED_EDGE('',*,*,#15798,.F.);
#21583=ORIENTED_EDGE('',*,*,#15799,.T.);
#21584=ORIENTED_EDGE('',*,*,#15800,.F.);
#21585=ORIENTED_EDGE('',*,*,#15795,.F.);
#21586=ORIENTED_EDGE('',*,*,#15801,.T.);
#21587=ORIENTED_EDGE('',*,*,#15802,.T.);
#21588=ORIENTED_EDGE('',*,*,#15803,.T.);
#21589=ORIENTED_EDGE('',*,*,#15798,.T.);
#21590=ORIENTED_EDGE('',*,*,#15779,.F.);
#21591=ORIENTED_EDGE('',*,*,#15804,.F.);
#21592=ORIENTED_EDGE('',*,*,#15805,.T.);
#21593=ORIENTED_EDGE('',*,*,#15801,.F.);
#21594=ORIENTED_EDGE('',*,*,#15794,.F.);
#21595=ORIENTED_EDGE('',*,*,#15806,.T.);
#21596=ORIENTED_EDGE('',*,*,#15807,.T.);
#21597=ORIENTED_EDGE('',*,*,#15808,.T.);
#21598=ORIENTED_EDGE('',*,*,#15809,.T.);
#21599=ORIENTED_EDGE('',*,*,#15810,.T.);
#21600=ORIENTED_EDGE('',*,*,#15811,.T.);
#21601=ORIENTED_EDGE('',*,*,#15812,.T.);
#21602=ORIENTED_EDGE('',*,*,#15810,.F.);
#21603=ORIENTED_EDGE('',*,*,#15813,.T.);
#21604=ORIENTED_EDGE('',*,*,#15579,.T.);
#21605=ORIENTED_EDGE('',*,*,#15814,.F.);
#21606=ORIENTED_EDGE('',*,*,#15815,.T.);
#21607=ORIENTED_EDGE('',*,*,#15809,.F.);
#21608=ORIENTED_EDGE('',*,*,#15816,.T.);
#21609=ORIENTED_EDGE('',*,*,#15817,.F.);
#21610=ORIENTED_EDGE('',*,*,#15818,.F.);
#21611=ORIENTED_EDGE('',*,*,#15580,.T.);
#21612=ORIENTED_EDGE('',*,*,#15813,.F.);
#21613=ORIENTED_EDGE('',*,*,#15808,.F.);
#21614=ORIENTED_EDGE('',*,*,#15819,.F.);
#21615=ORIENTED_EDGE('',*,*,#15820,.F.);
#21616=ORIENTED_EDGE('',*,*,#15816,.F.);
#21617=ORIENTED_EDGE('',*,*,#15817,.T.);
#21618=ORIENTED_EDGE('',*,*,#15820,.T.);
#21619=ORIENTED_EDGE('',*,*,#15821,.T.);
#21620=ORIENTED_EDGE('',*,*,#15822,.T.);
#21621=ORIENTED_EDGE('',*,*,#15823,.T.);
#21622=ORIENTED_EDGE('',*,*,#15824,.T.);
#21623=ORIENTED_EDGE('',*,*,#15824,.F.);
#21624=ORIENTED_EDGE('',*,*,#15825,.T.);
#21625=ORIENTED_EDGE('',*,*,#15826,.T.);
#21626=ORIENTED_EDGE('',*,*,#15581,.T.);
#21627=ORIENTED_EDGE('',*,*,#15818,.T.);
#21628=ORIENTED_EDGE('',*,*,#15827,.T.);
#21629=ORIENTED_EDGE('',*,*,#15828,.T.);
#21630=ORIENTED_EDGE('',*,*,#15829,.T.);
#21631=ORIENTED_EDGE('',*,*,#15830,.T.);
#21632=ORIENTED_EDGE('',*,*,#15831,.T.);
#21633=ORIENTED_EDGE('',*,*,#15832,.T.);
#21634=ORIENTED_EDGE('',*,*,#15830,.F.);
#21635=ORIENTED_EDGE('',*,*,#15833,.T.);
#21636=ORIENTED_EDGE('',*,*,#15583,.T.);
#21637=ORIENTED_EDGE('',*,*,#15834,.F.);
#21638=ORIENTED_EDGE('',*,*,#15835,.T.);
#21639=ORIENTED_EDGE('',*,*,#15829,.F.);
#21640=ORIENTED_EDGE('',*,*,#15836,.T.);
#21641=ORIENTED_EDGE('',*,*,#15837,.F.);
#21642=ORIENTED_EDGE('',*,*,#15838,.F.);
#21643=ORIENTED_EDGE('',*,*,#15584,.T.);
#21644=ORIENTED_EDGE('',*,*,#15833,.F.);
#21645=ORIENTED_EDGE('',*,*,#15828,.F.);
#21646=ORIENTED_EDGE('',*,*,#15839,.F.);
#21647=ORIENTED_EDGE('',*,*,#15840,.F.);
#21648=ORIENTED_EDGE('',*,*,#15836,.F.);
#21649=ORIENTED_EDGE('',*,*,#15837,.T.);
#21650=ORIENTED_EDGE('',*,*,#15840,.T.);
#21651=ORIENTED_EDGE('',*,*,#15841,.T.);
#21652=ORIENTED_EDGE('',*,*,#15842,.T.);
#21653=ORIENTED_EDGE('',*,*,#15843,.T.);
#21654=ORIENTED_EDGE('',*,*,#15844,.T.);
#21655=ORIENTED_EDGE('',*,*,#15844,.F.);
#21656=ORIENTED_EDGE('',*,*,#15845,.T.);
#21657=ORIENTED_EDGE('',*,*,#15846,.T.);
#21658=ORIENTED_EDGE('',*,*,#15585,.T.);
#21659=ORIENTED_EDGE('',*,*,#15838,.T.);
#21660=ORIENTED_EDGE('',*,*,#15847,.T.);
#21661=ORIENTED_EDGE('',*,*,#15144,.T.);
#21662=ORIENTED_EDGE('',*,*,#15149,.T.);
#21663=ORIENTED_EDGE('',*,*,#15848,.T.);
#21664=ORIENTED_EDGE('',*,*,#15849,.T.);
#21665=ORIENTED_EDGE('',*,*,#15850,.T.);
#21666=ORIENTED_EDGE('',*,*,#15850,.F.);
#21667=ORIENTED_EDGE('',*,*,#15851,.T.);
#21668=ORIENTED_EDGE('',*,*,#15852,.F.);
#21669=ORIENTED_EDGE('',*,*,#15853,.T.);
#21670=ORIENTED_EDGE('',*,*,#15854,.T.);
#21671=ORIENTED_EDGE('',*,*,#15849,.F.);
#21672=ORIENTED_EDGE('',*,*,#15855,.F.);
#21673=ORIENTED_EDGE('',*,*,#15856,.F.);
#21674=ORIENTED_EDGE('',*,*,#15851,.F.);
#21675=ORIENTED_EDGE('',*,*,#15848,.F.);
#21676=ORIENTED_EDGE('',*,*,#15148,.T.);
#21677=ORIENTED_EDGE('',*,*,#15587,.T.);
#21678=ORIENTED_EDGE('',*,*,#15857,.F.);
#21679=ORIENTED_EDGE('',*,*,#15855,.T.);
#21680=ORIENTED_EDGE('',*,*,#15586,.T.);
#21681=ORIENTED_EDGE('',*,*,#15846,.F.);
#21682=ORIENTED_EDGE('',*,*,#15858,.T.);
#21683=ORIENTED_EDGE('',*,*,#15857,.T.);
#21684=ORIENTED_EDGE('',*,*,#15858,.F.);
#21685=ORIENTED_EDGE('',*,*,#15859,.F.);
#21686=ORIENTED_EDGE('',*,*,#15860,.F.);
#21687=ORIENTED_EDGE('',*,*,#15856,.T.);
#21688=ORIENTED_EDGE('',*,*,#15843,.F.);
#21689=ORIENTED_EDGE('',*,*,#15861,.F.);
#21690=ORIENTED_EDGE('',*,*,#15859,.T.);
#21691=ORIENTED_EDGE('',*,*,#15845,.F.);
#21692=ORIENTED_EDGE('',*,*,#15582,.T.);
#21693=ORIENTED_EDGE('',*,*,#15826,.F.);
#21694=ORIENTED_EDGE('',*,*,#15862,.T.);
#21695=ORIENTED_EDGE('',*,*,#15834,.T.);
#21696=ORIENTED_EDGE('',*,*,#15831,.F.);
#21697=ORIENTED_EDGE('',*,*,#15835,.F.);
#21698=ORIENTED_EDGE('',*,*,#15863,.F.);
#21699=ORIENTED_EDGE('',*,*,#15864,.F.);
#21700=ORIENTED_EDGE('',*,*,#15862,.F.);
#21701=ORIENTED_EDGE('',*,*,#15865,.F.);
#21702=ORIENTED_EDGE('',*,*,#15866,.F.);
#21703=ORIENTED_EDGE('',*,*,#15863,.T.);
#21704=ORIENTED_EDGE('',*,*,#15823,.F.);
#21705=ORIENTED_EDGE('',*,*,#15867,.F.);
#21706=ORIENTED_EDGE('',*,*,#15865,.T.);
#21707=ORIENTED_EDGE('',*,*,#15825,.F.);
#21708=ORIENTED_EDGE('',*,*,#15797,.F.);
#21709=ORIENTED_EDGE('',*,*,#15800,.T.);
#21710=ORIENTED_EDGE('',*,*,#15868,.T.);
#21711=ORIENTED_EDGE('',*,*,#15577,.T.);
#21712=ORIENTED_EDGE('',*,*,#15792,.T.);
#21713=ORIENTED_EDGE('',*,*,#15578,.T.);
#21714=ORIENTED_EDGE('',*,*,#15868,.F.);
#21715=ORIENTED_EDGE('',*,*,#15869,.T.);
#21716=ORIENTED_EDGE('',*,*,#15814,.T.);
#21717=ORIENTED_EDGE('',*,*,#15811,.F.);
#21718=ORIENTED_EDGE('',*,*,#15815,.F.);
#21719=ORIENTED_EDGE('',*,*,#15870,.F.);
#21720=ORIENTED_EDGE('',*,*,#15871,.F.);
#21721=ORIENTED_EDGE('',*,*,#15869,.F.);
#21722=ORIENTED_EDGE('',*,*,#15799,.F.);
#21723=ORIENTED_EDGE('',*,*,#15872,.F.);
#21724=ORIENTED_EDGE('',*,*,#15870,.T.);
#21725=ORIENTED_EDGE('',*,*,#15574,.T.);
#21726=ORIENTED_EDGE('',*,*,#15778,.F.);
#21727=ORIENTED_EDGE('',*,*,#15873,.T.);
#21728=ORIENTED_EDGE('',*,*,#15789,.T.);
#21729=ORIENTED_EDGE('',*,*,#15873,.F.);
#21730=ORIENTED_EDGE('',*,*,#15874,.F.);
#21731=ORIENTED_EDGE('',*,*,#15875,.F.);
#21732=ORIENTED_EDGE('',*,*,#15786,.T.);
#21733=ORIENTED_EDGE('',*,*,#15775,.F.);
#21734=ORIENTED_EDGE('',*,*,#15876,.F.);
#21735=ORIENTED_EDGE('',*,*,#15874,.T.);
#21736=ORIENTED_EDGE('',*,*,#15777,.F.);
#21737=ORIENTED_EDGE('',*,*,#15570,.T.);
#21738=ORIENTED_EDGE('',*,*,#15758,.F.);
#21739=ORIENTED_EDGE('',*,*,#15877,.T.);
#21740=ORIENTED_EDGE('',*,*,#15766,.T.);
#21741=ORIENTED_EDGE('',*,*,#15763,.F.);
#21742=ORIENTED_EDGE('',*,*,#15767,.F.);
#21743=ORIENTED_EDGE('',*,*,#15878,.F.);
#21744=ORIENTED_EDGE('',*,*,#15879,.F.);
#21745=ORIENTED_EDGE('',*,*,#15877,.F.);
#21746=ORIENTED_EDGE('',*,*,#15880,.F.);
#21747=ORIENTED_EDGE('',*,*,#15881,.F.);
#21748=ORIENTED_EDGE('',*,*,#15878,.T.);
#21749=ORIENTED_EDGE('',*,*,#15755,.F.);
#21750=ORIENTED_EDGE('',*,*,#15882,.F.);
#21751=ORIENTED_EDGE('',*,*,#15880,.T.);
#21752=ORIENTED_EDGE('',*,*,#15757,.F.);
#21753=ORIENTED_EDGE('',*,*,#15566,.T.);
#21754=ORIENTED_EDGE('',*,*,#15738,.F.);
#21755=ORIENTED_EDGE('',*,*,#15883,.T.);
#21756=ORIENTED_EDGE('',*,*,#15746,.T.);
#21757=ORIENTED_EDGE('',*,*,#15743,.F.);
#21758=ORIENTED_EDGE('',*,*,#15747,.F.);
#21759=ORIENTED_EDGE('',*,*,#15884,.F.);
#21760=ORIENTED_EDGE('',*,*,#15885,.F.);
#21761=ORIENTED_EDGE('',*,*,#15883,.F.);
#21762=ORIENTED_EDGE('',*,*,#15886,.F.);
#21763=ORIENTED_EDGE('',*,*,#15887,.F.);
#21764=ORIENTED_EDGE('',*,*,#15884,.T.);
#21765=ORIENTED_EDGE('',*,*,#15735,.F.);
#21766=ORIENTED_EDGE('',*,*,#15888,.F.);
#21767=ORIENTED_EDGE('',*,*,#15886,.T.);
#21768=ORIENTED_EDGE('',*,*,#15737,.F.);
#21769=ORIENTED_EDGE('',*,*,#15562,.T.);
#21770=ORIENTED_EDGE('',*,*,#15045,.T.);
#21771=ORIENTED_EDGE('',*,*,#15889,.T.);
#21772=ORIENTED_EDGE('',*,*,#15726,.T.);
#21773=ORIENTED_EDGE('',*,*,#15723,.F.);
#21774=ORIENTED_EDGE('',*,*,#15727,.F.);
#21775=ORIENTED_EDGE('',*,*,#15890,.F.);
#21776=ORIENTED_EDGE('',*,*,#15891,.F.);
#21777=ORIENTED_EDGE('',*,*,#15889,.F.);
#21778=ORIENTED_EDGE('',*,*,#15049,.F.);
#21779=ORIENTED_EDGE('',*,*,#15892,.F.);
#21780=ORIENTED_EDGE('',*,*,#15890,.T.);
#21781=ORIENTED_EDGE('',*,*,#15561,.T.);
#21782=ORIENTED_EDGE('',*,*,#15121,.F.);
#21783=ORIENTED_EDGE('',*,*,#15893,.T.);
#21784=ORIENTED_EDGE('',*,*,#15134,.T.);
#21785=ORIENTED_EDGE('',*,*,#15893,.F.);
#21786=ORIENTED_EDGE('',*,*,#15894,.F.);
#21787=ORIENTED_EDGE('',*,*,#15895,.F.);
#21788=ORIENTED_EDGE('',*,*,#15130,.T.);
#21789=ORIENTED_EDGE('',*,*,#15118,.F.);
#21790=ORIENTED_EDGE('',*,*,#15896,.F.);
#21791=ORIENTED_EDGE('',*,*,#15894,.T.);
#21792=ORIENTED_EDGE('',*,*,#15120,.F.);
#21793=ORIENTED_EDGE('',*,*,#15560,.T.);
#21794=ORIENTED_EDGE('',*,*,#15098,.F.);
#21795=ORIENTED_EDGE('',*,*,#15897,.T.);
#21796=ORIENTED_EDGE('',*,*,#15108,.T.);
#21797=ORIENTED_EDGE('',*,*,#15104,.F.);
#21798=ORIENTED_EDGE('',*,*,#15109,.F.);
#21799=ORIENTED_EDGE('',*,*,#15898,.F.);
#21800=ORIENTED_EDGE('',*,*,#15899,.F.);
#21801=ORIENTED_EDGE('',*,*,#15897,.F.);
#21802=ORIENTED_EDGE('',*,*,#15900,.F.);
#21803=ORIENTED_EDGE('',*,*,#15901,.F.);
#21804=ORIENTED_EDGE('',*,*,#15898,.T.);
#21805=ORIENTED_EDGE('',*,*,#15088,.F.);
#21806=ORIENTED_EDGE('',*,*,#15902,.F.);
#21807=ORIENTED_EDGE('',*,*,#15900,.T.);
#21808=ORIENTED_EDGE('',*,*,#15097,.F.);
#21809=ORIENTED_EDGE('',*,*,#15903,.T.);
#21810=ORIENTED_EDGE('',*,*,#15904,.T.);
#21811=ORIENTED_EDGE('',*,*,#15905,.T.);
#21812=ORIENTED_EDGE('',*,*,#15906,.T.);
#21813=ORIENTED_EDGE('',*,*,#15907,.T.);
#21814=ORIENTED_EDGE('',*,*,#15908,.T.);
#21815=ORIENTED_EDGE('',*,*,#15906,.F.);
#21816=ORIENTED_EDGE('',*,*,#15909,.T.);
#21817=ORIENTED_EDGE('',*,*,#15535,.T.);
#21818=ORIENTED_EDGE('',*,*,#15910,.F.);
#21819=ORIENTED_EDGE('',*,*,#15911,.T.);
#21820=ORIENTED_EDGE('',*,*,#15905,.F.);
#21821=ORIENTED_EDGE('',*,*,#15912,.T.);
#21822=ORIENTED_EDGE('',*,*,#15913,.F.);
#21823=ORIENTED_EDGE('',*,*,#15914,.F.);
#21824=ORIENTED_EDGE('',*,*,#15536,.T.);
#21825=ORIENTED_EDGE('',*,*,#15909,.F.);
#21826=ORIENTED_EDGE('',*,*,#15904,.F.);
#21827=ORIENTED_EDGE('',*,*,#15915,.F.);
#21828=ORIENTED_EDGE('',*,*,#15916,.F.);
#21829=ORIENTED_EDGE('',*,*,#15912,.F.);
#21830=ORIENTED_EDGE('',*,*,#15913,.T.);
#21831=ORIENTED_EDGE('',*,*,#15916,.T.);
#21832=ORIENTED_EDGE('',*,*,#15917,.T.);
#21833=ORIENTED_EDGE('',*,*,#15918,.T.);
#21834=ORIENTED_EDGE('',*,*,#15919,.T.);
#21835=ORIENTED_EDGE('',*,*,#15920,.T.);
#21836=ORIENTED_EDGE('',*,*,#15920,.F.);
#21837=ORIENTED_EDGE('',*,*,#15921,.T.);
#21838=ORIENTED_EDGE('',*,*,#15922,.T.);
#21839=ORIENTED_EDGE('',*,*,#15537,.T.);
#21840=ORIENTED_EDGE('',*,*,#15914,.T.);
#21841=ORIENTED_EDGE('',*,*,#15923,.T.);
#21842=ORIENTED_EDGE('',*,*,#15924,.T.);
#21843=ORIENTED_EDGE('',*,*,#15925,.T.);
#21844=ORIENTED_EDGE('',*,*,#15926,.T.);
#21845=ORIENTED_EDGE('',*,*,#15927,.T.);
#21846=ORIENTED_EDGE('',*,*,#15928,.T.);
#21847=ORIENTED_EDGE('',*,*,#15926,.F.);
#21848=ORIENTED_EDGE('',*,*,#15929,.T.);
#21849=ORIENTED_EDGE('',*,*,#15539,.T.);
#21850=ORIENTED_EDGE('',*,*,#15930,.F.);
#21851=ORIENTED_EDGE('',*,*,#15931,.T.);
#21852=ORIENTED_EDGE('',*,*,#15925,.F.);
#21853=ORIENTED_EDGE('',*,*,#15932,.T.);
#21854=ORIENTED_EDGE('',*,*,#15933,.F.);
#21855=ORIENTED_EDGE('',*,*,#15934,.F.);
#21856=ORIENTED_EDGE('',*,*,#15540,.T.);
#21857=ORIENTED_EDGE('',*,*,#15929,.F.);
#21858=ORIENTED_EDGE('',*,*,#15924,.F.);
#21859=ORIENTED_EDGE('',*,*,#15935,.F.);
#21860=ORIENTED_EDGE('',*,*,#15936,.F.);
#21861=ORIENTED_EDGE('',*,*,#15932,.F.);
#21862=ORIENTED_EDGE('',*,*,#15933,.T.);
#21863=ORIENTED_EDGE('',*,*,#15936,.T.);
#21864=ORIENTED_EDGE('',*,*,#15937,.T.);
#21865=ORIENTED_EDGE('',*,*,#15938,.T.);
#21866=ORIENTED_EDGE('',*,*,#15939,.T.);
#21867=ORIENTED_EDGE('',*,*,#15940,.T.);
#21868=ORIENTED_EDGE('',*,*,#15940,.F.);
#21869=ORIENTED_EDGE('',*,*,#15941,.T.);
#21870=ORIENTED_EDGE('',*,*,#15942,.T.);
#21871=ORIENTED_EDGE('',*,*,#15541,.T.);
#21872=ORIENTED_EDGE('',*,*,#15934,.T.);
#21873=ORIENTED_EDGE('',*,*,#15943,.T.);
#21874=ORIENTED_EDGE('',*,*,#15944,.T.);
#21875=ORIENTED_EDGE('',*,*,#15945,.T.);
#21876=ORIENTED_EDGE('',*,*,#15946,.T.);
#21877=ORIENTED_EDGE('',*,*,#15947,.T.);
#21878=ORIENTED_EDGE('',*,*,#15948,.T.);
#21879=ORIENTED_EDGE('',*,*,#15946,.F.);
#21880=ORIENTED_EDGE('',*,*,#15949,.T.);
#21881=ORIENTED_EDGE('',*,*,#15543,.T.);
#21882=ORIENTED_EDGE('',*,*,#15950,.F.);
#21883=ORIENTED_EDGE('',*,*,#15951,.T.);
#21884=ORIENTED_EDGE('',*,*,#15945,.F.);
#21885=ORIENTED_EDGE('',*,*,#15952,.T.);
#21886=ORIENTED_EDGE('',*,*,#15953,.F.);
#21887=ORIENTED_EDGE('',*,*,#15954,.F.);
#21888=ORIENTED_EDGE('',*,*,#15544,.T.);
#21889=ORIENTED_EDGE('',*,*,#15949,.F.);
#21890=ORIENTED_EDGE('',*,*,#15944,.F.);
#21891=ORIENTED_EDGE('',*,*,#15955,.F.);
#21892=ORIENTED_EDGE('',*,*,#15956,.F.);
#21893=ORIENTED_EDGE('',*,*,#15952,.F.);
#21894=ORIENTED_EDGE('',*,*,#15953,.T.);
#21895=ORIENTED_EDGE('',*,*,#15956,.T.);
#21896=ORIENTED_EDGE('',*,*,#15957,.T.);
#21897=ORIENTED_EDGE('',*,*,#15958,.T.);
#21898=ORIENTED_EDGE('',*,*,#15959,.T.);
#21899=ORIENTED_EDGE('',*,*,#15960,.T.);
#21900=ORIENTED_EDGE('',*,*,#15960,.F.);
#21901=ORIENTED_EDGE('',*,*,#15961,.T.);
#21902=ORIENTED_EDGE('',*,*,#15962,.T.);
#21903=ORIENTED_EDGE('',*,*,#15545,.T.);
#21904=ORIENTED_EDGE('',*,*,#15954,.T.);
#21905=ORIENTED_EDGE('',*,*,#15963,.T.);
#21906=ORIENTED_EDGE('',*,*,#15964,.T.);
#21907=ORIENTED_EDGE('',*,*,#15965,.T.);
#21908=ORIENTED_EDGE('',*,*,#15966,.T.);
#21909=ORIENTED_EDGE('',*,*,#15967,.T.);
#21910=ORIENTED_EDGE('',*,*,#15968,.T.);
#21911=ORIENTED_EDGE('',*,*,#15966,.F.);
#21912=ORIENTED_EDGE('',*,*,#15969,.T.);
#21913=ORIENTED_EDGE('',*,*,#15547,.T.);
#21914=ORIENTED_EDGE('',*,*,#15970,.F.);
#21915=ORIENTED_EDGE('',*,*,#15971,.T.);
#21916=ORIENTED_EDGE('',*,*,#15965,.F.);
#21917=ORIENTED_EDGE('',*,*,#15972,.T.);
#21918=ORIENTED_EDGE('',*,*,#15973,.F.);
#21919=ORIENTED_EDGE('',*,*,#15974,.F.);
#21920=ORIENTED_EDGE('',*,*,#15548,.T.);
#21921=ORIENTED_EDGE('',*,*,#15969,.F.);
#21922=ORIENTED_EDGE('',*,*,#15964,.F.);
#21923=ORIENTED_EDGE('',*,*,#15975,.F.);
#21924=ORIENTED_EDGE('',*,*,#15976,.F.);
#21925=ORIENTED_EDGE('',*,*,#15972,.F.);
#21926=ORIENTED_EDGE('',*,*,#15973,.T.);
#21927=ORIENTED_EDGE('',*,*,#15976,.T.);
#21928=ORIENTED_EDGE('',*,*,#15977,.T.);
#21929=ORIENTED_EDGE('',*,*,#15978,.T.);
#21930=ORIENTED_EDGE('',*,*,#15979,.T.);
#21931=ORIENTED_EDGE('',*,*,#15980,.T.);
#21932=ORIENTED_EDGE('',*,*,#15980,.F.);
#21933=ORIENTED_EDGE('',*,*,#15981,.T.);
#21934=ORIENTED_EDGE('',*,*,#15982,.T.);
#21935=ORIENTED_EDGE('',*,*,#15549,.T.);
#21936=ORIENTED_EDGE('',*,*,#15974,.T.);
#21937=ORIENTED_EDGE('',*,*,#15983,.T.);
#21938=ORIENTED_EDGE('',*,*,#15984,.T.);
#21939=ORIENTED_EDGE('',*,*,#15985,.T.);
#21940=ORIENTED_EDGE('',*,*,#15986,.T.);
#21941=ORIENTED_EDGE('',*,*,#15987,.T.);
#21942=ORIENTED_EDGE('',*,*,#15988,.T.);
#21943=ORIENTED_EDGE('',*,*,#15986,.F.);
#21944=ORIENTED_EDGE('',*,*,#15989,.T.);
#21945=ORIENTED_EDGE('',*,*,#15551,.T.);
#21946=ORIENTED_EDGE('',*,*,#15990,.F.);
#21947=ORIENTED_EDGE('',*,*,#15991,.T.);
#21948=ORIENTED_EDGE('',*,*,#15985,.F.);
#21949=ORIENTED_EDGE('',*,*,#15992,.T.);
#21950=ORIENTED_EDGE('',*,*,#15993,.F.);
#21951=ORIENTED_EDGE('',*,*,#15994,.F.);
#21952=ORIENTED_EDGE('',*,*,#15552,.T.);
#21953=ORIENTED_EDGE('',*,*,#15989,.F.);
#21954=ORIENTED_EDGE('',*,*,#15984,.F.);
#21955=ORIENTED_EDGE('',*,*,#15995,.F.);
#21956=ORIENTED_EDGE('',*,*,#15996,.F.);
#21957=ORIENTED_EDGE('',*,*,#15992,.F.);
#21958=ORIENTED_EDGE('',*,*,#15993,.T.);
#21959=ORIENTED_EDGE('',*,*,#15996,.T.);
#21960=ORIENTED_EDGE('',*,*,#15997,.T.);
#21961=ORIENTED_EDGE('',*,*,#15998,.T.);
#21962=ORIENTED_EDGE('',*,*,#15999,.T.);
#21963=ORIENTED_EDGE('',*,*,#16000,.T.);
#21964=ORIENTED_EDGE('',*,*,#16000,.F.);
#21965=ORIENTED_EDGE('',*,*,#16001,.T.);
#21966=ORIENTED_EDGE('',*,*,#16002,.T.);
#21967=ORIENTED_EDGE('',*,*,#15553,.T.);
#21968=ORIENTED_EDGE('',*,*,#15994,.T.);
#21969=ORIENTED_EDGE('',*,*,#16003,.T.);
#21970=ORIENTED_EDGE('',*,*,#16004,.T.);
#21971=ORIENTED_EDGE('',*,*,#16005,.T.);
#21972=ORIENTED_EDGE('',*,*,#16006,.T.);
#21973=ORIENTED_EDGE('',*,*,#16007,.T.);
#21974=ORIENTED_EDGE('',*,*,#16008,.T.);
#21975=ORIENTED_EDGE('',*,*,#16006,.F.);
#21976=ORIENTED_EDGE('',*,*,#16009,.T.);
#21977=ORIENTED_EDGE('',*,*,#15555,.T.);
#21978=ORIENTED_EDGE('',*,*,#16010,.F.);
#21979=ORIENTED_EDGE('',*,*,#16011,.T.);
#21980=ORIENTED_EDGE('',*,*,#16005,.F.);
#21981=ORIENTED_EDGE('',*,*,#16012,.T.);
#21982=ORIENTED_EDGE('',*,*,#16013,.F.);
#21983=ORIENTED_EDGE('',*,*,#16014,.F.);
#21984=ORIENTED_EDGE('',*,*,#15556,.T.);
#21985=ORIENTED_EDGE('',*,*,#16009,.F.);
#21986=ORIENTED_EDGE('',*,*,#16004,.F.);
#21987=ORIENTED_EDGE('',*,*,#16015,.F.);
#21988=ORIENTED_EDGE('',*,*,#16016,.F.);
#21989=ORIENTED_EDGE('',*,*,#16012,.F.);
#21990=ORIENTED_EDGE('',*,*,#16013,.T.);
#21991=ORIENTED_EDGE('',*,*,#16016,.T.);
#21992=ORIENTED_EDGE('',*,*,#16017,.T.);
#21993=ORIENTED_EDGE('',*,*,#16018,.T.);
#21994=ORIENTED_EDGE('',*,*,#16019,.T.);
#21995=ORIENTED_EDGE('',*,*,#16020,.T.);
#21996=ORIENTED_EDGE('',*,*,#16020,.F.);
#21997=ORIENTED_EDGE('',*,*,#16021,.T.);
#21998=ORIENTED_EDGE('',*,*,#16022,.T.);
#21999=ORIENTED_EDGE('',*,*,#15557,.T.);
#22000=ORIENTED_EDGE('',*,*,#16014,.T.);
#22001=ORIENTED_EDGE('',*,*,#16023,.T.);
#22002=ORIENTED_EDGE('',*,*,#15091,.T.);
#22003=ORIENTED_EDGE('',*,*,#15096,.T.);
#22004=ORIENTED_EDGE('',*,*,#16024,.T.);
#22005=ORIENTED_EDGE('',*,*,#16025,.T.);
#22006=ORIENTED_EDGE('',*,*,#16026,.T.);
#22007=ORIENTED_EDGE('',*,*,#16026,.F.);
#22008=ORIENTED_EDGE('',*,*,#16027,.T.);
#22009=ORIENTED_EDGE('',*,*,#16028,.F.);
#22010=ORIENTED_EDGE('',*,*,#16029,.T.);
#22011=ORIENTED_EDGE('',*,*,#16030,.T.);
#22012=ORIENTED_EDGE('',*,*,#16025,.F.);
#22013=ORIENTED_EDGE('',*,*,#16031,.F.);
#22014=ORIENTED_EDGE('',*,*,#16032,.F.);
#22015=ORIENTED_EDGE('',*,*,#16027,.F.);
#22016=ORIENTED_EDGE('',*,*,#16024,.F.);
#22017=ORIENTED_EDGE('',*,*,#15095,.T.);
#22018=ORIENTED_EDGE('',*,*,#15559,.T.);
#22019=ORIENTED_EDGE('',*,*,#16033,.F.);
#22020=ORIENTED_EDGE('',*,*,#16031,.T.);
#22021=ORIENTED_EDGE('',*,*,#15558,.T.);
#22022=ORIENTED_EDGE('',*,*,#16022,.F.);
#22023=ORIENTED_EDGE('',*,*,#16034,.T.);
#22024=ORIENTED_EDGE('',*,*,#16033,.T.);
#22025=ORIENTED_EDGE('',*,*,#16034,.F.);
#22026=ORIENTED_EDGE('',*,*,#16035,.F.);
#22027=ORIENTED_EDGE('',*,*,#16036,.F.);
#22028=ORIENTED_EDGE('',*,*,#16032,.T.);
#22029=ORIENTED_EDGE('',*,*,#16019,.F.);
#22030=ORIENTED_EDGE('',*,*,#16037,.F.);
#22031=ORIENTED_EDGE('',*,*,#16035,.T.);
#22032=ORIENTED_EDGE('',*,*,#16021,.F.);
#22033=ORIENTED_EDGE('',*,*,#15554,.T.);
#22034=ORIENTED_EDGE('',*,*,#16002,.F.);
#22035=ORIENTED_EDGE('',*,*,#16038,.T.);
#22036=ORIENTED_EDGE('',*,*,#16010,.T.);
#22037=ORIENTED_EDGE('',*,*,#16007,.F.);
#22038=ORIENTED_EDGE('',*,*,#16011,.F.);
#22039=ORIENTED_EDGE('',*,*,#16039,.F.);
#22040=ORIENTED_EDGE('',*,*,#16040,.F.);
#22041=ORIENTED_EDGE('',*,*,#16038,.F.);
#22042=ORIENTED_EDGE('',*,*,#16041,.F.);
#22043=ORIENTED_EDGE('',*,*,#16042,.F.);
#22044=ORIENTED_EDGE('',*,*,#16039,.T.);
#22045=ORIENTED_EDGE('',*,*,#15999,.F.);
#22046=ORIENTED_EDGE('',*,*,#16043,.F.);
#22047=ORIENTED_EDGE('',*,*,#16041,.T.);
#22048=ORIENTED_EDGE('',*,*,#16001,.F.);
#22049=ORIENTED_EDGE('',*,*,#15550,.T.);
#22050=ORIENTED_EDGE('',*,*,#15982,.F.);
#22051=ORIENTED_EDGE('',*,*,#16044,.T.);
#22052=ORIENTED_EDGE('',*,*,#15990,.T.);
#22053=ORIENTED_EDGE('',*,*,#15987,.F.);
#22054=ORIENTED_EDGE('',*,*,#15991,.F.);
#22055=ORIENTED_EDGE('',*,*,#16045,.F.);
#22056=ORIENTED_EDGE('',*,*,#16046,.F.);
#22057=ORIENTED_EDGE('',*,*,#16044,.F.);
#22058=ORIENTED_EDGE('',*,*,#16047,.F.);
#22059=ORIENTED_EDGE('',*,*,#16048,.F.);
#22060=ORIENTED_EDGE('',*,*,#16045,.T.);
#22061=ORIENTED_EDGE('',*,*,#15979,.F.);
#22062=ORIENTED_EDGE('',*,*,#16049,.F.);
#22063=ORIENTED_EDGE('',*,*,#16047,.T.);
#22064=ORIENTED_EDGE('',*,*,#15981,.F.);
#22065=ORIENTED_EDGE('',*,*,#15546,.T.);
#22066=ORIENTED_EDGE('',*,*,#15962,.F.);
#22067=ORIENTED_EDGE('',*,*,#16050,.T.);
#22068=ORIENTED_EDGE('',*,*,#15970,.T.);
#22069=ORIENTED_EDGE('',*,*,#15967,.F.);
#22070=ORIENTED_EDGE('',*,*,#15971,.F.);
#22071=ORIENTED_EDGE('',*,*,#16051,.F.);
#22072=ORIENTED_EDGE('',*,*,#16052,.F.);
#22073=ORIENTED_EDGE('',*,*,#16050,.F.);
#22074=ORIENTED_EDGE('',*,*,#16053,.F.);
#22075=ORIENTED_EDGE('',*,*,#16054,.F.);
#22076=ORIENTED_EDGE('',*,*,#16051,.T.);
#22077=ORIENTED_EDGE('',*,*,#15959,.F.);
#22078=ORIENTED_EDGE('',*,*,#16055,.F.);
#22079=ORIENTED_EDGE('',*,*,#16053,.T.);
#22080=ORIENTED_EDGE('',*,*,#15961,.F.);
#22081=ORIENTED_EDGE('',*,*,#15542,.T.);
#22082=ORIENTED_EDGE('',*,*,#15942,.F.);
#22083=ORIENTED_EDGE('',*,*,#16056,.T.);
#22084=ORIENTED_EDGE('',*,*,#15950,.T.);
#22085=ORIENTED_EDGE('',*,*,#15947,.F.);
#22086=ORIENTED_EDGE('',*,*,#15951,.F.);
#22087=ORIENTED_EDGE('',*,*,#16057,.F.);
#22088=ORIENTED_EDGE('',*,*,#16058,.F.);
#22089=ORIENTED_EDGE('',*,*,#16056,.F.);
#22090=ORIENTED_EDGE('',*,*,#16059,.F.);
#22091=ORIENTED_EDGE('',*,*,#16060,.F.);
#22092=ORIENTED_EDGE('',*,*,#16057,.T.);
#22093=ORIENTED_EDGE('',*,*,#15939,.F.);
#22094=ORIENTED_EDGE('',*,*,#16061,.F.);
#22095=ORIENTED_EDGE('',*,*,#16059,.T.);
#22096=ORIENTED_EDGE('',*,*,#15941,.F.);
#22097=ORIENTED_EDGE('',*,*,#15538,.T.);
#22098=ORIENTED_EDGE('',*,*,#15922,.F.);
#22099=ORIENTED_EDGE('',*,*,#16062,.T.);
#22100=ORIENTED_EDGE('',*,*,#15930,.T.);
#22101=ORIENTED_EDGE('',*,*,#15927,.F.);
#22102=ORIENTED_EDGE('',*,*,#15931,.F.);
#22103=ORIENTED_EDGE('',*,*,#16063,.F.);
#22104=ORIENTED_EDGE('',*,*,#16064,.F.);
#22105=ORIENTED_EDGE('',*,*,#16062,.F.);
#22106=ORIENTED_EDGE('',*,*,#16065,.F.);
#22107=ORIENTED_EDGE('',*,*,#16066,.F.);
#22108=ORIENTED_EDGE('',*,*,#16063,.T.);
#22109=ORIENTED_EDGE('',*,*,#15919,.F.);
#22110=ORIENTED_EDGE('',*,*,#16067,.F.);
#22111=ORIENTED_EDGE('',*,*,#16065,.T.);
#22112=ORIENTED_EDGE('',*,*,#15921,.F.);
#22113=ORIENTED_EDGE('',*,*,#15534,.T.);
#22114=ORIENTED_EDGE('',*,*,#16068,.T.);
#22115=ORIENTED_EDGE('',*,*,#16069,.T.);
#22116=ORIENTED_EDGE('',*,*,#15910,.T.);
#22117=ORIENTED_EDGE('',*,*,#15907,.F.);
#22118=ORIENTED_EDGE('',*,*,#15911,.F.);
#22119=ORIENTED_EDGE('',*,*,#16070,.F.);
#22120=ORIENTED_EDGE('',*,*,#16071,.F.);
#22121=ORIENTED_EDGE('',*,*,#16069,.F.);
#22122=ORIENTED_EDGE('',*,*,#15060,.F.);
#22123=ORIENTED_EDGE('',*,*,#16072,.F.);
#22124=ORIENTED_EDGE('',*,*,#16070,.T.);
#22125=ORIENTED_EDGE('',*,*,#15058,.F.);
#22126=ORIENTED_EDGE('',*,*,#15061,.T.);
#22127=ORIENTED_EDGE('',*,*,#16068,.F.);
#22128=ORIENTED_EDGE('',*,*,#15533,.T.);
#22129=ORIENTED_EDGE('',*,*,#16073,.T.);
#22130=ORIENTED_EDGE('',*,*,#15426,.F.);
#22131=ORIENTED_EDGE('',*,*,#16074,.T.);
#22132=ORIENTED_EDGE('',*,*,#16075,.T.);
#22133=ORIENTED_EDGE('',*,*,#16076,.T.);
#22134=ORIENTED_EDGE('',*,*,#15628,.T.);
#22135=ORIENTED_EDGE('',*,*,#16077,.T.);
#22136=ORIENTED_EDGE('',*,*,#16078,.T.);
#22137=ORIENTED_EDGE('',*,*,#15627,.T.);
#22138=ORIENTED_EDGE('',*,*,#16076,.F.);
#22139=ORIENTED_EDGE('',*,*,#15437,.F.);
#22140=ORIENTED_EDGE('',*,*,#15625,.T.);
#22141=ORIENTED_EDGE('',*,*,#16078,.F.);
#22142=ORIENTED_EDGE('',*,*,#16079,.T.);
#22143=ORIENTED_EDGE('',*,*,#16080,.T.);
#22144=ORIENTED_EDGE('',*,*,#16079,.F.);
#22145=ORIENTED_EDGE('',*,*,#16077,.F.);
#22146=ORIENTED_EDGE('',*,*,#16075,.F.);
#22147=ORIENTED_EDGE('',*,*,#16081,.F.);
#22148=ORIENTED_EDGE('',*,*,#16082,.F.);
#22149=ORIENTED_EDGE('',*,*,#16083,.F.);
#22150=ORIENTED_EDGE('',*,*,#16084,.F.);
#22151=ORIENTED_EDGE('',*,*,#16085,.F.);
#22152=ORIENTED_EDGE('',*,*,#16086,.F.);
#22153=ORIENTED_EDGE('',*,*,#16087,.F.);
#22154=ORIENTED_EDGE('',*,*,#16088,.F.);
#22155=ORIENTED_EDGE('',*,*,#16089,.F.);
#22156=ORIENTED_EDGE('',*,*,#15649,.F.);
#22157=ORIENTED_EDGE('',*,*,#15652,.F.);
#22158=ORIENTED_EDGE('',*,*,#16090,.F.);
#22159=ORIENTED_EDGE('',*,*,#16091,.F.);
#22160=ORIENTED_EDGE('',*,*,#15297,.F.);
#22161=ORIENTED_EDGE('',*,*,#16092,.F.);
#22162=ORIENTED_EDGE('',*,*,#16093,.F.);
#22163=ORIENTED_EDGE('',*,*,#16094,.F.);
#22164=ORIENTED_EDGE('',*,*,#16095,.F.);
#22165=ORIENTED_EDGE('',*,*,#16096,.F.);
#22166=ORIENTED_EDGE('',*,*,#16097,.F.);
#22167=ORIENTED_EDGE('',*,*,#16098,.F.);
#22168=ORIENTED_EDGE('',*,*,#16099,.F.);
#22169=ORIENTED_EDGE('',*,*,#16100,.F.);
#22170=ORIENTED_EDGE('',*,*,#15238,.F.);
#22171=ORIENTED_EDGE('',*,*,#15241,.F.);
#22172=ORIENTED_EDGE('',*,*,#16101,.F.);
#22173=ORIENTED_EDGE('',*,*,#16102,.F.);
#22174=ORIENTED_EDGE('',*,*,#16103,.F.);
#22175=ORIENTED_EDGE('',*,*,#16104,.F.);
#22176=ORIENTED_EDGE('',*,*,#16105,.F.);
#22177=ORIENTED_EDGE('',*,*,#16106,.F.);
#22178=ORIENTED_EDGE('',*,*,#15036,.F.);
#22179=ORIENTED_EDGE('',*,*,#16107,.F.);
#22180=ORIENTED_EDGE('',*,*,#16108,.F.);
#22181=ORIENTED_EDGE('',*,*,#16109,.F.);
#22182=ORIENTED_EDGE('',*,*,#16110,.F.);
#22183=ORIENTED_EDGE('',*,*,#16111,.F.);
#22184=ORIENTED_EDGE('',*,*,#16112,.F.);
#22185=ORIENTED_EDGE('',*,*,#16113,.F.);
#22186=ORIENTED_EDGE('',*,*,#16114,.F.);
#22187=ORIENTED_EDGE('',*,*,#16115,.F.);
#22188=ORIENTED_EDGE('',*,*,#15853,.F.);
#22189=ORIENTED_EDGE('',*,*,#16116,.F.);
#22190=ORIENTED_EDGE('',*,*,#16117,.F.);
#22191=ORIENTED_EDGE('',*,*,#16118,.F.);
#22192=ORIENTED_EDGE('',*,*,#16119,.F.);
#22193=ORIENTED_EDGE('',*,*,#16120,.F.);
#22194=ORIENTED_EDGE('',*,*,#16121,.F.);
#22195=ORIENTED_EDGE('',*,*,#16122,.F.);
#22196=ORIENTED_EDGE('',*,*,#16123,.F.);
#22197=ORIENTED_EDGE('',*,*,#16124,.F.);
#22198=ORIENTED_EDGE('',*,*,#15802,.F.);
#22199=ORIENTED_EDGE('',*,*,#15805,.F.);
#22200=ORIENTED_EDGE('',*,*,#16125,.F.);
#22201=ORIENTED_EDGE('',*,*,#16126,.F.);
#22202=ORIENTED_EDGE('',*,*,#16127,.F.);
#22203=ORIENTED_EDGE('',*,*,#16128,.F.);
#22204=ORIENTED_EDGE('',*,*,#16129,.F.);
#22205=ORIENTED_EDGE('',*,*,#16130,.F.);
#22206=ORIENTED_EDGE('',*,*,#16131,.F.);
#22207=ORIENTED_EDGE('',*,*,#16132,.F.);
#22208=ORIENTED_EDGE('',*,*,#16133,.F.);
#22209=ORIENTED_EDGE('',*,*,#16134,.F.);
#22210=ORIENTED_EDGE('',*,*,#16135,.F.);
#22211=ORIENTED_EDGE('',*,*,#16136,.F.);
#22212=ORIENTED_EDGE('',*,*,#16137,.F.);
#22213=ORIENTED_EDGE('',*,*,#16138,.F.);
#22214=ORIENTED_EDGE('',*,*,#15051,.F.);
#22215=ORIENTED_EDGE('',*,*,#16139,.F.);
#22216=ORIENTED_EDGE('',*,*,#16140,.F.);
#22217=ORIENTED_EDGE('',*,*,#16141,.F.);
#22218=ORIENTED_EDGE('',*,*,#16142,.F.);
#22219=ORIENTED_EDGE('',*,*,#16143,.F.);
#22220=ORIENTED_EDGE('',*,*,#16144,.F.);
#22221=ORIENTED_EDGE('',*,*,#16145,.F.);
#22222=ORIENTED_EDGE('',*,*,#16146,.F.);
#22223=ORIENTED_EDGE('',*,*,#16147,.F.);
#22224=ORIENTED_EDGE('',*,*,#16029,.F.);
#22225=ORIENTED_EDGE('',*,*,#16148,.F.);
#22226=ORIENTED_EDGE('',*,*,#16149,.F.);
#22227=ORIENTED_EDGE('',*,*,#16150,.F.);
#22228=ORIENTED_EDGE('',*,*,#16151,.F.);
#22229=ORIENTED_EDGE('',*,*,#16152,.F.);
#22230=ORIENTED_EDGE('',*,*,#16153,.F.);
#22231=ORIENTED_EDGE('',*,*,#16154,.F.);
#22232=ORIENTED_EDGE('',*,*,#16155,.F.);
#22233=ORIENTED_EDGE('',*,*,#16156,.F.);
#22234=ORIENTED_EDGE('',*,*,#16157,.F.);
#22235=ORIENTED_EDGE('',*,*,#16158,.F.);
#22236=ORIENTED_EDGE('',*,*,#16159,.F.);
#22237=ORIENTED_EDGE('',*,*,#16160,.F.);
#22238=ORIENTED_EDGE('',*,*,#16161,.F.);
#22239=ORIENTED_EDGE('',*,*,#16162,.F.);
#22240=ORIENTED_EDGE('',*,*,#16163,.F.);
#22241=ORIENTED_EDGE('',*,*,#16164,.F.);
#22242=ORIENTED_EDGE('',*,*,#16165,.F.);
#22243=ORIENTED_EDGE('',*,*,#16166,.F.);
#22244=ORIENTED_EDGE('',*,*,#16167,.F.);
#22245=ORIENTED_EDGE('',*,*,#16168,.F.);
#22246=ORIENTED_EDGE('',*,*,#16169,.F.);
#22247=ORIENTED_EDGE('',*,*,#16170,.F.);
#22248=ORIENTED_EDGE('',*,*,#16171,.F.);
#22249=ORIENTED_EDGE('',*,*,#16172,.F.);
#22250=ORIENTED_EDGE('',*,*,#15063,.F.);
#22251=ORIENTED_EDGE('',*,*,#15068,.F.);
#22252=ORIENTED_EDGE('',*,*,#15357,.F.);
#22253=ORIENTED_EDGE('',*,*,#16173,.F.);
#22254=ORIENTED_EDGE('',*,*,#16174,.F.);
#22255=ORIENTED_EDGE('',*,*,#16175,.F.);
#22256=ORIENTED_EDGE('',*,*,#16176,.F.);
#22257=ORIENTED_EDGE('',*,*,#16177,.F.);
#22258=ORIENTED_EDGE('',*,*,#16178,.F.);
#22259=ORIENTED_EDGE('',*,*,#16179,.F.);
#22260=ORIENTED_EDGE('',*,*,#16180,.F.);
#22261=ORIENTED_EDGE('',*,*,#16181,.F.);
#22262=ORIENTED_EDGE('',*,*,#15082,.F.);
#22263=ORIENTED_EDGE('',*,*,#16182,.F.);
#22264=ORIENTED_EDGE('',*,*,#16183,.F.);
#22265=ORIENTED_EDGE('',*,*,#16184,.F.);
#22266=ORIENTED_EDGE('',*,*,#16185,.F.);
#22267=ORIENTED_EDGE('',*,*,#16186,.F.);
#22268=ORIENTED_EDGE('',*,*,#16187,.F.);
#22269=ORIENTED_EDGE('',*,*,#16188,.F.);
#22270=ORIENTED_EDGE('',*,*,#16189,.F.);
#22271=ORIENTED_EDGE('',*,*,#16190,.F.);
#22272=ORIENTED_EDGE('',*,*,#16191,.F.);
#22273=ORIENTED_EDGE('',*,*,#16192,.F.);
#22274=ORIENTED_EDGE('',*,*,#16193,.F.);
#22275=ORIENTED_EDGE('',*,*,#16194,.F.);
#22276=ORIENTED_EDGE('',*,*,#16195,.F.);
#22277=ORIENTED_EDGE('',*,*,#15409,.F.);
#22278=ORIENTED_EDGE('',*,*,#16196,.F.);
#22279=ORIENTED_EDGE('',*,*,#16081,.T.);
#22280=ORIENTED_EDGE('',*,*,#16074,.F.);
#22281=ORIENTED_EDGE('',*,*,#15425,.F.);
#22282=ORIENTED_EDGE('',*,*,#15423,.T.);
#22283=ORIENTED_EDGE('',*,*,#15449,.F.);
#22284=ORIENTED_EDGE('',*,*,#16197,.T.);
#22285=ORIENTED_EDGE('',*,*,#16193,.T.);
#22286=ORIENTED_EDGE('',*,*,#16198,.T.);
#22287=ORIENTED_EDGE('',*,*,#15622,.T.);
#22288=ORIENTED_EDGE('',*,*,#16192,.T.);
#22289=ORIENTED_EDGE('',*,*,#16199,.T.);
#22290=ORIENTED_EDGE('',*,*,#15621,.T.);
#22291=ORIENTED_EDGE('',*,*,#16198,.F.);
#22292=ORIENTED_EDGE('',*,*,#15460,.F.);
#22293=ORIENTED_EDGE('',*,*,#15619,.T.);
#22294=ORIENTED_EDGE('',*,*,#16199,.F.);
#22295=ORIENTED_EDGE('',*,*,#16191,.T.);
#22296=ORIENTED_EDGE('',*,*,#16200,.T.);
#22297=ORIENTED_EDGE('',*,*,#15432,.F.);
#22298=ORIENTED_EDGE('',*,*,#16080,.F.);
#22299=ORIENTED_EDGE('',*,*,#16194,.T.);
#22300=ORIENTED_EDGE('',*,*,#16197,.F.);
#22301=ORIENTED_EDGE('',*,*,#15448,.F.);
#22302=ORIENTED_EDGE('',*,*,#15446,.T.);
#22303=ORIENTED_EDGE('',*,*,#15472,.F.);
#22304=ORIENTED_EDGE('',*,*,#16201,.T.);
#22305=ORIENTED_EDGE('',*,*,#16189,.T.);
#22306=ORIENTED_EDGE('',*,*,#16202,.T.);
#22307=ORIENTED_EDGE('',*,*,#15616,.T.);
#22308=ORIENTED_EDGE('',*,*,#16188,.T.);
#22309=ORIENTED_EDGE('',*,*,#16203,.T.);
#22310=ORIENTED_EDGE('',*,*,#15615,.T.);
#22311=ORIENTED_EDGE('',*,*,#16202,.F.);
#22312=ORIENTED_EDGE('',*,*,#15483,.F.);
#22313=ORIENTED_EDGE('',*,*,#15613,.T.);
#22314=ORIENTED_EDGE('',*,*,#16203,.F.);
#22315=ORIENTED_EDGE('',*,*,#16187,.T.);
#22316=ORIENTED_EDGE('',*,*,#16204,.T.);
#22317=ORIENTED_EDGE('',*,*,#15455,.F.);
#22318=ORIENTED_EDGE('',*,*,#16200,.F.);
#22319=ORIENTED_EDGE('',*,*,#16190,.T.);
#22320=ORIENTED_EDGE('',*,*,#16201,.F.);
#22321=ORIENTED_EDGE('',*,*,#15471,.F.);
#22322=ORIENTED_EDGE('',*,*,#15469,.T.);
#22323=ORIENTED_EDGE('',*,*,#15495,.F.);
#22324=ORIENTED_EDGE('',*,*,#16205,.T.);
#22325=ORIENTED_EDGE('',*,*,#16185,.T.);
#22326=ORIENTED_EDGE('',*,*,#16206,.T.);
#22327=ORIENTED_EDGE('',*,*,#15610,.T.);
#22328=ORIENTED_EDGE('',*,*,#16184,.T.);
#22329=ORIENTED_EDGE('',*,*,#16207,.T.);
#22330=ORIENTED_EDGE('',*,*,#15609,.T.);
#22331=ORIENTED_EDGE('',*,*,#16206,.F.);
#22332=ORIENTED_EDGE('',*,*,#15506,.F.);
#22333=ORIENTED_EDGE('',*,*,#15509,.T.);
#22334=ORIENTED_EDGE('',*,*,#16207,.F.);
#22335=ORIENTED_EDGE('',*,*,#16183,.T.);
#22336=ORIENTED_EDGE('',*,*,#16208,.T.);
#22337=ORIENTED_EDGE('',*,*,#15478,.F.);
#22338=ORIENTED_EDGE('',*,*,#16204,.F.);
#22339=ORIENTED_EDGE('',*,*,#16186,.T.);
#22340=ORIENTED_EDGE('',*,*,#16205,.F.);
#22341=ORIENTED_EDGE('',*,*,#15494,.F.);
#22342=ORIENTED_EDGE('',*,*,#15492,.T.);
#22343=ORIENTED_EDGE('',*,*,#16181,.T.);
#22344=ORIENTED_EDGE('',*,*,#16209,.T.);
#22345=ORIENTED_EDGE('',*,*,#15531,.T.);
#22346=ORIENTED_EDGE('',*,*,#15083,.F.);
#22347=ORIENTED_EDGE('',*,*,#15309,.F.);
#22348=ORIENTED_EDGE('',*,*,#15530,.T.);
#22349=ORIENTED_EDGE('',*,*,#16209,.F.);
#22350=ORIENTED_EDGE('',*,*,#16180,.T.);
#22351=ORIENTED_EDGE('',*,*,#16210,.T.);
#22352=ORIENTED_EDGE('',*,*,#15071,.F.);
#22353=ORIENTED_EDGE('',*,*,#16211,.T.);
#22354=ORIENTED_EDGE('',*,*,#15501,.F.);
#22355=ORIENTED_EDGE('',*,*,#16208,.F.);
#22356=ORIENTED_EDGE('',*,*,#16182,.T.);
#22357=ORIENTED_EDGE('',*,*,#15081,.F.);
#22358=ORIENTED_EDGE('',*,*,#15321,.F.);
#22359=ORIENTED_EDGE('',*,*,#16212,.T.);
#22360=ORIENTED_EDGE('',*,*,#16178,.T.);
#22361=ORIENTED_EDGE('',*,*,#16213,.T.);
#22362=ORIENTED_EDGE('',*,*,#15526,.T.);
#22363=ORIENTED_EDGE('',*,*,#16177,.T.);
#22364=ORIENTED_EDGE('',*,*,#16214,.T.);
#22365=ORIENTED_EDGE('',*,*,#15525,.T.);
#22366=ORIENTED_EDGE('',*,*,#16213,.F.);
#22367=ORIENTED_EDGE('',*,*,#15332,.F.);
#22368=ORIENTED_EDGE('',*,*,#15523,.T.);
#22369=ORIENTED_EDGE('',*,*,#16214,.F.);
#22370=ORIENTED_EDGE('',*,*,#16176,.T.);
#22371=ORIENTED_EDGE('',*,*,#16215,.T.);
#22372=ORIENTED_EDGE('',*,*,#15304,.F.);
#22373=ORIENTED_EDGE('',*,*,#16210,.F.);
#22374=ORIENTED_EDGE('',*,*,#16179,.T.);
#22375=ORIENTED_EDGE('',*,*,#16212,.F.);
#22376=ORIENTED_EDGE('',*,*,#15320,.F.);
#22377=ORIENTED_EDGE('',*,*,#15318,.T.);
#22378=ORIENTED_EDGE('',*,*,#15344,.F.);
#22379=ORIENTED_EDGE('',*,*,#16216,.T.);
#22380=ORIENTED_EDGE('',*,*,#16174,.T.);
#22381=ORIENTED_EDGE('',*,*,#16217,.T.);
#22382=ORIENTED_EDGE('',*,*,#15519,.T.);
#22383=ORIENTED_EDGE('',*,*,#15518,.T.);
#22384=ORIENTED_EDGE('',*,*,#16217,.F.);
#22385=ORIENTED_EDGE('',*,*,#16173,.T.);
#22386=ORIENTED_EDGE('',*,*,#15356,.T.);
#22387=ORIENTED_EDGE('',*,*,#16172,.T.);
#22388=ORIENTED_EDGE('',*,*,#16218,.T.);
#22389=ORIENTED_EDGE('',*,*,#16072,.T.);
#22390=ORIENTED_EDGE('',*,*,#15064,.F.);
#22391=ORIENTED_EDGE('',*,*,#15908,.F.);
#22392=ORIENTED_EDGE('',*,*,#16071,.T.);
#22393=ORIENTED_EDGE('',*,*,#16218,.F.);
#22394=ORIENTED_EDGE('',*,*,#16171,.T.);
#22395=ORIENTED_EDGE('',*,*,#16219,.T.);
#22396=ORIENTED_EDGE('',*,*,#15918,.F.);
#22397=ORIENTED_EDGE('',*,*,#16220,.T.);
#22398=ORIENTED_EDGE('',*,*,#16169,.T.);
#22399=ORIENTED_EDGE('',*,*,#16221,.T.);
#22400=ORIENTED_EDGE('',*,*,#16067,.T.);
#22401=ORIENTED_EDGE('',*,*,#16168,.T.);
#22402=ORIENTED_EDGE('',*,*,#16222,.T.);
#22403=ORIENTED_EDGE('',*,*,#16066,.T.);
#22404=ORIENTED_EDGE('',*,*,#16221,.F.);
#22405=ORIENTED_EDGE('',*,*,#15928,.F.);
#22406=ORIENTED_EDGE('',*,*,#16064,.T.);
#22407=ORIENTED_EDGE('',*,*,#16222,.F.);
#22408=ORIENTED_EDGE('',*,*,#16167,.T.);
#22409=ORIENTED_EDGE('',*,*,#16223,.T.);
#22410=ORIENTED_EDGE('',*,*,#15903,.F.);
#22411=ORIENTED_EDGE('',*,*,#16219,.F.);
#22412=ORIENTED_EDGE('',*,*,#16170,.T.);
#22413=ORIENTED_EDGE('',*,*,#16220,.F.);
#22414=ORIENTED_EDGE('',*,*,#15917,.F.);
#22415=ORIENTED_EDGE('',*,*,#15915,.T.);
#22416=ORIENTED_EDGE('',*,*,#15938,.F.);
#22417=ORIENTED_EDGE('',*,*,#16224,.T.);
#22418=ORIENTED_EDGE('',*,*,#16165,.T.);
#22419=ORIENTED_EDGE('',*,*,#16225,.T.);
#22420=ORIENTED_EDGE('',*,*,#16061,.T.);
#22421=ORIENTED_EDGE('',*,*,#16164,.T.);
#22422=ORIENTED_EDGE('',*,*,#16226,.T.);
#22423=ORIENTED_EDGE('',*,*,#16060,.T.);
#22424=ORIENTED_EDGE('',*,*,#16225,.F.);
#22425=ORIENTED_EDGE('',*,*,#15948,.F.);
#22426=ORIENTED_EDGE('',*,*,#16058,.T.);
#22427=ORIENTED_EDGE('',*,*,#16226,.F.);
#22428=ORIENTED_EDGE('',*,*,#16163,.T.);
#22429=ORIENTED_EDGE('',*,*,#16227,.T.);
#22430=ORIENTED_EDGE('',*,*,#15923,.F.);
#22431=ORIENTED_EDGE('',*,*,#16223,.F.);
#22432=ORIENTED_EDGE('',*,*,#16166,.T.);
#22433=ORIENTED_EDGE('',*,*,#16224,.F.);
#22434=ORIENTED_EDGE('',*,*,#15937,.F.);
#22435=ORIENTED_EDGE('',*,*,#15935,.T.);
#22436=ORIENTED_EDGE('',*,*,#15958,.F.);
#22437=ORIENTED_EDGE('',*,*,#16228,.T.);
#22438=ORIENTED_EDGE('',*,*,#16161,.T.);
#22439=ORIENTED_EDGE('',*,*,#16229,.T.);
#22440=ORIENTED_EDGE('',*,*,#16055,.T.);
#22441=ORIENTED_EDGE('',*,*,#16160,.T.);
#22442=ORIENTED_EDGE('',*,*,#16230,.T.);
#22443=ORIENTED_EDGE('',*,*,#16054,.T.);
#22444=ORIENTED_EDGE('',*,*,#16229,.F.);
#22445=ORIENTED_EDGE('',*,*,#15968,.F.);
#22446=ORIENTED_EDGE('',*,*,#16052,.T.);
#22447=ORIENTED_EDGE('',*,*,#16230,.F.);
#22448=ORIENTED_EDGE('',*,*,#16159,.T.);
#22449=ORIENTED_EDGE('',*,*,#16231,.T.);
#22450=ORIENTED_EDGE('',*,*,#15943,.F.);
#22451=ORIENTED_EDGE('',*,*,#16227,.F.);
#22452=ORIENTED_EDGE('',*,*,#16162,.T.);
#22453=ORIENTED_EDGE('',*,*,#16228,.F.);
#22454=ORIENTED_EDGE('',*,*,#15957,.F.);
#22455=ORIENTED_EDGE('',*,*,#15955,.T.);
#22456=ORIENTED_EDGE('',*,*,#15978,.F.);
#22457=ORIENTED_EDGE('',*,*,#16232,.T.);
#22458=ORIENTED_EDGE('',*,*,#16157,.T.);
#22459=ORIENTED_EDGE('',*,*,#16233,.T.);
#22460=ORIENTED_EDGE('',*,*,#16049,.T.);
#22461=ORIENTED_EDGE('',*,*,#16156,.T.);
#22462=ORIENTED_EDGE('',*,*,#16234,.T.);
#22463=ORIENTED_EDGE('',*,*,#16048,.T.);
#22464=ORIENTED_EDGE('',*,*,#16233,.F.);
#22465=ORIENTED_EDGE('',*,*,#15988,.F.);
#22466=ORIENTED_EDGE('',*,*,#16046,.T.);
#22467=ORIENTED_EDGE('',*,*,#16234,.F.);
#22468=ORIENTED_EDGE('',*,*,#16155,.T.);
#22469=ORIENTED_EDGE('',*,*,#16235,.T.);
#22470=ORIENTED_EDGE('',*,*,#15963,.F.);
#22471=ORIENTED_EDGE('',*,*,#16231,.F.);
#22472=ORIENTED_EDGE('',*,*,#16158,.T.);
#22473=ORIENTED_EDGE('',*,*,#16232,.F.);
#22474=ORIENTED_EDGE('',*,*,#15977,.F.);
#22475=ORIENTED_EDGE('',*,*,#15975,.T.);
#22476=ORIENTED_EDGE('',*,*,#15998,.F.);
#22477=ORIENTED_EDGE('',*,*,#16236,.T.);
#22478=ORIENTED_EDGE('',*,*,#16153,.T.);
#22479=ORIENTED_EDGE('',*,*,#16237,.T.);
#22480=ORIENTED_EDGE('',*,*,#16043,.T.);
#22481=ORIENTED_EDGE('',*,*,#16152,.T.);
#22482=ORIENTED_EDGE('',*,*,#16238,.T.);
#22483=ORIENTED_EDGE('',*,*,#16042,.T.);
#22484=ORIENTED_EDGE('',*,*,#16237,.F.);
#22485=ORIENTED_EDGE('',*,*,#16008,.F.);
#22486=ORIENTED_EDGE('',*,*,#16040,.T.);
#22487=ORIENTED_EDGE('',*,*,#16238,.F.);
#22488=ORIENTED_EDGE('',*,*,#16151,.T.);
#22489=ORIENTED_EDGE('',*,*,#16239,.T.);
#22490=ORIENTED_EDGE('',*,*,#15983,.F.);
#22491=ORIENTED_EDGE('',*,*,#16235,.F.);
#22492=ORIENTED_EDGE('',*,*,#16154,.T.);
#22493=ORIENTED_EDGE('',*,*,#16236,.F.);
#22494=ORIENTED_EDGE('',*,*,#15997,.F.);
#22495=ORIENTED_EDGE('',*,*,#15995,.T.);
#22496=ORIENTED_EDGE('',*,*,#16018,.F.);
#22497=ORIENTED_EDGE('',*,*,#16240,.T.);
#22498=ORIENTED_EDGE('',*,*,#16149,.T.);
#22499=ORIENTED_EDGE('',*,*,#16241,.T.);
#22500=ORIENTED_EDGE('',*,*,#16037,.T.);
#22501=ORIENTED_EDGE('',*,*,#16148,.T.);
#22502=ORIENTED_EDGE('',*,*,#16028,.T.);
#22503=ORIENTED_EDGE('',*,*,#16036,.T.);
#22504=ORIENTED_EDGE('',*,*,#16241,.F.);
#22505=ORIENTED_EDGE('',*,*,#16003,.F.);
#22506=ORIENTED_EDGE('',*,*,#16239,.F.);
#22507=ORIENTED_EDGE('',*,*,#16150,.T.);
#22508=ORIENTED_EDGE('',*,*,#16240,.F.);
#22509=ORIENTED_EDGE('',*,*,#16017,.F.);
#22510=ORIENTED_EDGE('',*,*,#16015,.T.);
#22511=ORIENTED_EDGE('',*,*,#15087,.F.);
#22512=ORIENTED_EDGE('',*,*,#16242,.T.);
#22513=ORIENTED_EDGE('',*,*,#16146,.T.);
#22514=ORIENTED_EDGE('',*,*,#16243,.T.);
#22515=ORIENTED_EDGE('',*,*,#15902,.T.);
#22516=ORIENTED_EDGE('',*,*,#16145,.T.);
#22517=ORIENTED_EDGE('',*,*,#16244,.T.);
#22518=ORIENTED_EDGE('',*,*,#15901,.T.);
#22519=ORIENTED_EDGE('',*,*,#16243,.F.);
#22520=ORIENTED_EDGE('',*,*,#15105,.F.);
#22521=ORIENTED_EDGE('',*,*,#15899,.T.);
#22522=ORIENTED_EDGE('',*,*,#16244,.F.);
#22523=ORIENTED_EDGE('',*,*,#16144,.T.);
#22524=ORIENTED_EDGE('',*,*,#16245,.T.);
#22525=ORIENTED_EDGE('',*,*,#15086,.F.);
#22526=ORIENTED_EDGE('',*,*,#15092,.T.);
#22527=ORIENTED_EDGE('',*,*,#16023,.F.);
#22528=ORIENTED_EDGE('',*,*,#16030,.F.);
#22529=ORIENTED_EDGE('',*,*,#16147,.T.);
#22530=ORIENTED_EDGE('',*,*,#16242,.F.);
#22531=ORIENTED_EDGE('',*,*,#15117,.F.);
#22532=ORIENTED_EDGE('',*,*,#16246,.T.);
#22533=ORIENTED_EDGE('',*,*,#16142,.T.);
#22534=ORIENTED_EDGE('',*,*,#16247,.T.);
#22535=ORIENTED_EDGE('',*,*,#15896,.T.);
#22536=ORIENTED_EDGE('',*,*,#16141,.T.);
#22537=ORIENTED_EDGE('',*,*,#16248,.T.);
#22538=ORIENTED_EDGE('',*,*,#15895,.T.);
#22539=ORIENTED_EDGE('',*,*,#16247,.F.);
#22540=ORIENTED_EDGE('',*,*,#15128,.F.);
#22541=ORIENTED_EDGE('',*,*,#15131,.T.);
#22542=ORIENTED_EDGE('',*,*,#16248,.F.);
#22543=ORIENTED_EDGE('',*,*,#16140,.T.);
#22544=ORIENTED_EDGE('',*,*,#16249,.T.);
#22545=ORIENTED_EDGE('',*,*,#15100,.F.);
#22546=ORIENTED_EDGE('',*,*,#16245,.F.);
#22547=ORIENTED_EDGE('',*,*,#16143,.T.);
#22548=ORIENTED_EDGE('',*,*,#16246,.F.);
#22549=ORIENTED_EDGE('',*,*,#15116,.F.);
#22550=ORIENTED_EDGE('',*,*,#15114,.T.);
#22551=ORIENTED_EDGE('',*,*,#16138,.T.);
#22552=ORIENTED_EDGE('',*,*,#16250,.T.);
#22553=ORIENTED_EDGE('',*,*,#15892,.T.);
#22554=ORIENTED_EDGE('',*,*,#15052,.F.);
#22555=ORIENTED_EDGE('',*,*,#15724,.F.);
#22556=ORIENTED_EDGE('',*,*,#15891,.T.);
#22557=ORIENTED_EDGE('',*,*,#16250,.F.);
#22558=ORIENTED_EDGE('',*,*,#16137,.T.);
#22559=ORIENTED_EDGE('',*,*,#16251,.T.);
#22560=ORIENTED_EDGE('',*,*,#15040,.F.);
#22561=ORIENTED_EDGE('',*,*,#16252,.T.);
#22562=ORIENTED_EDGE('',*,*,#15123,.F.);
#22563=ORIENTED_EDGE('',*,*,#16249,.F.);
#22564=ORIENTED_EDGE('',*,*,#16139,.T.);
#22565=ORIENTED_EDGE('',*,*,#15050,.F.);
#22566=ORIENTED_EDGE('',*,*,#15734,.F.);
#22567=ORIENTED_EDGE('',*,*,#16253,.T.);
#22568=ORIENTED_EDGE('',*,*,#16135,.T.);
#22569=ORIENTED_EDGE('',*,*,#16254,.T.);
#22570=ORIENTED_EDGE('',*,*,#15888,.T.);
#22571=ORIENTED_EDGE('',*,*,#16134,.T.);
#22572=ORIENTED_EDGE('',*,*,#16255,.T.);
#22573=ORIENTED_EDGE('',*,*,#15887,.T.);
#22574=ORIENTED_EDGE('',*,*,#16254,.F.);
#22575=ORIENTED_EDGE('',*,*,#15744,.F.);
#22576=ORIENTED_EDGE('',*,*,#15885,.T.);
#22577=ORIENTED_EDGE('',*,*,#16255,.F.);
#22578=ORIENTED_EDGE('',*,*,#16133,.T.);
#22579=ORIENTED_EDGE('',*,*,#16256,.T.);
#22580=ORIENTED_EDGE('',*,*,#15719,.F.);
#22581=ORIENTED_EDGE('',*,*,#16251,.F.);
#22582=ORIENTED_EDGE('',*,*,#16136,.T.);
#22583=ORIENTED_EDGE('',*,*,#16253,.F.);
#22584=ORIENTED_EDGE('',*,*,#15733,.F.);
#22585=ORIENTED_EDGE('',*,*,#15731,.T.);
#22586=ORIENTED_EDGE('',*,*,#15754,.F.);
#22587=ORIENTED_EDGE('',*,*,#16257,.T.);
#22588=ORIENTED_EDGE('',*,*,#16131,.T.);
#22589=ORIENTED_EDGE('',*,*,#16258,.T.);
#22590=ORIENTED_EDGE('',*,*,#15882,.T.);
#22591=ORIENTED_EDGE('',*,*,#16130,.T.);
#22592=ORIENTED_EDGE('',*,*,#16259,.T.);
#22593=ORIENTED_EDGE('',*,*,#15881,.T.);
#22594=ORIENTED_EDGE('',*,*,#16258,.F.);
#22595=ORIENTED_EDGE('',*,*,#15764,.F.);
#22596=ORIENTED_EDGE('',*,*,#15879,.T.);
#22597=ORIENTED_EDGE('',*,*,#16259,.F.);
#22598=ORIENTED_EDGE('',*,*,#16129,.T.);
#22599=ORIENTED_EDGE('',*,*,#16260,.T.);
#22600=ORIENTED_EDGE('',*,*,#15739,.F.);
#22601=ORIENTED_EDGE('',*,*,#16256,.F.);
#22602=ORIENTED_EDGE('',*,*,#16132,.T.);
#22603=ORIENTED_EDGE('',*,*,#16257,.F.);
#22604=ORIENTED_EDGE('',*,*,#15753,.F.);
#22605=ORIENTED_EDGE('',*,*,#15751,.T.);
#22606=ORIENTED_EDGE('',*,*,#15774,.F.);
#22607=ORIENTED_EDGE('',*,*,#16261,.T.);
#22608=ORIENTED_EDGE('',*,*,#16127,.T.);
#22609=ORIENTED_EDGE('',*,*,#16262,.T.);
#22610=ORIENTED_EDGE('',*,*,#15876,.T.);
#22611=ORIENTED_EDGE('',*,*,#16126,.T.);
#22612=ORIENTED_EDGE('',*,*,#16263,.T.);
#22613=ORIENTED_EDGE('',*,*,#15875,.T.);
#22614=ORIENTED_EDGE('',*,*,#16262,.F.);
#22615=ORIENTED_EDGE('',*,*,#15784,.F.);
#22616=ORIENTED_EDGE('',*,*,#15787,.T.);
#22617=ORIENTED_EDGE('',*,*,#16263,.F.);
#22618=ORIENTED_EDGE('',*,*,#16125,.T.);
#22619=ORIENTED_EDGE('',*,*,#15804,.T.);
#22620=ORIENTED_EDGE('',*,*,#16124,.T.);
#22621=ORIENTED_EDGE('',*,*,#16264,.T.);
#22622=ORIENTED_EDGE('',*,*,#15872,.T.);
#22623=ORIENTED_EDGE('',*,*,#15803,.F.);
#22624=ORIENTED_EDGE('',*,*,#15812,.F.);
#22625=ORIENTED_EDGE('',*,*,#15871,.T.);
#22626=ORIENTED_EDGE('',*,*,#16264,.F.);
#22627=ORIENTED_EDGE('',*,*,#16123,.T.);
#22628=ORIENTED_EDGE('',*,*,#16265,.T.);
#22629=ORIENTED_EDGE('',*,*,#15822,.F.);
#22630=ORIENTED_EDGE('',*,*,#16266,.T.);
#22631=ORIENTED_EDGE('',*,*,#16121,.T.);
#22632=ORIENTED_EDGE('',*,*,#16267,.T.);
#22633=ORIENTED_EDGE('',*,*,#15867,.T.);
#22634=ORIENTED_EDGE('',*,*,#16120,.T.);
#22635=ORIENTED_EDGE('',*,*,#16268,.T.);
#22636=ORIENTED_EDGE('',*,*,#15866,.T.);
#22637=ORIENTED_EDGE('',*,*,#16267,.F.);
#22638=ORIENTED_EDGE('',*,*,#15832,.F.);
#22639=ORIENTED_EDGE('',*,*,#15864,.T.);
#22640=ORIENTED_EDGE('',*,*,#16268,.F.);
#22641=ORIENTED_EDGE('',*,*,#16119,.T.);
#22642=ORIENTED_EDGE('',*,*,#16269,.T.);
#22643=ORIENTED_EDGE('',*,*,#15807,.F.);
#22644=ORIENTED_EDGE('',*,*,#16265,.F.);
#22645=ORIENTED_EDGE('',*,*,#16122,.T.);
#22646=ORIENTED_EDGE('',*,*,#16266,.F.);
#22647=ORIENTED_EDGE('',*,*,#15821,.F.);
#22648=ORIENTED_EDGE('',*,*,#15819,.T.);
#22649=ORIENTED_EDGE('',*,*,#15842,.F.);
#22650=ORIENTED_EDGE('',*,*,#16270,.T.);
#22651=ORIENTED_EDGE('',*,*,#16117,.T.);
#22652=ORIENTED_EDGE('',*,*,#16271,.T.);
#22653=ORIENTED_EDGE('',*,*,#15861,.T.);
#22654=ORIENTED_EDGE('',*,*,#16116,.T.);
#22655=ORIENTED_EDGE('',*,*,#15852,.T.);
#22656=ORIENTED_EDGE('',*,*,#15860,.T.);
#22657=ORIENTED_EDGE('',*,*,#16271,.F.);
#22658=ORIENTED_EDGE('',*,*,#15827,.F.);
#22659=ORIENTED_EDGE('',*,*,#16269,.F.);
#22660=ORIENTED_EDGE('',*,*,#16118,.T.);
#22661=ORIENTED_EDGE('',*,*,#16270,.F.);
#22662=ORIENTED_EDGE('',*,*,#15841,.F.);
#22663=ORIENTED_EDGE('',*,*,#15839,.T.);
#22664=ORIENTED_EDGE('',*,*,#15140,.F.);
#22665=ORIENTED_EDGE('',*,*,#16272,.T.);
#22666=ORIENTED_EDGE('',*,*,#16114,.T.);
#22667=ORIENTED_EDGE('',*,*,#16273,.T.);
#22668=ORIENTED_EDGE('',*,*,#15718,.T.);
#22669=ORIENTED_EDGE('',*,*,#16113,.T.);
#22670=ORIENTED_EDGE('',*,*,#16274,.T.);
#22671=ORIENTED_EDGE('',*,*,#15717,.T.);
#22672=ORIENTED_EDGE('',*,*,#16273,.F.);
#22673=ORIENTED_EDGE('',*,*,#15158,.F.);
#22674=ORIENTED_EDGE('',*,*,#15715,.T.);
#22675=ORIENTED_EDGE('',*,*,#16274,.F.);
#22676=ORIENTED_EDGE('',*,*,#16112,.T.);
#22677=ORIENTED_EDGE('',*,*,#16275,.T.);
#22678=ORIENTED_EDGE('',*,*,#15139,.F.);
#22679=ORIENTED_EDGE('',*,*,#15145,.T.);
#22680=ORIENTED_EDGE('',*,*,#15847,.F.);
#22681=ORIENTED_EDGE('',*,*,#15854,.F.);
#22682=ORIENTED_EDGE('',*,*,#16115,.T.);
#22683=ORIENTED_EDGE('',*,*,#16272,.F.);
#22684=ORIENTED_EDGE('',*,*,#15170,.F.);
#22685=ORIENTED_EDGE('',*,*,#16276,.T.);
#22686=ORIENTED_EDGE('',*,*,#16110,.T.);
#22687=ORIENTED_EDGE('',*,*,#16277,.T.);
#22688=ORIENTED_EDGE('',*,*,#15712,.T.);
#22689=ORIENTED_EDGE('',*,*,#16109,.T.);
#22690=ORIENTED_EDGE('',*,*,#16278,.T.);
#22691=ORIENTED_EDGE('',*,*,#15711,.T.);
#22692=ORIENTED_EDGE('',*,*,#16277,.F.);
#22693=ORIENTED_EDGE('',*,*,#15181,.F.);
#22694=ORIENTED_EDGE('',*,*,#15184,.T.);
#22695=ORIENTED_EDGE('',*,*,#16278,.F.);
#22696=ORIENTED_EDGE('',*,*,#16108,.T.);
#22697=ORIENTED_EDGE('',*,*,#16279,.T.);
#22698=ORIENTED_EDGE('',*,*,#15153,.F.);
#22699=ORIENTED_EDGE('',*,*,#16275,.F.);
#22700=ORIENTED_EDGE('',*,*,#16111,.T.);
#22701=ORIENTED_EDGE('',*,*,#16276,.F.);
#22702=ORIENTED_EDGE('',*,*,#15169,.F.);
#22703=ORIENTED_EDGE('',*,*,#15167,.T.);
#22704=ORIENTED_EDGE('',*,*,#16106,.T.);
#22705=ORIENTED_EDGE('',*,*,#16280,.T.);
#22706=ORIENTED_EDGE('',*,*,#15708,.T.);
#22707=ORIENTED_EDGE('',*,*,#15037,.F.);
#22708=ORIENTED_EDGE('',*,*,#15195,.F.);
#22709=ORIENTED_EDGE('',*,*,#15707,.T.);
#22710=ORIENTED_EDGE('',*,*,#16280,.F.);
#22711=ORIENTED_EDGE('',*,*,#16105,.T.);
#22712=ORIENTED_EDGE('',*,*,#16281,.T.);
#22713=ORIENTED_EDGE('',*,*,#15025,.F.);
#22714=ORIENTED_EDGE('',*,*,#16282,.T.);
#22715=ORIENTED_EDGE('',*,*,#15176,.F.);
#22716=ORIENTED_EDGE('',*,*,#16279,.F.);
#22717=ORIENTED_EDGE('',*,*,#16107,.T.);
#22718=ORIENTED_EDGE('',*,*,#15035,.F.);
#22719=ORIENTED_EDGE('',*,*,#15207,.F.);
#22720=ORIENTED_EDGE('',*,*,#16283,.T.);
#22721=ORIENTED_EDGE('',*,*,#16103,.T.);
#22722=ORIENTED_EDGE('',*,*,#16284,.T.);
#22723=ORIENTED_EDGE('',*,*,#15704,.T.);
#22724=ORIENTED_EDGE('',*,*,#15703,.T.);
#22725=ORIENTED_EDGE('',*,*,#16284,.F.);
#22726=ORIENTED_EDGE('',*,*,#16102,.T.);
#22727=ORIENTED_EDGE('',*,*,#16285,.T.);
#22728=ORIENTED_EDGE('',*,*,#15218,.F.);
#22729=ORIENTED_EDGE('',*,*,#15221,.T.);
#22730=ORIENTED_EDGE('',*,*,#16285,.F.);
#22731=ORIENTED_EDGE('',*,*,#16101,.T.);
#22732=ORIENTED_EDGE('',*,*,#15240,.T.);
#22733=ORIENTED_EDGE('',*,*,#16100,.T.);
#22734=ORIENTED_EDGE('',*,*,#16286,.T.);
#22735=ORIENTED_EDGE('',*,*,#15700,.T.);
#22736=ORIENTED_EDGE('',*,*,#15239,.F.);
#22737=ORIENTED_EDGE('',*,*,#15248,.F.);
#22738=ORIENTED_EDGE('',*,*,#15699,.T.);
#22739=ORIENTED_EDGE('',*,*,#16286,.F.);
#22740=ORIENTED_EDGE('',*,*,#16099,.T.);
#22741=ORIENTED_EDGE('',*,*,#16287,.T.);
#22742=ORIENTED_EDGE('',*,*,#15260,.F.);
#22743=ORIENTED_EDGE('',*,*,#16288,.T.);
#22744=ORIENTED_EDGE('',*,*,#16097,.T.);
#22745=ORIENTED_EDGE('',*,*,#16289,.T.);
#22746=ORIENTED_EDGE('',*,*,#15695,.T.);
#22747=ORIENTED_EDGE('',*,*,#16096,.T.);
#22748=ORIENTED_EDGE('',*,*,#16290,.T.);
#22749=ORIENTED_EDGE('',*,*,#15694,.T.);
#22750=ORIENTED_EDGE('',*,*,#16289,.F.);
#22751=ORIENTED_EDGE('',*,*,#15271,.F.);
#22752=ORIENTED_EDGE('',*,*,#15692,.T.);
#22753=ORIENTED_EDGE('',*,*,#16290,.F.);
#22754=ORIENTED_EDGE('',*,*,#16095,.T.);
#22755=ORIENTED_EDGE('',*,*,#16291,.T.);
#22756=ORIENTED_EDGE('',*,*,#15243,.F.);
#22757=ORIENTED_EDGE('',*,*,#16287,.F.);
#22758=ORIENTED_EDGE('',*,*,#16098,.T.);
#22759=ORIENTED_EDGE('',*,*,#16288,.F.);
#22760=ORIENTED_EDGE('',*,*,#15259,.F.);
#22761=ORIENTED_EDGE('',*,*,#15257,.T.);
#22762=ORIENTED_EDGE('',*,*,#15283,.F.);
#22763=ORIENTED_EDGE('',*,*,#16292,.T.);
#22764=ORIENTED_EDGE('',*,*,#16093,.T.);
#22765=ORIENTED_EDGE('',*,*,#16293,.T.);
#22766=ORIENTED_EDGE('',*,*,#15689,.T.);
#22767=ORIENTED_EDGE('',*,*,#16092,.T.);
#22768=ORIENTED_EDGE('',*,*,#15296,.T.);
#22769=ORIENTED_EDGE('',*,*,#15688,.T.);
#22770=ORIENTED_EDGE('',*,*,#16293,.F.);
#22771=ORIENTED_EDGE('',*,*,#15266,.F.);
#22772=ORIENTED_EDGE('',*,*,#16291,.F.);
#22773=ORIENTED_EDGE('',*,*,#16094,.T.);
#22774=ORIENTED_EDGE('',*,*,#16292,.F.);
#22775=ORIENTED_EDGE('',*,*,#15282,.F.);
#22776=ORIENTED_EDGE('',*,*,#15280,.T.);
#22777=ORIENTED_EDGE('',*,*,#15377,.F.);
#22778=ORIENTED_EDGE('',*,*,#15372,.T.);
#22779=ORIENTED_EDGE('',*,*,#16294,.T.);
#22780=ORIENTED_EDGE('',*,*,#16295,.T.);
#22781=ORIENTED_EDGE('',*,*,#16090,.T.);
#22782=ORIENTED_EDGE('',*,*,#15651,.T.);
#22783=ORIENTED_EDGE('',*,*,#15655,.F.);
#22784=ORIENTED_EDGE('',*,*,#16296,.T.);
#22785=ORIENTED_EDGE('',*,*,#16088,.T.);
#22786=ORIENTED_EDGE('',*,*,#16297,.T.);
#22787=ORIENTED_EDGE('',*,*,#15685,.T.);
#22788=ORIENTED_EDGE('',*,*,#16087,.T.);
#22789=ORIENTED_EDGE('',*,*,#16298,.T.);
#22790=ORIENTED_EDGE('',*,*,#15684,.T.);
#22791=ORIENTED_EDGE('',*,*,#16297,.F.);
#22792=ORIENTED_EDGE('',*,*,#15665,.F.);
#22793=ORIENTED_EDGE('',*,*,#15682,.T.);
#22794=ORIENTED_EDGE('',*,*,#16298,.F.);
#22795=ORIENTED_EDGE('',*,*,#16086,.T.);
#22796=ORIENTED_EDGE('',*,*,#16299,.T.);
#22797=ORIENTED_EDGE('',*,*,#15396,.F.);
#22798=ORIENTED_EDGE('',*,*,#15650,.F.);
#22799=ORIENTED_EDGE('',*,*,#16089,.T.);
#22800=ORIENTED_EDGE('',*,*,#16296,.F.);
#22801=ORIENTED_EDGE('',*,*,#15654,.F.);
#22802=ORIENTED_EDGE('',*,*,#15407,.T.);
#22803=ORIENTED_EDGE('',*,*,#15675,.F.);
#22804=ORIENTED_EDGE('',*,*,#16300,.T.);
#22805=ORIENTED_EDGE('',*,*,#16084,.T.);
#22806=ORIENTED_EDGE('',*,*,#16301,.T.);
#22807=ORIENTED_EDGE('',*,*,#15679,.T.);
#22808=ORIENTED_EDGE('',*,*,#16083,.T.);
#22809=ORIENTED_EDGE('',*,*,#16302,.T.);
#22810=ORIENTED_EDGE('',*,*,#15634,.T.);
#22811=ORIENTED_EDGE('',*,*,#16301,.F.);
#22812=ORIENTED_EDGE('',*,*,#15414,.F.);
#22813=ORIENTED_EDGE('',*,*,#15632,.T.);
#22814=ORIENTED_EDGE('',*,*,#16302,.F.);
#22815=ORIENTED_EDGE('',*,*,#16082,.T.);
#22816=ORIENTED_EDGE('',*,*,#16196,.T.);
#22817=ORIENTED_EDGE('',*,*,#15660,.F.);
#22818=ORIENTED_EDGE('',*,*,#16299,.F.);
#22819=ORIENTED_EDGE('',*,*,#16085,.T.);
#22820=ORIENTED_EDGE('',*,*,#16300,.F.);
#22821=ORIENTED_EDGE('',*,*,#15674,.F.);
#22822=ORIENTED_EDGE('',*,*,#15672,.T.);
#22823=ORIENTED_EDGE('',*,*,#16303,.T.);
#22824=ORIENTED_EDGE('',*,*,#16304,.T.);
#22825=ORIENTED_EDGE('',*,*,#16305,.T.);
#22826=ORIENTED_EDGE('',*,*,#16303,.F.);
#22827=ORIENTED_EDGE('',*,*,#16306,.T.);
#22828=ORIENTED_EDGE('',*,*,#16307,.F.);
#22829=ORIENTED_EDGE('',*,*,#16308,.T.);
#22830=ORIENTED_EDGE('',*,*,#16304,.F.);
#22831=ORIENTED_EDGE('',*,*,#16305,.F.);
#22832=ORIENTED_EDGE('',*,*,#16308,.F.);
#22833=ORIENTED_EDGE('',*,*,#16309,.F.);
#22834=ORIENTED_EDGE('',*,*,#16310,.T.);
#22835=ORIENTED_EDGE('',*,*,#16311,.T.);
#22836=ORIENTED_EDGE('',*,*,#16310,.F.);
#22837=ORIENTED_EDGE('',*,*,#16306,.F.);
#22838=ORIENTED_EDGE('',*,*,#16195,.T.);
#22839=ORIENTED_EDGE('',*,*,#16312,.T.);
#22840=ORIENTED_EDGE('',*,*,#16307,.T.);
#22841=ORIENTED_EDGE('',*,*,#16312,.F.);
#22842=ORIENTED_EDGE('',*,*,#15370,.T.);
#22843=ORIENTED_EDGE('',*,*,#16313,.T.);
#22844=ORIENTED_EDGE('',*,*,#16309,.T.);
#22845=ORIENTED_EDGE('',*,*,#16313,.F.);
#22846=ORIENTED_EDGE('',*,*,#16311,.F.);
#22847=ORIENTED_EDGE('',*,*,#16314,.T.);
#22848=ORIENTED_EDGE('',*,*,#16314,.F.);
#22849=ORIENTED_EDGE('',*,*,#15291,.F.);
#22850=ORIENTED_EDGE('',*,*,#16315,.T.);
#22851=ORIENTED_EDGE('',*,*,#16316,.T.);
#22852=ORIENTED_EDGE('',*,*,#15385,.F.);
#22853=ORIENTED_EDGE('',*,*,#15596,.T.);
#22854=ORIENTED_EDGE('',*,*,#15301,.F.);
#22855=ORIENTED_EDGE('',*,*,#15053,.F.);
#22856=ORIENTED_EDGE('',*,*,#16073,.F.);
#22857=ORIENTED_EDGE('',*,*,#15532,.T.);
#22858=ORIENTED_EDGE('',*,*,#15360,.F.);
#22859=ORIENTED_EDGE('',*,*,#15351,.F.);
#22860=ORIENTED_EDGE('',*,*,#16317,.T.);
#22861=ORIENTED_EDGE('',*,*,#15290,.F.);
#22862=ORIENTED_EDGE('',*,*,#16318,.F.);
#22863=ORIENTED_EDGE('',*,*,#16319,.F.);
#22864=ORIENTED_EDGE('',*,*,#16315,.F.);
#22865=ORIENTED_EDGE('',*,*,#15070,.F.);
#22866=ORIENTED_EDGE('',*,*,#15514,.F.);
#22867=ORIENTED_EDGE('',*,*,#15502,.F.);
#22868=ORIENTED_EDGE('',*,*,#16211,.F.);
#22869=ORIENTED_EDGE('',*,*,#15024,.F.);
#22870=ORIENTED_EDGE('',*,*,#15189,.F.);
#22871=ORIENTED_EDGE('',*,*,#15177,.F.);
#22872=ORIENTED_EDGE('',*,*,#16282,.F.);
#22873=ORIENTED_EDGE('',*,*,#15214,.F.);
#22874=ORIENTED_EDGE('',*,*,#15242,.F.);
#22875=ORIENTED_EDGE('',*,*,#15229,.F.);
#22876=ORIENTED_EDGE('',*,*,#15225,.F.);
#22877=ORIENTED_EDGE('',*,*,#15780,.F.);
#22878=ORIENTED_EDGE('',*,*,#15806,.F.);
#22879=ORIENTED_EDGE('',*,*,#15793,.F.);
#22880=ORIENTED_EDGE('',*,*,#15790,.F.);
#22881=ORIENTED_EDGE('',*,*,#15039,.F.);
#22882=ORIENTED_EDGE('',*,*,#15136,.F.);
#22883=ORIENTED_EDGE('',*,*,#15124,.F.);
#22884=ORIENTED_EDGE('',*,*,#16252,.F.);
#22885=ORIENTED_EDGE('',*,*,#15054,.F.);
#22886=ORIENTED_EDGE('',*,*,#16317,.F.);
#22887=ORIENTED_EDGE('',*,*,#15350,.F.);
#22888=ORIENTED_EDGE('',*,*,#15065,.F.);
#22889=ORIENTED_EDGE('',*,*,#15289,.F.);
#22890=ORIENTED_EDGE('',*,*,#15298,.F.);
#22891=ORIENTED_EDGE('',*,*,#16091,.T.);
#22892=ORIENTED_EDGE('',*,*,#16295,.F.);
#22893=ORIENTED_EDGE('',*,*,#16320,.T.);
#22894=ORIENTED_EDGE('',*,*,#16318,.T.);
#22895=ORIENTED_EDGE('',*,*,#15327,.F.);
#22896=ORIENTED_EDGE('',*,*,#16215,.F.);
#22897=ORIENTED_EDGE('',*,*,#16175,.T.);
#22898=ORIENTED_EDGE('',*,*,#16216,.F.);
#22899=ORIENTED_EDGE('',*,*,#15343,.F.);
#22900=ORIENTED_EDGE('',*,*,#15341,.T.);
#22901=ORIENTED_EDGE('',*,*,#15759,.F.);
#22902=ORIENTED_EDGE('',*,*,#16260,.F.);
#22903=ORIENTED_EDGE('',*,*,#16128,.T.);
#22904=ORIENTED_EDGE('',*,*,#16261,.F.);
#22905=ORIENTED_EDGE('',*,*,#15773,.F.);
#22906=ORIENTED_EDGE('',*,*,#15771,.T.);
#22907=ORIENTED_EDGE('',*,*,#15190,.F.);
#22908=ORIENTED_EDGE('',*,*,#16281,.F.);
#22909=ORIENTED_EDGE('',*,*,#16104,.T.);
#22910=ORIENTED_EDGE('',*,*,#16283,.F.);
#22911=ORIENTED_EDGE('',*,*,#15206,.F.);
#22912=ORIENTED_EDGE('',*,*,#15204,.T.);
#22913=ORIENTED_EDGE('',*,*,#15635,.F.);
#22914=ORIENTED_EDGE('',*,*,#16321,.T.);
#22915=ORIENTED_EDGE('',*,*,#16322,.T.);
#22916=ORIENTED_EDGE('',*,*,#15402,.F.);
#22917=ORIENTED_EDGE('',*,*,#15643,.F.);
#22918=ORIENTED_EDGE('',*,*,#15364,.F.);
#22919=ORIENTED_EDGE('',*,*,#16323,.T.);
#22920=ORIENTED_EDGE('',*,*,#15386,.F.);
#22921=ORIENTED_EDGE('',*,*,#16316,.F.);
#22922=ORIENTED_EDGE('',*,*,#16319,.T.);
#22923=ORIENTED_EDGE('',*,*,#16320,.F.);
#22924=ORIENTED_EDGE('',*,*,#16294,.F.);
#22925=ORIENTED_EDGE('',*,*,#15371,.F.);
#22926=ORIENTED_EDGE('',*,*,#15394,.F.);
#22927=ORIENTED_EDGE('',*,*,#16322,.F.);
#22928=ORIENTED_EDGE('',*,*,#16324,.T.);
#22929=ORIENTED_EDGE('',*,*,#15641,.T.);
#22930=ORIENTED_EDGE('',*,*,#15363,.F.);
#22931=ORIENTED_EDGE('',*,*,#15369,.T.);
#22932=ORIENTED_EDGE('',*,*,#15392,.F.);
#22933=ORIENTED_EDGE('',*,*,#15381,.F.);
#22934=ORIENTED_EDGE('',*,*,#15387,.F.);
#22935=ORIENTED_EDGE('',*,*,#16323,.F.);
#22936=ORIENTED_EDGE('',*,*,#15638,.F.);
#22937=ORIENTED_EDGE('',*,*,#15642,.F.);
#22938=ORIENTED_EDGE('',*,*,#16324,.F.);
#22939=ORIENTED_EDGE('',*,*,#16321,.F.);
#22940=ORIENTED_EDGE('',*,*,#15379,.F.);
#22941=ORIENTED_EDGE('',*,*,#15653,.F.);
#22942=ORIENTED_EDGE('',*,*,#15646,.F.);
#22943=ORIENTED_EDGE('',*,*,#15388,.F.);
#22944=ORIENTED_EDGE('',*,*,#16325,.T.);
#22945=ORIENTED_EDGE('',*,*,#16326,.T.);
#22946=ORIENTED_EDGE('',*,*,#16327,.T.);
#22947=ORIENTED_EDGE('',*,*,#16328,.T.);
#22948=ORIENTED_EDGE('',*,*,#16326,.F.);
#22949=ORIENTED_EDGE('',*,*,#16329,.F.);
#22950=ORIENTED_EDGE('',*,*,#16330,.F.);
#22951=ORIENTED_EDGE('',*,*,#16331,.T.);
#22952=ORIENTED_EDGE('',*,*,#16332,.T.);
#22953=ORIENTED_EDGE('',*,*,#16330,.T.);
#22954=ORIENTED_EDGE('',*,*,#16333,.T.);
#22955=ORIENTED_EDGE('',*,*,#16334,.T.);
#22956=ORIENTED_EDGE('',*,*,#16335,.T.);
#22957=ORIENTED_EDGE('',*,*,#16336,.T.);
#22958=ORIENTED_EDGE('',*,*,#16337,.T.);
#22959=ORIENTED_EDGE('',*,*,#16338,.T.);
#22960=ORIENTED_EDGE('',*,*,#16336,.F.);
#22961=ORIENTED_EDGE('',*,*,#16339,.T.);
#22962=ORIENTED_EDGE('',*,*,#16340,.F.);
#22963=ORIENTED_EDGE('',*,*,#16341,.F.);
#22964=ORIENTED_EDGE('',*,*,#16342,.T.);
#22965=ORIENTED_EDGE('',*,*,#16340,.T.);
#22966=ORIENTED_EDGE('',*,*,#16343,.T.);
#22967=ORIENTED_EDGE('',*,*,#16344,.T.);
#22968=ORIENTED_EDGE('',*,*,#16345,.T.);
#22969=ORIENTED_EDGE('',*,*,#16346,.T.);
#22970=ORIENTED_EDGE('',*,*,#16347,.T.);
#22971=ORIENTED_EDGE('',*,*,#16348,.T.);
#22972=ORIENTED_EDGE('',*,*,#16346,.F.);
#22973=ORIENTED_EDGE('',*,*,#16349,.F.);
#22974=ORIENTED_EDGE('',*,*,#16350,.F.);
#22975=ORIENTED_EDGE('',*,*,#16351,.T.);
#22976=ORIENTED_EDGE('',*,*,#16352,.T.);
#22977=ORIENTED_EDGE('',*,*,#16350,.T.);
#22978=ORIENTED_EDGE('',*,*,#16353,.T.);
#22979=ORIENTED_EDGE('',*,*,#16354,.T.);
#22980=ORIENTED_EDGE('',*,*,#16355,.T.);
#22981=ORIENTED_EDGE('',*,*,#16356,.T.);
#22982=ORIENTED_EDGE('',*,*,#16357,.T.);
#22983=ORIENTED_EDGE('',*,*,#16358,.T.);
#22984=ORIENTED_EDGE('',*,*,#16356,.F.);
#22985=ORIENTED_EDGE('',*,*,#16359,.T.);
#22986=ORIENTED_EDGE('',*,*,#16360,.F.);
#22987=ORIENTED_EDGE('',*,*,#16361,.F.);
#22988=ORIENTED_EDGE('',*,*,#16362,.T.);
#22989=ORIENTED_EDGE('',*,*,#16360,.T.);
#22990=ORIENTED_EDGE('',*,*,#16363,.T.);
#22991=ORIENTED_EDGE('',*,*,#16364,.T.);
#22992=ORIENTED_EDGE('',*,*,#16365,.T.);
#22993=ORIENTED_EDGE('',*,*,#16366,.T.);
#22994=ORIENTED_EDGE('',*,*,#16367,.T.);
#22995=ORIENTED_EDGE('',*,*,#16368,.T.);
#22996=ORIENTED_EDGE('',*,*,#16366,.F.);
#22997=ORIENTED_EDGE('',*,*,#16369,.F.);
#22998=ORIENTED_EDGE('',*,*,#16370,.F.);
#22999=ORIENTED_EDGE('',*,*,#16371,.T.);
#23000=ORIENTED_EDGE('',*,*,#16372,.T.);
#23001=ORIENTED_EDGE('',*,*,#16370,.T.);
#23002=ORIENTED_EDGE('',*,*,#16373,.T.);
#23003=ORIENTED_EDGE('',*,*,#16374,.T.);
#23004=ORIENTED_EDGE('',*,*,#16375,.T.);
#23005=ORIENTED_EDGE('',*,*,#16376,.T.);
#23006=ORIENTED_EDGE('',*,*,#16377,.T.);
#23007=ORIENTED_EDGE('',*,*,#16378,.T.);
#23008=ORIENTED_EDGE('',*,*,#16376,.F.);
#23009=ORIENTED_EDGE('',*,*,#16379,.T.);
#23010=ORIENTED_EDGE('',*,*,#16380,.F.);
#23011=ORIENTED_EDGE('',*,*,#16381,.F.);
#23012=ORIENTED_EDGE('',*,*,#16382,.T.);
#23013=ORIENTED_EDGE('',*,*,#16380,.T.);
#23014=ORIENTED_EDGE('',*,*,#16383,.T.);
#23015=ORIENTED_EDGE('',*,*,#16384,.T.);
#23016=ORIENTED_EDGE('',*,*,#16385,.T.);
#23017=ORIENTED_EDGE('',*,*,#16386,.T.);
#23018=ORIENTED_EDGE('',*,*,#16387,.T.);
#23019=ORIENTED_EDGE('',*,*,#16388,.T.);
#23020=ORIENTED_EDGE('',*,*,#16386,.F.);
#23021=ORIENTED_EDGE('',*,*,#16389,.T.);
#23022=ORIENTED_EDGE('',*,*,#16390,.F.);
#23023=ORIENTED_EDGE('',*,*,#16391,.F.);
#23024=ORIENTED_EDGE('',*,*,#16392,.T.);
#23025=ORIENTED_EDGE('',*,*,#16390,.T.);
#23026=ORIENTED_EDGE('',*,*,#16393,.T.);
#23027=ORIENTED_EDGE('',*,*,#16394,.T.);
#23028=ORIENTED_EDGE('',*,*,#16395,.T.);
#23029=ORIENTED_EDGE('',*,*,#16396,.T.);
#23030=ORIENTED_EDGE('',*,*,#16397,.T.);
#23031=ORIENTED_EDGE('',*,*,#16398,.T.);
#23032=ORIENTED_EDGE('',*,*,#16396,.F.);
#23033=ORIENTED_EDGE('',*,*,#16399,.T.);
#23034=ORIENTED_EDGE('',*,*,#16400,.F.);
#23035=ORIENTED_EDGE('',*,*,#16401,.F.);
#23036=ORIENTED_EDGE('',*,*,#16402,.T.);
#23037=ORIENTED_EDGE('',*,*,#16400,.T.);
#23038=ORIENTED_EDGE('',*,*,#16403,.T.);
#23039=ORIENTED_EDGE('',*,*,#16404,.T.);
#23040=ORIENTED_EDGE('',*,*,#16405,.F.);
#23041=ORIENTED_EDGE('',*,*,#16403,.F.);
#23042=ORIENTED_EDGE('',*,*,#16399,.F.);
#23043=ORIENTED_EDGE('',*,*,#16395,.F.);
#23044=ORIENTED_EDGE('',*,*,#16406,.F.);
#23045=ORIENTED_EDGE('',*,*,#16397,.F.);
#23046=ORIENTED_EDGE('',*,*,#16401,.T.);
#23047=ORIENTED_EDGE('',*,*,#16402,.F.);
#23048=ORIENTED_EDGE('',*,*,#16407,.F.);
#23049=ORIENTED_EDGE('',*,*,#16393,.F.);
#23050=ORIENTED_EDGE('',*,*,#16389,.F.);
#23051=ORIENTED_EDGE('',*,*,#16385,.F.);
#23052=ORIENTED_EDGE('',*,*,#16408,.F.);
#23053=ORIENTED_EDGE('',*,*,#16409,.F.);
#23054=ORIENTED_EDGE('',*,*,#16387,.F.);
#23055=ORIENTED_EDGE('',*,*,#16391,.T.);
#23056=ORIENTED_EDGE('',*,*,#16392,.F.);
#23057=ORIENTED_EDGE('',*,*,#16410,.F.);
#23058=ORIENTED_EDGE('',*,*,#16411,.F.);
#23059=ORIENTED_EDGE('',*,*,#16383,.F.);
#23060=ORIENTED_EDGE('',*,*,#16379,.F.);
#23061=ORIENTED_EDGE('',*,*,#16375,.F.);
#23062=ORIENTED_EDGE('',*,*,#16412,.F.);
#23063=ORIENTED_EDGE('',*,*,#16377,.F.);
#23064=ORIENTED_EDGE('',*,*,#16381,.T.);
#23065=ORIENTED_EDGE('',*,*,#16382,.F.);
#23066=ORIENTED_EDGE('',*,*,#16413,.F.);
#23067=ORIENTED_EDGE('',*,*,#16373,.F.);
#23068=ORIENTED_EDGE('',*,*,#16369,.T.);
#23069=ORIENTED_EDGE('',*,*,#16365,.F.);
#23070=ORIENTED_EDGE('',*,*,#16414,.F.);
#23071=ORIENTED_EDGE('',*,*,#16367,.F.);
#23072=ORIENTED_EDGE('',*,*,#16371,.F.);
#23073=ORIENTED_EDGE('',*,*,#16372,.F.);
#23074=ORIENTED_EDGE('',*,*,#16415,.F.);
#23075=ORIENTED_EDGE('',*,*,#16363,.F.);
#23076=ORIENTED_EDGE('',*,*,#16359,.F.);
#23077=ORIENTED_EDGE('',*,*,#16355,.F.);
#23078=ORIENTED_EDGE('',*,*,#16416,.F.);
#23079=ORIENTED_EDGE('',*,*,#16357,.F.);
#23080=ORIENTED_EDGE('',*,*,#16361,.T.);
#23081=ORIENTED_EDGE('',*,*,#16362,.F.);
#23082=ORIENTED_EDGE('',*,*,#16417,.F.);
#23083=ORIENTED_EDGE('',*,*,#16353,.F.);
#23084=ORIENTED_EDGE('',*,*,#16349,.T.);
#23085=ORIENTED_EDGE('',*,*,#16345,.F.);
#23086=ORIENTED_EDGE('',*,*,#16418,.F.);
#23087=ORIENTED_EDGE('',*,*,#16347,.F.);
#23088=ORIENTED_EDGE('',*,*,#16351,.F.);
#23089=ORIENTED_EDGE('',*,*,#16352,.F.);
#23090=ORIENTED_EDGE('',*,*,#16419,.F.);
#23091=ORIENTED_EDGE('',*,*,#16343,.F.);
#23092=ORIENTED_EDGE('',*,*,#16339,.F.);
#23093=ORIENTED_EDGE('',*,*,#16335,.F.);
#23094=ORIENTED_EDGE('',*,*,#16420,.F.);
#23095=ORIENTED_EDGE('',*,*,#16337,.F.);
#23096=ORIENTED_EDGE('',*,*,#16341,.T.);
#23097=ORIENTED_EDGE('',*,*,#16342,.F.);
#23098=ORIENTED_EDGE('',*,*,#16421,.F.);
#23099=ORIENTED_EDGE('',*,*,#16333,.F.);
#23100=ORIENTED_EDGE('',*,*,#16329,.T.);
#23101=ORIENTED_EDGE('',*,*,#16325,.F.);
#23102=ORIENTED_EDGE('',*,*,#16422,.F.);
#23103=ORIENTED_EDGE('',*,*,#16327,.F.);
#23104=ORIENTED_EDGE('',*,*,#16331,.F.);
#23105=ORIENTED_EDGE('',*,*,#16332,.F.);
#23106=ORIENTED_EDGE('',*,*,#16423,.F.);
#23107=ORIENTED_EDGE('',*,*,#16424,.T.);
#23108=ORIENTED_EDGE('',*,*,#16425,.T.);
#23109=ORIENTED_EDGE('',*,*,#16424,.F.);
#23110=ORIENTED_EDGE('',*,*,#16425,.F.);
#23111=ORIENTED_EDGE('',*,*,#16426,.T.);
#23112=ORIENTED_EDGE('',*,*,#16426,.F.);
#23113=ORIENTED_EDGE('',*,*,#16427,.T.);
#23114=ORIENTED_EDGE('',*,*,#16428,.T.);
#23115=ORIENTED_EDGE('',*,*,#16427,.F.);
#23116=ORIENTED_EDGE('',*,*,#16428,.F.);
#23117=ORIENTED_EDGE('',*,*,#16429,.T.);
#23118=ORIENTED_EDGE('',*,*,#16429,.F.);
#23119=ORIENTED_EDGE('',*,*,#16430,.F.);
#23120=ORIENTED_EDGE('',*,*,#16423,.T.);
#23121=ORIENTED_EDGE('',*,*,#16431,.F.);
#23122=ORIENTED_EDGE('',*,*,#16432,.T.);
#23123=ORIENTED_EDGE('',*,*,#16430,.T.);
#23124=ORIENTED_EDGE('',*,*,#16432,.F.);
#23125=ORIENTED_EDGE('',*,*,#16433,.F.);
#23126=ORIENTED_EDGE('',*,*,#16434,.T.);
#23127=ORIENTED_EDGE('',*,*,#16408,.T.);
#23128=ORIENTED_EDGE('',*,*,#16388,.F.);
#23129=ORIENTED_EDGE('',*,*,#16409,.T.);
#23130=ORIENTED_EDGE('',*,*,#16435,.T.);
#23131=ORIENTED_EDGE('',*,*,#16431,.T.);
#23132=ORIENTED_EDGE('',*,*,#16435,.F.);
#23133=ORIENTED_EDGE('',*,*,#16410,.T.);
#23134=ORIENTED_EDGE('',*,*,#16394,.F.);
#23135=ORIENTED_EDGE('',*,*,#16407,.T.);
#23136=ORIENTED_EDGE('',*,*,#16434,.F.);
#23137=ORIENTED_EDGE('',*,*,#16422,.T.);
#23138=ORIENTED_EDGE('',*,*,#16334,.F.);
#23139=ORIENTED_EDGE('',*,*,#16421,.T.);
#23140=ORIENTED_EDGE('',*,*,#16328,.F.);
#23141=ORIENTED_EDGE('',*,*,#16420,.T.);
#23142=ORIENTED_EDGE('',*,*,#16344,.F.);
#23143=ORIENTED_EDGE('',*,*,#16419,.T.);
#23144=ORIENTED_EDGE('',*,*,#16338,.F.);
#23145=ORIENTED_EDGE('',*,*,#16418,.T.);
#23146=ORIENTED_EDGE('',*,*,#16354,.F.);
#23147=ORIENTED_EDGE('',*,*,#16417,.T.);
#23148=ORIENTED_EDGE('',*,*,#16348,.F.);
#23149=ORIENTED_EDGE('',*,*,#16416,.T.);
#23150=ORIENTED_EDGE('',*,*,#16364,.F.);
#23151=ORIENTED_EDGE('',*,*,#16415,.T.);
#23152=ORIENTED_EDGE('',*,*,#16358,.F.);
#23153=ORIENTED_EDGE('',*,*,#16414,.T.);
#23154=ORIENTED_EDGE('',*,*,#16374,.F.);
#23155=ORIENTED_EDGE('',*,*,#16413,.T.);
#23156=ORIENTED_EDGE('',*,*,#16368,.F.);
#23157=ORIENTED_EDGE('',*,*,#16412,.T.);
#23158=ORIENTED_EDGE('',*,*,#16384,.F.);
#23159=ORIENTED_EDGE('',*,*,#16411,.T.);
#23160=ORIENTED_EDGE('',*,*,#16378,.F.);
#23161=ORIENTED_EDGE('',*,*,#16406,.T.);
#23162=ORIENTED_EDGE('',*,*,#16404,.F.);
#23163=ORIENTED_EDGE('',*,*,#16405,.T.);
#23164=ORIENTED_EDGE('',*,*,#16398,.F.);
#23165=ORIENTED_EDGE('',*,*,#16433,.T.);
#23166=ORIENTED_EDGE('',*,*,#16436,.F.);
#23167=ORIENTED_EDGE('',*,*,#16436,.T.);
#23168=ORIENTED_EDGE('',*,*,#16437,.T.);
#23169=ORIENTED_EDGE('',*,*,#16438,.T.);
#23170=ORIENTED_EDGE('',*,*,#16439,.T.);
#23171=ORIENTED_EDGE('',*,*,#16440,.T.);
#23172=ORIENTED_EDGE('',*,*,#16441,.T.);
#23173=ORIENTED_EDGE('',*,*,#16442,.T.);
#23174=ORIENTED_EDGE('',*,*,#16443,.T.);
#23175=ORIENTED_EDGE('',*,*,#16439,.F.);
#23176=ORIENTED_EDGE('',*,*,#16444,.T.);
#23177=ORIENTED_EDGE('',*,*,#16445,.T.);
#23178=ORIENTED_EDGE('',*,*,#16446,.T.);
#23179=ORIENTED_EDGE('',*,*,#16447,.T.);
#23180=ORIENTED_EDGE('',*,*,#16441,.F.);
#23181=ORIENTED_EDGE('',*,*,#16448,.T.);
#23182=ORIENTED_EDGE('',*,*,#16449,.T.);
#23183=ORIENTED_EDGE('',*,*,#16450,.T.);
#23184=ORIENTED_EDGE('',*,*,#16451,.T.);
#23185=ORIENTED_EDGE('',*,*,#16452,.T.);
#23186=ORIENTED_EDGE('',*,*,#16453,.T.);
#23187=ORIENTED_EDGE('',*,*,#16451,.F.);
#23188=ORIENTED_EDGE('',*,*,#16454,.T.);
#23189=ORIENTED_EDGE('',*,*,#16445,.F.);
#23190=ORIENTED_EDGE('',*,*,#16449,.F.);
#23191=ORIENTED_EDGE('',*,*,#16455,.F.);
#23192=ORIENTED_EDGE('',*,*,#16456,.F.);
#23193=ORIENTED_EDGE('',*,*,#16457,.T.);
#23194=ORIENTED_EDGE('',*,*,#16440,.F.);
#23195=ORIENTED_EDGE('',*,*,#16443,.F.);
#23196=ORIENTED_EDGE('',*,*,#16458,.T.);
#23197=ORIENTED_EDGE('',*,*,#16459,.F.);
#23198=ORIENTED_EDGE('',*,*,#16460,.F.);
#23199=ORIENTED_EDGE('',*,*,#16461,.F.);
#23200=ORIENTED_EDGE('',*,*,#16462,.F.);
#23201=ORIENTED_EDGE('',*,*,#16455,.T.);
#23202=ORIENTED_EDGE('',*,*,#16448,.F.);
#23203=ORIENTED_EDGE('',*,*,#16463,.F.);
#23204=ORIENTED_EDGE('',*,*,#16464,.T.);
#23205=ORIENTED_EDGE('',*,*,#16452,.F.);
#23206=ORIENTED_EDGE('',*,*,#16444,.F.);
#23207=ORIENTED_EDGE('',*,*,#16438,.F.);
#23208=ORIENTED_EDGE('',*,*,#16465,.T.);
#23209=ORIENTED_EDGE('',*,*,#16466,.F.);
#23210=ORIENTED_EDGE('',*,*,#16465,.F.);
#23211=ORIENTED_EDGE('',*,*,#16437,.F.);
#23212=ORIENTED_EDGE('',*,*,#16447,.F.);
#23213=ORIENTED_EDGE('',*,*,#16453,.F.);
#23214=ORIENTED_EDGE('',*,*,#16464,.F.);
#23215=ORIENTED_EDGE('',*,*,#16467,.T.);
#23216=ORIENTED_EDGE('',*,*,#16468,.T.);
#23217=ORIENTED_EDGE('',*,*,#16469,.T.);
#23218=ORIENTED_EDGE('',*,*,#16470,.T.);
#23219=ORIENTED_EDGE('',*,*,#16471,.T.);
#23220=ORIENTED_EDGE('',*,*,#16470,.F.);
#23221=ORIENTED_EDGE('',*,*,#16472,.F.);
#23222=ORIENTED_EDGE('',*,*,#16473,.T.);
#23223=ORIENTED_EDGE('',*,*,#16474,.F.);
#23224=ORIENTED_EDGE('',*,*,#16475,.F.);
#23225=ORIENTED_EDGE('',*,*,#16476,.F.);
#23226=ORIENTED_EDGE('',*,*,#16469,.F.);
#23227=ORIENTED_EDGE('',*,*,#16477,.T.);
#23228=ORIENTED_EDGE('',*,*,#16478,.F.);
#23229=ORIENTED_EDGE('',*,*,#16479,.T.);
#23230=ORIENTED_EDGE('',*,*,#16468,.F.);
#23231=ORIENTED_EDGE('',*,*,#16480,.F.);
#23232=ORIENTED_EDGE('',*,*,#16481,.F.);
#23233=ORIENTED_EDGE('',*,*,#16477,.F.);
#23234=ORIENTED_EDGE('',*,*,#16482,.T.);
#23235=ORIENTED_EDGE('',*,*,#16483,.T.);
#23236=ORIENTED_EDGE('',*,*,#16484,.T.);
#23237=ORIENTED_EDGE('',*,*,#16485,.T.);
#23238=ORIENTED_EDGE('',*,*,#16486,.T.);
#23239=ORIENTED_EDGE('',*,*,#16482,.F.);
#23240=ORIENTED_EDGE('',*,*,#16487,.T.);
#23241=ORIENTED_EDGE('',*,*,#16488,.T.);
#23242=ORIENTED_EDGE('',*,*,#16489,.T.);
#23243=ORIENTED_EDGE('',*,*,#16486,.F.);
#23244=ORIENTED_EDGE('',*,*,#16490,.F.);
#23245=ORIENTED_EDGE('',*,*,#16491,.F.);
#23246=ORIENTED_EDGE('',*,*,#16492,.F.);
#23247=ORIENTED_EDGE('',*,*,#16493,.F.);
#23248=ORIENTED_EDGE('',*,*,#16494,.F.);
#23249=ORIENTED_EDGE('',*,*,#16485,.F.);
#23250=ORIENTED_EDGE('',*,*,#16495,.T.);
#23251=ORIENTED_EDGE('',*,*,#16496,.T.);
#23252=ORIENTED_EDGE('',*,*,#16497,.T.);
#23253=ORIENTED_EDGE('',*,*,#16490,.T.);
#23254=ORIENTED_EDGE('',*,*,#16498,.F.);
#23255=ORIENTED_EDGE('',*,*,#16499,.F.);
#23256=ORIENTED_EDGE('',*,*,#16500,.F.);
#23257=ORIENTED_EDGE('',*,*,#16501,.T.);
#23258=ORIENTED_EDGE('',*,*,#16499,.T.);
#23259=ORIENTED_EDGE('',*,*,#16475,.T.);
#23260=ORIENTED_EDGE('',*,*,#16502,.T.);
#23261=ORIENTED_EDGE('',*,*,#16503,.F.);
#23262=ORIENTED_EDGE('',*,*,#16497,.F.);
#23263=ORIENTED_EDGE('',*,*,#16504,.F.);
#23264=ORIENTED_EDGE('',*,*,#16505,.T.);
#23265=ORIENTED_EDGE('',*,*,#16506,.T.);
#23266=ORIENTED_EDGE('',*,*,#16507,.T.);
#23267=ORIENTED_EDGE('',*,*,#16508,.T.);
#23268=ORIENTED_EDGE('',*,*,#16509,.T.);
#23269=ORIENTED_EDGE('',*,*,#16504,.T.);
#23270=ORIENTED_EDGE('',*,*,#16510,.T.);
#23271=ORIENTED_EDGE('',*,*,#16506,.F.);
#23272=ORIENTED_EDGE('',*,*,#16491,.T.);
#23273=ORIENTED_EDGE('',*,*,#16503,.T.);
#23274=ORIENTED_EDGE('',*,*,#16511,.T.);
#23275=ORIENTED_EDGE('',*,*,#16512,.T.);
#23276=ORIENTED_EDGE('',*,*,#16513,.T.);
#23277=ORIENTED_EDGE('',*,*,#16508,.F.);
#23278=ORIENTED_EDGE('',*,*,#16514,.T.);
#23279=ORIENTED_EDGE('',*,*,#16515,.T.);
#23280=ORIENTED_EDGE('',*,*,#16516,.T.);
#23281=ORIENTED_EDGE('',*,*,#16517,.T.);
#23282=ORIENTED_EDGE('',*,*,#16492,.T.);
#23283=ORIENTED_EDGE('',*,*,#16512,.F.);
#23284=ORIENTED_EDGE('',*,*,#16518,.T.);
#23285=ORIENTED_EDGE('',*,*,#16519,.T.);
#23286=ORIENTED_EDGE('',*,*,#16517,.F.);
#23287=ORIENTED_EDGE('',*,*,#16520,.T.);
#23288=ORIENTED_EDGE('',*,*,#16474,.T.);
#23289=ORIENTED_EDGE('',*,*,#16518,.F.);
#23290=ORIENTED_EDGE('',*,*,#16521,.T.);
#23291=ORIENTED_EDGE('',*,*,#16502,.F.);
#23292=ORIENTED_EDGE('',*,*,#16522,.T.);
#23293=ORIENTED_EDGE('',*,*,#16515,.F.);
#23294=ORIENTED_EDGE('',*,*,#16523,.T.);
#23295=ORIENTED_EDGE('',*,*,#16524,.T.);
#23296=ORIENTED_EDGE('',*,*,#16525,.T.);
#23297=ORIENTED_EDGE('',*,*,#16500,.T.);
#23298=ORIENTED_EDGE('',*,*,#16526,.T.);
#23299=ORIENTED_EDGE('',*,*,#16524,.F.);
#23300=ORIENTED_EDGE('',*,*,#16471,.F.);
#23301=ORIENTED_EDGE('',*,*,#16476,.T.);
#23302=ORIENTED_EDGE('',*,*,#16498,.T.);
#23303=ORIENTED_EDGE('',*,*,#16527,.T.);
#23304=ORIENTED_EDGE('',*,*,#16528,.T.);
#23305=ORIENTED_EDGE('',*,*,#16467,.F.);
#23306=ORIENTED_EDGE('',*,*,#16528,.F.);
#23307=ORIENTED_EDGE('',*,*,#16529,.T.);
#23308=ORIENTED_EDGE('',*,*,#16530,.T.);
#23309=ORIENTED_EDGE('',*,*,#16480,.T.);
#23310=ORIENTED_EDGE('',*,*,#16527,.F.);
#23311=ORIENTED_EDGE('',*,*,#16525,.F.);
#23312=ORIENTED_EDGE('',*,*,#16523,.F.);
#23313=ORIENTED_EDGE('',*,*,#16514,.F.);
#23314=ORIENTED_EDGE('',*,*,#16507,.F.);
#23315=ORIENTED_EDGE('',*,*,#16510,.F.);
#23316=ORIENTED_EDGE('',*,*,#16496,.F.);
#23317=ORIENTED_EDGE('',*,*,#16531,.F.);
#23318=ORIENTED_EDGE('',*,*,#16532,.F.);
#23319=ORIENTED_EDGE('',*,*,#16533,.F.);
#23320=ORIENTED_EDGE('',*,*,#16534,.F.);
#23321=ORIENTED_EDGE('',*,*,#16535,.F.);
#23322=ORIENTED_EDGE('',*,*,#16536,.F.);
#23323=ORIENTED_EDGE('',*,*,#16537,.F.);
#23324=ORIENTED_EDGE('',*,*,#16538,.F.);
#23325=ORIENTED_EDGE('',*,*,#16529,.F.);
#23326=ORIENTED_EDGE('',*,*,#16539,.F.);
#23327=ORIENTED_EDGE('',*,*,#16540,.F.);
#23328=ORIENTED_EDGE('',*,*,#16541,.F.);
#23329=ORIENTED_EDGE('',*,*,#16542,.F.);
#23330=ORIENTED_EDGE('',*,*,#16521,.F.);
#23331=ORIENTED_EDGE('',*,*,#16520,.F.);
#23332=ORIENTED_EDGE('',*,*,#16516,.F.);
#23333=ORIENTED_EDGE('',*,*,#16543,.F.);
#23334=ORIENTED_EDGE('',*,*,#16544,.F.);
#23335=ORIENTED_EDGE('',*,*,#16545,.F.);
#23336=ORIENTED_EDGE('',*,*,#16546,.F.);
#23337=ORIENTED_EDGE('',*,*,#16547,.F.);
#23338=ORIENTED_EDGE('',*,*,#16548,.F.);
#23339=ORIENTED_EDGE('',*,*,#16511,.F.);
#23340=ORIENTED_EDGE('',*,*,#16509,.F.);
#23341=ORIENTED_EDGE('',*,*,#16549,.T.);
#23342=ORIENTED_EDGE('',*,*,#16543,.T.);
#23343=ORIENTED_EDGE('',*,*,#16505,.F.);
#23344=ORIENTED_EDGE('',*,*,#16550,.T.);
#23345=ORIENTED_EDGE('',*,*,#16544,.T.);
#23346=ORIENTED_EDGE('',*,*,#16549,.F.);
#23347=ORIENTED_EDGE('',*,*,#16551,.T.);
#23348=ORIENTED_EDGE('',*,*,#16552,.T.);
#23349=ORIENTED_EDGE('',*,*,#16553,.T.);
#23350=ORIENTED_EDGE('',*,*,#16552,.F.);
#23351=ORIENTED_EDGE('',*,*,#16554,.F.);
#23352=ORIENTED_EDGE('',*,*,#16555,.T.);
#23353=ORIENTED_EDGE('',*,*,#16551,.F.);
#23354=ORIENTED_EDGE('',*,*,#16555,.F.);
#23355=ORIENTED_EDGE('',*,*,#16556,.T.);
#23356=ORIENTED_EDGE('',*,*,#16553,.F.);
#23357=ORIENTED_EDGE('',*,*,#16539,.T.);
#23358=ORIENTED_EDGE('',*,*,#16557,.T.);
#23359=ORIENTED_EDGE('',*,*,#16554,.T.);
#23360=ORIENTED_EDGE('',*,*,#16557,.F.);
#23361=ORIENTED_EDGE('',*,*,#16558,.T.);
#23362=ORIENTED_EDGE('',*,*,#16559,.T.);
#23363=ORIENTED_EDGE('',*,*,#16560,.T.);
#23364=ORIENTED_EDGE('',*,*,#16559,.F.);
#23365=ORIENTED_EDGE('',*,*,#16561,.F.);
#23366=ORIENTED_EDGE('',*,*,#16562,.T.);
#23367=ORIENTED_EDGE('',*,*,#16558,.F.);
#23368=ORIENTED_EDGE('',*,*,#16562,.F.);
#23369=ORIENTED_EDGE('',*,*,#16563,.T.);
#23370=ORIENTED_EDGE('',*,*,#16560,.F.);
#23371=ORIENTED_EDGE('',*,*,#16542,.T.);
#23372=ORIENTED_EDGE('',*,*,#16564,.T.);
#23373=ORIENTED_EDGE('',*,*,#16561,.T.);
#23374=ORIENTED_EDGE('',*,*,#16564,.F.);
#23375=ORIENTED_EDGE('',*,*,#16540,.T.);
#23376=ORIENTED_EDGE('',*,*,#16565,.T.);
#23377=ORIENTED_EDGE('',*,*,#16566,.T.);
#23378=ORIENTED_EDGE('',*,*,#16565,.F.);
#23379=ORIENTED_EDGE('',*,*,#16566,.F.);
#23380=ORIENTED_EDGE('',*,*,#16567,.T.);
#23381=ORIENTED_EDGE('',*,*,#16568,.T.);
#23382=ORIENTED_EDGE('',*,*,#16567,.F.);
#23383=ORIENTED_EDGE('',*,*,#16541,.T.);
#23384=ORIENTED_EDGE('',*,*,#16569,.T.);
#23385=ORIENTED_EDGE('',*,*,#16570,.T.);
#23386=ORIENTED_EDGE('',*,*,#16569,.F.);
#23387=ORIENTED_EDGE('',*,*,#16570,.F.);
#23388=ORIENTED_EDGE('',*,*,#16571,.T.);
#23389=ORIENTED_EDGE('',*,*,#16572,.T.);
#23390=ORIENTED_EDGE('',*,*,#16571,.F.);
#23391=ORIENTED_EDGE('',*,*,#16573,.F.);
#23392=ORIENTED_EDGE('',*,*,#16574,.F.);
#23393=ORIENTED_EDGE('',*,*,#16575,.F.);
#23394=ORIENTED_EDGE('',*,*,#16576,.F.);
#23395=ORIENTED_EDGE('',*,*,#16577,.F.);
#23396=ORIENTED_EDGE('',*,*,#16578,.F.);
#23397=ORIENTED_EDGE('',*,*,#16574,.T.);
#23398=ORIENTED_EDGE('',*,*,#16579,.T.);
#23399=ORIENTED_EDGE('',*,*,#16577,.T.);
#23400=ORIENTED_EDGE('',*,*,#16580,.T.);
#23401=ORIENTED_EDGE('',*,*,#16581,.T.);
#23402=ORIENTED_EDGE('',*,*,#16582,.T.);
#23403=ORIENTED_EDGE('',*,*,#16578,.T.);
#23404=ORIENTED_EDGE('',*,*,#16583,.T.);
#23405=ORIENTED_EDGE('',*,*,#16584,.T.);
#23406=ORIENTED_EDGE('',*,*,#16585,.T.);
#23407=ORIENTED_EDGE('',*,*,#16576,.T.);
#23408=ORIENTED_EDGE('',*,*,#16586,.T.);
#23409=ORIENTED_EDGE('',*,*,#16587,.T.);
#23410=ORIENTED_EDGE('',*,*,#16588,.T.);
#23411=ORIENTED_EDGE('',*,*,#16575,.T.);
#23412=ORIENTED_EDGE('',*,*,#16589,.T.);
#23413=ORIENTED_EDGE('',*,*,#16590,.T.);
#23414=ORIENTED_EDGE('',*,*,#16591,.T.);
#23415=ORIENTED_EDGE('',*,*,#16573,.T.);
#23416=ORIENTED_EDGE('',*,*,#16592,.T.);
#23417=ORIENTED_EDGE('',*,*,#16586,.F.);
#23418=ORIENTED_EDGE('',*,*,#16582,.F.);
#23419=ORIENTED_EDGE('',*,*,#16593,.F.);
#23420=ORIENTED_EDGE('',*,*,#16594,.F.);
#23421=ORIENTED_EDGE('',*,*,#16595,.T.);
#23422=ORIENTED_EDGE('',*,*,#16596,.T.);
#23423=ORIENTED_EDGE('',*,*,#16597,.F.);
#23424=ORIENTED_EDGE('',*,*,#16583,.F.);
#23425=ORIENTED_EDGE('',*,*,#16579,.F.);
#23426=ORIENTED_EDGE('',*,*,#16591,.F.);
#23427=ORIENTED_EDGE('',*,*,#16598,.F.);
#23428=ORIENTED_EDGE('',*,*,#16599,.T.);
#23429=ORIENTED_EDGE('',*,*,#16600,.F.);
#23430=ORIENTED_EDGE('',*,*,#16601,.T.);
#23431=ORIENTED_EDGE('',*,*,#16602,.T.);
#23432=ORIENTED_EDGE('',*,*,#16603,.T.);
#23433=ORIENTED_EDGE('',*,*,#16604,.T.);
#23434=ORIENTED_EDGE('',*,*,#16605,.T.);
#23435=ORIENTED_EDGE('',*,*,#16606,.T.);
#23436=ORIENTED_EDGE('',*,*,#16607,.T.);
#23437=ORIENTED_EDGE('',*,*,#16608,.F.);
#23438=ORIENTED_EDGE('',*,*,#16609,.T.);
#23439=ORIENTED_EDGE('',*,*,#16610,.T.);
#23440=ORIENTED_EDGE('',*,*,#16611,.T.);
#23441=ORIENTED_EDGE('',*,*,#16610,.F.);
#23442=ORIENTED_EDGE('',*,*,#16612,.T.);
#23443=ORIENTED_EDGE('',*,*,#16604,.F.);
#23444=ORIENTED_EDGE('',*,*,#16602,.F.);
#23445=ORIENTED_EDGE('',*,*,#16613,.F.);
#23446=ORIENTED_EDGE('',*,*,#16614,.F.);
#23447=ORIENTED_EDGE('',*,*,#16615,.F.);
#23448=ORIENTED_EDGE('',*,*,#16616,.F.);
#23449=ORIENTED_EDGE('',*,*,#16617,.F.);
#23450=ORIENTED_EDGE('',*,*,#16618,.F.);
#23451=ORIENTED_EDGE('',*,*,#16619,.F.);
#23452=ORIENTED_EDGE('',*,*,#16620,.F.);
#23453=ORIENTED_EDGE('',*,*,#16621,.F.);
#23454=ORIENTED_EDGE('',*,*,#16622,.T.);
#23455=ORIENTED_EDGE('',*,*,#16605,.F.);
#23456=ORIENTED_EDGE('',*,*,#16623,.F.);
#23457=ORIENTED_EDGE('',*,*,#16624,.F.);
#23458=ORIENTED_EDGE('',*,*,#16625,.T.);
#23459=ORIENTED_EDGE('',*,*,#16626,.T.);
#23460=ORIENTED_EDGE('',*,*,#16613,.T.);
#23461=ORIENTED_EDGE('',*,*,#16612,.F.);
#23462=ORIENTED_EDGE('',*,*,#16627,.T.);
#23463=ORIENTED_EDGE('',*,*,#16628,.T.);
#23464=ORIENTED_EDGE('',*,*,#16623,.T.);
#23465=ORIENTED_EDGE('',*,*,#16609,.F.);
#23466=ORIENTED_EDGE('',*,*,#16629,.F.);
#23467=ORIENTED_EDGE('',*,*,#16630,.F.);
#23468=ORIENTED_EDGE('',*,*,#16631,.F.);
#23469=ORIENTED_EDGE('',*,*,#16632,.F.);
#23470=ORIENTED_EDGE('',*,*,#16633,.F.);
#23471=ORIENTED_EDGE('',*,*,#16634,.F.);
#23472=ORIENTED_EDGE('',*,*,#16627,.F.);
#23473=ORIENTED_EDGE('',*,*,#16635,.F.);
#23474=ORIENTED_EDGE('',*,*,#16636,.F.);
#23475=ORIENTED_EDGE('',*,*,#16637,.T.);
#23476=ORIENTED_EDGE('',*,*,#16638,.F.);
#23477=ORIENTED_EDGE('',*,*,#16639,.F.);
#23478=ORIENTED_EDGE('',*,*,#16640,.T.);
#23479=ORIENTED_EDGE('',*,*,#16641,.T.);
#23480=ORIENTED_EDGE('',*,*,#16632,.T.);
#23481=ORIENTED_EDGE('',*,*,#16642,.T.);
#23482=ORIENTED_EDGE('',*,*,#16643,.F.);
#23483=ORIENTED_EDGE('',*,*,#16644,.T.);
#23484=ORIENTED_EDGE('',*,*,#16645,.T.);
#23485=ORIENTED_EDGE('',*,*,#16646,.T.);
#23486=ORIENTED_EDGE('',*,*,#16647,.T.);
#23487=ORIENTED_EDGE('',*,*,#16646,.F.);
#23488=ORIENTED_EDGE('',*,*,#16648,.T.);
#23489=ORIENTED_EDGE('',*,*,#16641,.F.);
#23490=ORIENTED_EDGE('',*,*,#16648,.F.);
#23491=ORIENTED_EDGE('',*,*,#16649,.T.);
#23492=ORIENTED_EDGE('',*,*,#16650,.F.);
#23493=ORIENTED_EDGE('',*,*,#16633,.T.);
#23494=ORIENTED_EDGE('',*,*,#16645,.F.);
#23495=ORIENTED_EDGE('',*,*,#16651,.T.);
#23496=ORIENTED_EDGE('',*,*,#16652,.T.);
#23497=ORIENTED_EDGE('',*,*,#16653,.T.);
#23498=ORIENTED_EDGE('',*,*,#16654,.F.);
#23499=ORIENTED_EDGE('',*,*,#16649,.F.);
#23500=ORIENTED_EDGE('',*,*,#16644,.F.);
#23501=ORIENTED_EDGE('',*,*,#16655,.T.);
#23502=ORIENTED_EDGE('',*,*,#16656,.F.);
#23503=ORIENTED_EDGE('',*,*,#16657,.F.);
#23504=ORIENTED_EDGE('',*,*,#16658,.F.);
#23505=ORIENTED_EDGE('',*,*,#16659,.F.);
#23506=ORIENTED_EDGE('',*,*,#16660,.F.);
#23507=ORIENTED_EDGE('',*,*,#16661,.F.);
#23508=ORIENTED_EDGE('',*,*,#16662,.F.);
#23509=ORIENTED_EDGE('',*,*,#16663,.F.);
#23510=ORIENTED_EDGE('',*,*,#16651,.F.);
#23511=ORIENTED_EDGE('',*,*,#16664,.T.);
#23512=ORIENTED_EDGE('',*,*,#16665,.T.);
#23513=ORIENTED_EDGE('',*,*,#16666,.T.);
#23514=ORIENTED_EDGE('',*,*,#16638,.T.);
#23515=ORIENTED_EDGE('',*,*,#16665,.F.);
#23516=ORIENTED_EDGE('',*,*,#16667,.F.);
#23517=ORIENTED_EDGE('',*,*,#16668,.F.);
#23518=ORIENTED_EDGE('',*,*,#16669,.F.);
#23519=ORIENTED_EDGE('',*,*,#16670,.T.);
#23520=ORIENTED_EDGE('',*,*,#16671,.F.);
#23521=ORIENTED_EDGE('',*,*,#16672,.T.);
#23522=ORIENTED_EDGE('',*,*,#16673,.T.);
#23523=ORIENTED_EDGE('',*,*,#16674,.T.);
#23524=ORIENTED_EDGE('',*,*,#16675,.T.);
#23525=ORIENTED_EDGE('',*,*,#16673,.F.);
#23526=ORIENTED_EDGE('',*,*,#16676,.F.);
#23527=ORIENTED_EDGE('',*,*,#16677,.F.);
#23528=ORIENTED_EDGE('',*,*,#16678,.F.);
#23529=ORIENTED_EDGE('',*,*,#16679,.F.);
#23530=ORIENTED_EDGE('',*,*,#16680,.F.);
#23531=ORIENTED_EDGE('',*,*,#16630,.T.);
#23532=ORIENTED_EDGE('',*,*,#16681,.F.);
#23533=ORIENTED_EDGE('',*,*,#16682,.F.);
#23534=ORIENTED_EDGE('',*,*,#16683,.F.);
#23535=ORIENTED_EDGE('',*,*,#16684,.F.);
#23536=ORIENTED_EDGE('',*,*,#16685,.F.);
#23537=ORIENTED_EDGE('',*,*,#16686,.F.);
#23538=ORIENTED_EDGE('',*,*,#16687,.F.);
#23539=ORIENTED_EDGE('',*,*,#16672,.F.);
#23540=ORIENTED_EDGE('',*,*,#16688,.F.);
#23541=ORIENTED_EDGE('',*,*,#16689,.T.);
#23542=ORIENTED_EDGE('',*,*,#16674,.F.);
#23543=ORIENTED_EDGE('',*,*,#16675,.F.);
#23544=ORIENTED_EDGE('',*,*,#16689,.F.);
#23545=ORIENTED_EDGE('',*,*,#16686,.T.);
#23546=ORIENTED_EDGE('',*,*,#16690,.T.);
#23547=ORIENTED_EDGE('',*,*,#16691,.T.);
#23548=ORIENTED_EDGE('',*,*,#16692,.T.);
#23549=ORIENTED_EDGE('',*,*,#16690,.F.);
#23550=ORIENTED_EDGE('',*,*,#16693,.F.);
#23551=ORIENTED_EDGE('',*,*,#16694,.T.);
#23552=ORIENTED_EDGE('',*,*,#16691,.F.);
#23553=ORIENTED_EDGE('',*,*,#16692,.F.);
#23554=ORIENTED_EDGE('',*,*,#16694,.F.);
#23555=ORIENTED_EDGE('',*,*,#16687,.T.);
#23556=ORIENTED_EDGE('',*,*,#16695,.T.);
#23557=ORIENTED_EDGE('',*,*,#16696,.T.);
#23558=ORIENTED_EDGE('',*,*,#16697,.T.);
#23559=ORIENTED_EDGE('',*,*,#16695,.F.);
#23560=ORIENTED_EDGE('',*,*,#16698,.F.);
#23561=ORIENTED_EDGE('',*,*,#16699,.T.);
#23562=ORIENTED_EDGE('',*,*,#16696,.F.);
#23563=ORIENTED_EDGE('',*,*,#16697,.F.);
#23564=ORIENTED_EDGE('',*,*,#16699,.F.);
#23565=ORIENTED_EDGE('',*,*,#16700,.T.);
#23566=ORIENTED_EDGE('',*,*,#16676,.T.);
#23567=ORIENTED_EDGE('',*,*,#16701,.T.);
#23568=ORIENTED_EDGE('',*,*,#16702,.T.);
#23569=ORIENTED_EDGE('',*,*,#16703,.T.);
#23570=ORIENTED_EDGE('',*,*,#16701,.F.);
#23571=ORIENTED_EDGE('',*,*,#16685,.T.);
#23572=ORIENTED_EDGE('',*,*,#16700,.F.);
#23573=ORIENTED_EDGE('',*,*,#16684,.T.);
#23574=ORIENTED_EDGE('',*,*,#16704,.F.);
#23575=ORIENTED_EDGE('',*,*,#16705,.F.);
#23576=ORIENTED_EDGE('',*,*,#16706,.F.);
#23577=ORIENTED_EDGE('',*,*,#16707,.F.);
#23578=ORIENTED_EDGE('',*,*,#16708,.F.);
#23579=ORIENTED_EDGE('',*,*,#16709,.F.);
#23580=ORIENTED_EDGE('',*,*,#16710,.F.);
#23581=ORIENTED_EDGE('',*,*,#16677,.T.);
#23582=ORIENTED_EDGE('',*,*,#16711,.F.);
#23583=ORIENTED_EDGE('',*,*,#16712,.T.);
#23584=ORIENTED_EDGE('',*,*,#16702,.F.);
#23585=ORIENTED_EDGE('',*,*,#16703,.F.);
#23586=ORIENTED_EDGE('',*,*,#16712,.F.);
#23587=ORIENTED_EDGE('',*,*,#16713,.F.);
#23588=ORIENTED_EDGE('',*,*,#16636,.T.);
#23589=ORIENTED_EDGE('',*,*,#16714,.T.);
#23590=ORIENTED_EDGE('',*,*,#16715,.T.);
#23591=ORIENTED_EDGE('',*,*,#16716,.T.);
#23592=ORIENTED_EDGE('',*,*,#16717,.F.);
#23593=ORIENTED_EDGE('',*,*,#16716,.F.);
#23594=ORIENTED_EDGE('',*,*,#16718,.F.);
#23595=ORIENTED_EDGE('',*,*,#16719,.T.);
#23596=ORIENTED_EDGE('',*,*,#16720,.F.);
#23597=ORIENTED_EDGE('',*,*,#16721,.F.);
#23598=ORIENTED_EDGE('',*,*,#16722,.F.);
#23599=ORIENTED_EDGE('',*,*,#16460,.T.);
#23600=ORIENTED_EDGE('',*,*,#16723,.T.);
#23601=ORIENTED_EDGE('',*,*,#16724,.T.);
#23602=ORIENTED_EDGE('',*,*,#16725,.T.);
#23603=ORIENTED_EDGE('',*,*,#16726,.F.);
#23604=ORIENTED_EDGE('',*,*,#16727,.F.);
#23605=ORIENTED_EDGE('',*,*,#16728,.F.);
#23606=ORIENTED_EDGE('',*,*,#16729,.F.);
#23607=ORIENTED_EDGE('',*,*,#16548,.T.);
#23608=ORIENTED_EDGE('',*,*,#16730,.T.);
#23609=ORIENTED_EDGE('',*,*,#16731,.T.);
#23610=ORIENTED_EDGE('',*,*,#16730,.F.);
#23611=ORIENTED_EDGE('',*,*,#16731,.F.);
#23612=ORIENTED_EDGE('',*,*,#16732,.T.);
#23613=ORIENTED_EDGE('',*,*,#16733,.F.);
#23614=ORIENTED_EDGE('',*,*,#16734,.F.);
#23615=ORIENTED_EDGE('',*,*,#16732,.F.);
#23616=ORIENTED_EDGE('',*,*,#16735,.T.);
#23617=ORIENTED_EDGE('',*,*,#16736,.T.);
#23618=ORIENTED_EDGE('',*,*,#16737,.T.);
#23619=ORIENTED_EDGE('',*,*,#16738,.T.);
#23620=ORIENTED_EDGE('',*,*,#16738,.F.);
#23621=ORIENTED_EDGE('',*,*,#16739,.F.);
#23622=ORIENTED_EDGE('',*,*,#16740,.F.);
#23623=ORIENTED_EDGE('',*,*,#16741,.F.);
#23624=ORIENTED_EDGE('',*,*,#16737,.F.);
#23625=ORIENTED_EDGE('',*,*,#16742,.F.);
#23626=ORIENTED_EDGE('',*,*,#16743,.F.);
#23627=ORIENTED_EDGE('',*,*,#16744,.F.);
#23628=ORIENTED_EDGE('',*,*,#16745,.T.);
#23629=ORIENTED_EDGE('',*,*,#16746,.T.);
#23630=ORIENTED_EDGE('',*,*,#16747,.T.);
#23631=ORIENTED_EDGE('',*,*,#16740,.T.);
#23632=ORIENTED_EDGE('',*,*,#16746,.F.);
#23633=ORIENTED_EDGE('',*,*,#16748,.T.);
#23634=ORIENTED_EDGE('',*,*,#16749,.T.);
#23635=ORIENTED_EDGE('',*,*,#16750,.T.);
#23636=ORIENTED_EDGE('',*,*,#16745,.F.);
#23637=ORIENTED_EDGE('',*,*,#16751,.F.);
#23638=ORIENTED_EDGE('',*,*,#16752,.F.);
#23639=ORIENTED_EDGE('',*,*,#16748,.F.);
#23640=ORIENTED_EDGE('',*,*,#16753,.T.);
#23641=ORIENTED_EDGE('',*,*,#16754,.T.);
#23642=ORIENTED_EDGE('',*,*,#16733,.T.);
#23643=ORIENTED_EDGE('',*,*,#16734,.T.);
#23644=ORIENTED_EDGE('',*,*,#16754,.F.);
#23645=ORIENTED_EDGE('',*,*,#16487,.F.);
#23646=ORIENTED_EDGE('',*,*,#16494,.T.);
#23647=ORIENTED_EDGE('',*,*,#16755,.T.);
#23648=ORIENTED_EDGE('',*,*,#16472,.T.);
#23649=ORIENTED_EDGE('',*,*,#16479,.F.);
#23650=ORIENTED_EDGE('',*,*,#16756,.F.);
#23651=ORIENTED_EDGE('',*,*,#16757,.F.);
#23652=ORIENTED_EDGE('',*,*,#16758,.F.);
#23653=ORIENTED_EDGE('',*,*,#16759,.F.);
#23654=ORIENTED_EDGE('',*,*,#16760,.F.);
#23655=ORIENTED_EDGE('',*,*,#16761,.F.);
#23656=ORIENTED_EDGE('',*,*,#16762,.F.);
#23657=ORIENTED_EDGE('',*,*,#16763,.T.);
#23658=ORIENTED_EDGE('',*,*,#16764,.T.);
#23659=ORIENTED_EDGE('',*,*,#16765,.T.);
#23660=ORIENTED_EDGE('',*,*,#16766,.T.);
#23661=ORIENTED_EDGE('',*,*,#16767,.F.);
#23662=ORIENTED_EDGE('',*,*,#16768,.F.);
#23663=ORIENTED_EDGE('',*,*,#16769,.T.);
#23664=ORIENTED_EDGE('',*,*,#16770,.T.);
#23665=ORIENTED_EDGE('',*,*,#16771,.F.);
#23666=ORIENTED_EDGE('',*,*,#16772,.T.);
#23667=ORIENTED_EDGE('',*,*,#16773,.T.);
#23668=ORIENTED_EDGE('',*,*,#16774,.F.);
#23669=ORIENTED_EDGE('',*,*,#16775,.F.);
#23670=ORIENTED_EDGE('',*,*,#16776,.T.);
#23671=ORIENTED_EDGE('',*,*,#16771,.T.);
#23672=ORIENTED_EDGE('',*,*,#16777,.T.);
#23673=ORIENTED_EDGE('',*,*,#16753,.F.);
#23674=ORIENTED_EDGE('',*,*,#16461,.T.);
#23675=ORIENTED_EDGE('',*,*,#16722,.T.);
#23676=ORIENTED_EDGE('',*,*,#16778,.F.);
#23677=ORIENTED_EDGE('',*,*,#16779,.F.);
#23678=ORIENTED_EDGE('',*,*,#16707,.T.);
#23679=ORIENTED_EDGE('',*,*,#16780,.T.);
#23680=ORIENTED_EDGE('',*,*,#16726,.T.);
#23681=ORIENTED_EDGE('',*,*,#16781,.T.);
#23682=ORIENTED_EDGE('',*,*,#16711,.T.);
#23683=ORIENTED_EDGE('',*,*,#16781,.F.);
#23684=ORIENTED_EDGE('',*,*,#16729,.T.);
#23685=ORIENTED_EDGE('',*,*,#16782,.T.);
#23686=ORIENTED_EDGE('',*,*,#16698,.T.);
#23687=ORIENTED_EDGE('',*,*,#16782,.F.);
#23688=ORIENTED_EDGE('',*,*,#16727,.T.);
#23689=ORIENTED_EDGE('',*,*,#16783,.T.);
#23690=ORIENTED_EDGE('',*,*,#16693,.T.);
#23691=ORIENTED_EDGE('',*,*,#16783,.F.);
#23692=ORIENTED_EDGE('',*,*,#16728,.T.);
#23693=ORIENTED_EDGE('',*,*,#16784,.T.);
#23694=ORIENTED_EDGE('',*,*,#16688,.T.);
#23695=ORIENTED_EDGE('',*,*,#16784,.F.);
#23696=ORIENTED_EDGE('',*,*,#16785,.T.);
#23697=ORIENTED_EDGE('',*,*,#16786,.T.);
#23698=ORIENTED_EDGE('',*,*,#16787,.T.);
#23699=ORIENTED_EDGE('',*,*,#16788,.T.);
#23700=ORIENTED_EDGE('',*,*,#16789,.T.);
#23701=ORIENTED_EDGE('',*,*,#16790,.T.);
#23702=ORIENTED_EDGE('',*,*,#16791,.T.);
#23703=ORIENTED_EDGE('',*,*,#16792,.T.);
#23704=ORIENTED_EDGE('',*,*,#16785,.F.);
#23705=ORIENTED_EDGE('',*,*,#16793,.T.);
#23706=ORIENTED_EDGE('',*,*,#16624,.T.);
#23707=ORIENTED_EDGE('',*,*,#16628,.F.);
#23708=ORIENTED_EDGE('',*,*,#16794,.T.);
#23709=ORIENTED_EDGE('',*,*,#16792,.F.);
#23710=ORIENTED_EDGE('',*,*,#16795,.T.);
#23711=ORIENTED_EDGE('',*,*,#16796,.F.);
#23712=ORIENTED_EDGE('',*,*,#16797,.T.);
#23713=ORIENTED_EDGE('',*,*,#16625,.F.);
#23714=ORIENTED_EDGE('',*,*,#16793,.F.);
#23715=ORIENTED_EDGE('',*,*,#16791,.F.);
#23716=ORIENTED_EDGE('',*,*,#16798,.T.);
#23717=ORIENTED_EDGE('',*,*,#16799,.T.);
#23718=ORIENTED_EDGE('',*,*,#16795,.F.);
#23719=ORIENTED_EDGE('',*,*,#16790,.F.);
#23720=ORIENTED_EDGE('',*,*,#16800,.F.);
#23721=ORIENTED_EDGE('',*,*,#16801,.F.);
#23722=ORIENTED_EDGE('',*,*,#16802,.F.);
#23723=ORIENTED_EDGE('',*,*,#16803,.T.);
#23724=ORIENTED_EDGE('',*,*,#16600,.T.);
#23725=ORIENTED_EDGE('',*,*,#16804,.T.);
#23726=ORIENTED_EDGE('',*,*,#16805,.F.);
#23727=ORIENTED_EDGE('',*,*,#16806,.F.);
#23728=ORIENTED_EDGE('',*,*,#16798,.F.);
#23729=ORIENTED_EDGE('',*,*,#16786,.F.);
#23730=ORIENTED_EDGE('',*,*,#16794,.F.);
#23731=ORIENTED_EDGE('',*,*,#16634,.T.);
#23732=ORIENTED_EDGE('',*,*,#16807,.F.);
#23733=ORIENTED_EDGE('',*,*,#16671,.T.);
#23734=ORIENTED_EDGE('',*,*,#16808,.T.);
#23735=ORIENTED_EDGE('',*,*,#16714,.F.);
#23736=ORIENTED_EDGE('',*,*,#16635,.T.);
#23737=ORIENTED_EDGE('',*,*,#16666,.F.);
#23738=ORIENTED_EDGE('',*,*,#16808,.F.);
#23739=ORIENTED_EDGE('',*,*,#16670,.F.);
#23740=ORIENTED_EDGE('',*,*,#16809,.F.);
#23741=ORIENTED_EDGE('',*,*,#16810,.F.);
#23742=ORIENTED_EDGE('',*,*,#16718,.T.);
#23743=ORIENTED_EDGE('',*,*,#16715,.F.);
#23744=ORIENTED_EDGE('',*,*,#16811,.T.);
#23745=ORIENTED_EDGE('',*,*,#16667,.T.);
#23746=ORIENTED_EDGE('',*,*,#16664,.F.);
#23747=ORIENTED_EDGE('',*,*,#16637,.F.);
#23748=ORIENTED_EDGE('',*,*,#16713,.T.);
#23749=ORIENTED_EDGE('',*,*,#16811,.F.);
#23750=ORIENTED_EDGE('',*,*,#16717,.T.);
#23751=ORIENTED_EDGE('',*,*,#16725,.F.);
#23752=ORIENTED_EDGE('',*,*,#16812,.F.);
#23753=ORIENTED_EDGE('',*,*,#16813,.F.);
#23754=ORIENTED_EDGE('',*,*,#16668,.T.);
#23755=ORIENTED_EDGE('',*,*,#16787,.F.);
#23756=ORIENTED_EDGE('',*,*,#16807,.T.);
#23757=ORIENTED_EDGE('',*,*,#16650,.T.);
#23758=ORIENTED_EDGE('',*,*,#16654,.T.);
#23759=ORIENTED_EDGE('',*,*,#16814,.T.);
#23760=ORIENTED_EDGE('',*,*,#16788,.F.);
#23761=ORIENTED_EDGE('',*,*,#16814,.F.);
#23762=ORIENTED_EDGE('',*,*,#16653,.F.);
#23763=ORIENTED_EDGE('',*,*,#16815,.T.);
#23764=ORIENTED_EDGE('',*,*,#16816,.F.);
#23765=ORIENTED_EDGE('',*,*,#16817,.F.);
#23766=ORIENTED_EDGE('',*,*,#16818,.F.);
#23767=ORIENTED_EDGE('',*,*,#16815,.F.);
#23768=ORIENTED_EDGE('',*,*,#16652,.F.);
#23769=ORIENTED_EDGE('',*,*,#16663,.T.);
#23770=ORIENTED_EDGE('',*,*,#16640,.F.);
#23771=ORIENTED_EDGE('',*,*,#16819,.F.);
#23772=ORIENTED_EDGE('',*,*,#16820,.F.);
#23773=ORIENTED_EDGE('',*,*,#16655,.F.);
#23774=ORIENTED_EDGE('',*,*,#16647,.F.);
#23775=ORIENTED_EDGE('',*,*,#16819,.T.);
#23776=ORIENTED_EDGE('',*,*,#16639,.T.);
#23777=ORIENTED_EDGE('',*,*,#16821,.F.);
#23778=ORIENTED_EDGE('',*,*,#16822,.T.);
#23779=ORIENTED_EDGE('',*,*,#16823,.T.);
#23780=ORIENTED_EDGE('',*,*,#16824,.T.);
#23781=ORIENTED_EDGE('',*,*,#16657,.T.);
#23782=ORIENTED_EDGE('',*,*,#16825,.T.);
#23783=ORIENTED_EDGE('',*,*,#16826,.F.);
#23784=ORIENTED_EDGE('',*,*,#16827,.T.);
#23785=ORIENTED_EDGE('',*,*,#16656,.T.);
#23786=ORIENTED_EDGE('',*,*,#16820,.T.);
#23787=ORIENTED_EDGE('',*,*,#16824,.F.);
#23788=ORIENTED_EDGE('',*,*,#16828,.F.);
#23789=ORIENTED_EDGE('',*,*,#16829,.F.);
#23790=ORIENTED_EDGE('',*,*,#16830,.F.);
#23791=ORIENTED_EDGE('',*,*,#16831,.F.);
#23792=ORIENTED_EDGE('',*,*,#16832,.F.);
#23793=ORIENTED_EDGE('',*,*,#16833,.F.);
#23794=ORIENTED_EDGE('',*,*,#16834,.F.);
#23795=ORIENTED_EDGE('',*,*,#16801,.T.);
#23796=ORIENTED_EDGE('',*,*,#16835,.F.);
#23797=ORIENTED_EDGE('',*,*,#16816,.T.);
#23798=ORIENTED_EDGE('',*,*,#16818,.T.);
#23799=ORIENTED_EDGE('',*,*,#16662,.T.);
#23800=ORIENTED_EDGE('',*,*,#16836,.F.);
#23801=ORIENTED_EDGE('',*,*,#16837,.F.);
#23802=ORIENTED_EDGE('',*,*,#16838,.F.);
#23803=ORIENTED_EDGE('',*,*,#16839,.F.);
#23804=ORIENTED_EDGE('',*,*,#16825,.F.);
#23805=ORIENTED_EDGE('',*,*,#16840,.T.);
#23806=ORIENTED_EDGE('',*,*,#16841,.T.);
#23807=ORIENTED_EDGE('',*,*,#16842,.T.);
#23808=ORIENTED_EDGE('',*,*,#16843,.T.);
#23809=ORIENTED_EDGE('',*,*,#16844,.T.);
#23810=ORIENTED_EDGE('',*,*,#16845,.T.);
#23811=ORIENTED_EDGE('',*,*,#16846,.T.);
#23812=ORIENTED_EDGE('',*,*,#16847,.T.);
#23813=ORIENTED_EDGE('',*,*,#16848,.T.);
#23814=ORIENTED_EDGE('',*,*,#16849,.T.);
#23815=ORIENTED_EDGE('',*,*,#16850,.T.);
#23816=ORIENTED_EDGE('',*,*,#16851,.T.);
#23817=ORIENTED_EDGE('',*,*,#16852,.T.);
#23818=ORIENTED_EDGE('',*,*,#16853,.T.);
#23819=ORIENTED_EDGE('',*,*,#16854,.F.);
#23820=ORIENTED_EDGE('',*,*,#16855,.T.);
#23821=ORIENTED_EDGE('',*,*,#16856,.T.);
#23822=ORIENTED_EDGE('',*,*,#16857,.T.);
#23823=ORIENTED_EDGE('',*,*,#16858,.T.);
#23824=ORIENTED_EDGE('',*,*,#16859,.T.);
#23825=ORIENTED_EDGE('',*,*,#16860,.T.);
#23826=ORIENTED_EDGE('',*,*,#16861,.T.);
#23827=ORIENTED_EDGE('',*,*,#16862,.T.);
#23828=ORIENTED_EDGE('',*,*,#16863,.T.);
#23829=ORIENTED_EDGE('',*,*,#16864,.T.);
#23830=ORIENTED_EDGE('',*,*,#16865,.T.);
#23831=ORIENTED_EDGE('',*,*,#16866,.T.);
#23832=ORIENTED_EDGE('',*,*,#16867,.T.);
#23833=ORIENTED_EDGE('',*,*,#16868,.T.);
#23834=ORIENTED_EDGE('',*,*,#16869,.T.);
#23835=ORIENTED_EDGE('',*,*,#16870,.T.);
#23836=ORIENTED_EDGE('',*,*,#16871,.T.);
#23837=ORIENTED_EDGE('',*,*,#16872,.T.);
#23838=ORIENTED_EDGE('',*,*,#16873,.T.);
#23839=ORIENTED_EDGE('',*,*,#16874,.T.);
#23840=ORIENTED_EDGE('',*,*,#16679,.T.);
#23841=ORIENTED_EDGE('',*,*,#16822,.F.);
#23842=ORIENTED_EDGE('',*,*,#16821,.T.);
#23843=ORIENTED_EDGE('',*,*,#16643,.T.);
#23844=ORIENTED_EDGE('',*,*,#16680,.T.);
#23845=ORIENTED_EDGE('',*,*,#16874,.F.);
#23846=ORIENTED_EDGE('',*,*,#16642,.F.);
#23847=ORIENTED_EDGE('',*,*,#16631,.T.);
#23848=ORIENTED_EDGE('',*,*,#16603,.F.);
#23849=ORIENTED_EDGE('',*,*,#16622,.F.);
#23850=ORIENTED_EDGE('',*,*,#16875,.F.);
#23851=ORIENTED_EDGE('',*,*,#16876,.F.);
#23852=ORIENTED_EDGE('',*,*,#16611,.F.);
#23853=ORIENTED_EDGE('',*,*,#16877,.F.);
#23854=ORIENTED_EDGE('',*,*,#16614,.T.);
#23855=ORIENTED_EDGE('',*,*,#16626,.F.);
#23856=ORIENTED_EDGE('',*,*,#16797,.F.);
#23857=ORIENTED_EDGE('',*,*,#16617,.T.);
#23858=ORIENTED_EDGE('',*,*,#16878,.F.);
#23859=ORIENTED_EDGE('',*,*,#16879,.T.);
#23860=ORIENTED_EDGE('',*,*,#16880,.F.);
#23861=ORIENTED_EDGE('',*,*,#16616,.T.);
#23862=ORIENTED_EDGE('',*,*,#16881,.T.);
#23863=ORIENTED_EDGE('',*,*,#16882,.F.);
#23864=ORIENTED_EDGE('',*,*,#16878,.T.);
#23865=ORIENTED_EDGE('',*,*,#16615,.T.);
#23866=ORIENTED_EDGE('',*,*,#16877,.T.);
#23867=ORIENTED_EDGE('',*,*,#16796,.T.);
#23868=ORIENTED_EDGE('',*,*,#16799,.F.);
#23869=ORIENTED_EDGE('',*,*,#16806,.T.);
#23870=ORIENTED_EDGE('',*,*,#16883,.F.);
#23871=ORIENTED_EDGE('',*,*,#16884,.F.);
#23872=ORIENTED_EDGE('',*,*,#16885,.F.);
#23873=ORIENTED_EDGE('',*,*,#16886,.F.);
#23874=ORIENTED_EDGE('',*,*,#16887,.F.);
#23875=ORIENTED_EDGE('',*,*,#16888,.F.);
#23876=ORIENTED_EDGE('',*,*,#16889,.F.);
#23877=ORIENTED_EDGE('',*,*,#16890,.F.);
#23878=ORIENTED_EDGE('',*,*,#16875,.T.);
#23879=ORIENTED_EDGE('',*,*,#16621,.T.);
#23880=ORIENTED_EDGE('',*,*,#16891,.F.);
#23881=ORIENTED_EDGE('',*,*,#16892,.F.);
#23882=ORIENTED_EDGE('',*,*,#16893,.F.);
#23883=ORIENTED_EDGE('',*,*,#16894,.F.);
#23884=ORIENTED_EDGE('',*,*,#16881,.F.);
#23885=ORIENTED_EDGE('',*,*,#16895,.F.);
#23886=ORIENTED_EDGE('',*,*,#16876,.T.);
#23887=ORIENTED_EDGE('',*,*,#16890,.T.);
#23888=ORIENTED_EDGE('',*,*,#16896,.F.);
#23889=ORIENTED_EDGE('',*,*,#16897,.T.);
#23890=ORIENTED_EDGE('',*,*,#16898,.T.);
#23891=ORIENTED_EDGE('',*,*,#16606,.F.);
#23892=ORIENTED_EDGE('',*,*,#16897,.F.);
#23893=ORIENTED_EDGE('',*,*,#16682,.T.);
#23894=ORIENTED_EDGE('',*,*,#16899,.F.);
#23895=ORIENTED_EDGE('',*,*,#16607,.F.);
#23896=ORIENTED_EDGE('',*,*,#16898,.F.);
#23897=ORIENTED_EDGE('',*,*,#16899,.T.);
#23898=ORIENTED_EDGE('',*,*,#16681,.T.);
#23899=ORIENTED_EDGE('',*,*,#16629,.T.);
#23900=ORIENTED_EDGE('',*,*,#16608,.T.);
#23901=ORIENTED_EDGE('',*,*,#16810,.T.);
#23902=ORIENTED_EDGE('',*,*,#16900,.F.);
#23903=ORIENTED_EDGE('',*,*,#16901,.F.);
#23904=ORIENTED_EDGE('',*,*,#16719,.F.);
#23905=ORIENTED_EDGE('',*,*,#16812,.T.);
#23906=ORIENTED_EDGE('',*,*,#16724,.F.);
#23907=ORIENTED_EDGE('',*,*,#16902,.F.);
#23908=ORIENTED_EDGE('',*,*,#16903,.F.);
#23909=ORIENTED_EDGE('',*,*,#16904,.F.);
#23910=ORIENTED_EDGE('',*,*,#16905,.F.);
#23911=ORIENTED_EDGE('',*,*,#16906,.F.);
#23912=ORIENTED_EDGE('',*,*,#16907,.F.);
#23913=ORIENTED_EDGE('',*,*,#16772,.F.);
#23914=ORIENTED_EDGE('',*,*,#16803,.F.);
#23915=ORIENTED_EDGE('',*,*,#16908,.F.);
#23916=ORIENTED_EDGE('',*,*,#16804,.F.);
#23917=ORIENTED_EDGE('',*,*,#16770,.F.);
#23918=ORIENTED_EDGE('',*,*,#16909,.F.);
#23919=ORIENTED_EDGE('',*,*,#16910,.F.);
#23920=ORIENTED_EDGE('',*,*,#16911,.F.);
#23921=ORIENTED_EDGE('',*,*,#16912,.F.);
#23922=ORIENTED_EDGE('',*,*,#16777,.F.);
#23923=ORIENTED_EDGE('',*,*,#16599,.F.);
#23924=ORIENTED_EDGE('',*,*,#16913,.F.);
#23925=ORIENTED_EDGE('',*,*,#16601,.F.);
#23926=ORIENTED_EDGE('',*,*,#16776,.F.);
#23927=ORIENTED_EDGE('',*,*,#16913,.T.);
#23928=ORIENTED_EDGE('',*,*,#16775,.T.);
#23929=ORIENTED_EDGE('',*,*,#16914,.F.);
#23930=ORIENTED_EDGE('',*,*,#16593,.T.);
#23931=ORIENTED_EDGE('',*,*,#16581,.F.);
#23932=ORIENTED_EDGE('',*,*,#16597,.T.);
#23933=ORIENTED_EDGE('',*,*,#16912,.T.);
#23934=ORIENTED_EDGE('',*,*,#16598,.T.);
#23935=ORIENTED_EDGE('',*,*,#16590,.F.);
#23936=ORIENTED_EDGE('',*,*,#16915,.T.);
#23937=ORIENTED_EDGE('',*,*,#16916,.F.);
#23938=ORIENTED_EDGE('',*,*,#16767,.T.);
#23939=ORIENTED_EDGE('',*,*,#16706,.T.);
#23940=ORIENTED_EDGE('',*,*,#16917,.T.);
#23941=ORIENTED_EDGE('',*,*,#16918,.T.);
#23942=ORIENTED_EDGE('',*,*,#16462,.T.);
#23943=ORIENTED_EDGE('',*,*,#16780,.F.);
#23944=ORIENTED_EDGE('',*,*,#16704,.T.);
#23945=ORIENTED_EDGE('',*,*,#16919,.T.);
#23946=ORIENTED_EDGE('',*,*,#16888,.T.);
#23947=ORIENTED_EDGE('',*,*,#16920,.F.);
#23948=ORIENTED_EDGE('',*,*,#16905,.T.);
#23949=ORIENTED_EDGE('',*,*,#16921,.F.);
#23950=ORIENTED_EDGE('',*,*,#16922,.F.);
#23951=ORIENTED_EDGE('',*,*,#16789,.F.);
#23952=ORIENTED_EDGE('',*,*,#16817,.T.);
#23953=ORIENTED_EDGE('',*,*,#16835,.T.);
#23954=ORIENTED_EDGE('',*,*,#16800,.T.);
#23955=ORIENTED_EDGE('',*,*,#16805,.T.);
#23956=ORIENTED_EDGE('',*,*,#16908,.T.);
#23957=ORIENTED_EDGE('',*,*,#16923,.T.);
#23958=ORIENTED_EDGE('',*,*,#16924,.T.);
#23959=ORIENTED_EDGE('',*,*,#16925,.T.);
#23960=ORIENTED_EDGE('',*,*,#16883,.T.);
#23961=ORIENTED_EDGE('',*,*,#16909,.T.);
#23962=ORIENTED_EDGE('',*,*,#16769,.F.);
#23963=ORIENTED_EDGE('',*,*,#16926,.F.);
#23964=ORIENTED_EDGE('',*,*,#16911,.T.);
#23965=ORIENTED_EDGE('',*,*,#16927,.F.);
#23966=ORIENTED_EDGE('',*,*,#16923,.F.);
#23967=ORIENTED_EDGE('',*,*,#16747,.F.);
#23968=ORIENTED_EDGE('',*,*,#16750,.F.);
#23969=ORIENTED_EDGE('',*,*,#16928,.F.);
#23970=ORIENTED_EDGE('',*,*,#16929,.F.);
#23971=ORIENTED_EDGE('',*,*,#16735,.F.);
#23972=ORIENTED_EDGE('',*,*,#16930,.F.);
#23973=ORIENTED_EDGE('',*,*,#16931,.F.);
#23974=ORIENTED_EDGE('',*,*,#16932,.F.);
#23975=ORIENTED_EDGE('',*,*,#16933,.F.);
#23976=ORIENTED_EDGE('',*,*,#16928,.T.);
#23977=ORIENTED_EDGE('',*,*,#16749,.F.);
#23978=ORIENTED_EDGE('',*,*,#16752,.T.);
#23979=ORIENTED_EDGE('',*,*,#16934,.F.);
#23980=ORIENTED_EDGE('',*,*,#16743,.T.);
#23981=ORIENTED_EDGE('',*,*,#16935,.F.);
#23982=ORIENTED_EDGE('',*,*,#16931,.T.);
#23983=ORIENTED_EDGE('',*,*,#16736,.F.);
#23984=ORIENTED_EDGE('',*,*,#16932,.T.);
#23985=ORIENTED_EDGE('',*,*,#16935,.T.);
#23986=ORIENTED_EDGE('',*,*,#16742,.T.);
#23987=ORIENTED_EDGE('',*,*,#16741,.T.);
#23988=ORIENTED_EDGE('',*,*,#16936,.F.);
#23989=ORIENTED_EDGE('',*,*,#16709,.T.);
#23990=ORIENTED_EDGE('',*,*,#16937,.F.);
#23991=ORIENTED_EDGE('',*,*,#16938,.F.);
#23992=ORIENTED_EDGE('',*,*,#16917,.F.);
#23993=ORIENTED_EDGE('',*,*,#16705,.T.);
#23994=ORIENTED_EDGE('',*,*,#16939,.F.);
#23995=ORIENTED_EDGE('',*,*,#16933,.T.);
#23996=ORIENTED_EDGE('',*,*,#16940,.T.);
#23997=ORIENTED_EDGE('',*,*,#16831,.T.);
#23998=ORIENTED_EDGE('',*,*,#16941,.F.);
#23999=ORIENTED_EDGE('',*,*,#16660,.T.);
#24000=ORIENTED_EDGE('',*,*,#16942,.F.);
#24001=ORIENTED_EDGE('',*,*,#16943,.T.);
#24002=ORIENTED_EDGE('',*,*,#16944,.F.);
#24003=ORIENTED_EDGE('',*,*,#16945,.F.);
#24004=ORIENTED_EDGE('',*,*,#16943,.F.);
#24005=ORIENTED_EDGE('',*,*,#16946,.F.);
#24006=ORIENTED_EDGE('',*,*,#16947,.F.);
#24007=ORIENTED_EDGE('',*,*,#16948,.F.);
#24008=ORIENTED_EDGE('',*,*,#16949,.F.);
#24009=ORIENTED_EDGE('',*,*,#16950,.F.);
#24010=ORIENTED_EDGE('',*,*,#16879,.F.);
#24011=ORIENTED_EDGE('',*,*,#16813,.T.);
#24012=ORIENTED_EDGE('',*,*,#16903,.T.);
#24013=ORIENTED_EDGE('',*,*,#16951,.F.);
#24014=ORIENTED_EDGE('',*,*,#16952,.F.);
#24015=ORIENTED_EDGE('',*,*,#16953,.F.);
#24016=ORIENTED_EDGE('',*,*,#16900,.T.);
#24017=ORIENTED_EDGE('',*,*,#16809,.T.);
#24018=ORIENTED_EDGE('',*,*,#16669,.T.);
#24019=ORIENTED_EDGE('',*,*,#16954,.F.);
#24020=ORIENTED_EDGE('',*,*,#16955,.F.);
#24021=ORIENTED_EDGE('',*,*,#16956,.F.);
#24022=ORIENTED_EDGE('',*,*,#16957,.T.);
#24023=ORIENTED_EDGE('',*,*,#16958,.F.);
#24024=ORIENTED_EDGE('',*,*,#16959,.T.);
#24025=ORIENTED_EDGE('',*,*,#16960,.F.);
#24026=ORIENTED_EDGE('',*,*,#16961,.F.);
#24027=ORIENTED_EDGE('',*,*,#16658,.T.);
#24028=ORIENTED_EDGE('',*,*,#16827,.F.);
#24029=ORIENTED_EDGE('',*,*,#16957,.F.);
#24030=ORIENTED_EDGE('',*,*,#16962,.F.);
#24031=ORIENTED_EDGE('',*,*,#16659,.T.);
#24032=ORIENTED_EDGE('',*,*,#16962,.T.);
#24033=ORIENTED_EDGE('',*,*,#16956,.T.);
#24034=ORIENTED_EDGE('',*,*,#16963,.T.);
#24035=ORIENTED_EDGE('',*,*,#16946,.T.);
#24036=ORIENTED_EDGE('',*,*,#16942,.T.);
#24037=ORIENTED_EDGE('',*,*,#16619,.T.);
#24038=ORIENTED_EDGE('',*,*,#16964,.F.);
#24039=ORIENTED_EDGE('',*,*,#16959,.F.);
#24040=ORIENTED_EDGE('',*,*,#16965,.F.);
#24041=ORIENTED_EDGE('',*,*,#16955,.T.);
#24042=ORIENTED_EDGE('',*,*,#16966,.T.);
#24043=ORIENTED_EDGE('',*,*,#16961,.T.);
#24044=ORIENTED_EDGE('',*,*,#16967,.F.);
#24045=ORIENTED_EDGE('',*,*,#16949,.T.);
#24046=ORIENTED_EDGE('',*,*,#16968,.T.);
#24047=ORIENTED_EDGE('',*,*,#16947,.T.);
#24048=ORIENTED_EDGE('',*,*,#16963,.F.);
#24049=ORIENTED_EDGE('',*,*,#16618,.T.);
#24050=ORIENTED_EDGE('',*,*,#16880,.T.);
#24051=ORIENTED_EDGE('',*,*,#16950,.T.);
#24052=ORIENTED_EDGE('',*,*,#16967,.T.);
#24053=ORIENTED_EDGE('',*,*,#16960,.T.);
#24054=ORIENTED_EDGE('',*,*,#16964,.T.);
#24055=ORIENTED_EDGE('',*,*,#16620,.T.);
#24056=ORIENTED_EDGE('',*,*,#16965,.T.);
#24057=ORIENTED_EDGE('',*,*,#16969,.T.);
#24058=ORIENTED_EDGE('',*,*,#16891,.T.);
#24059=ORIENTED_EDGE('',*,*,#16902,.T.);
#24060=ORIENTED_EDGE('',*,*,#16723,.F.);
#24061=ORIENTED_EDGE('',*,*,#16459,.T.);
#24062=ORIENTED_EDGE('',*,*,#16970,.T.);
#24063=ORIENTED_EDGE('',*,*,#16951,.T.);
#24064=ORIENTED_EDGE('',*,*,#16584,.F.);
#24065=ORIENTED_EDGE('',*,*,#16596,.F.);
#24066=ORIENTED_EDGE('',*,*,#16971,.T.);
#24067=ORIENTED_EDGE('',*,*,#16972,.F.);
#24068=ORIENTED_EDGE('',*,*,#16587,.F.);
#24069=ORIENTED_EDGE('',*,*,#16973,.F.);
#24070=ORIENTED_EDGE('',*,*,#16974,.T.);
#24071=ORIENTED_EDGE('',*,*,#16975,.F.);
#24072=ORIENTED_EDGE('',*,*,#16976,.F.);
#24073=ORIENTED_EDGE('',*,*,#16977,.F.);
#24074=ORIENTED_EDGE('',*,*,#16971,.F.);
#24075=ORIENTED_EDGE('',*,*,#16595,.F.);
#24076=ORIENTED_EDGE('',*,*,#16978,.F.);
#24077=ORIENTED_EDGE('',*,*,#16979,.F.);
#24078=ORIENTED_EDGE('',*,*,#16974,.F.);
#24079=ORIENTED_EDGE('',*,*,#16980,.F.);
#24080=ORIENTED_EDGE('',*,*,#16585,.F.);
#24081=ORIENTED_EDGE('',*,*,#16981,.F.);
#24082=ORIENTED_EDGE('',*,*,#16589,.F.);
#24083=ORIENTED_EDGE('',*,*,#16580,.F.);
#24084=ORIENTED_EDGE('',*,*,#16588,.F.);
#24085=ORIENTED_EDGE('',*,*,#16975,.T.);
#24086=ORIENTED_EDGE('',*,*,#16979,.T.);
#24087=ORIENTED_EDGE('',*,*,#16982,.F.);
#24088=ORIENTED_EDGE('',*,*,#16915,.F.);
#24089=ORIENTED_EDGE('',*,*,#16592,.F.);
#24090=ORIENTED_EDGE('',*,*,#16910,.T.);
#24091=ORIENTED_EDGE('',*,*,#16926,.T.);
#24092=ORIENTED_EDGE('',*,*,#16768,.T.);
#24093=ORIENTED_EDGE('',*,*,#16916,.T.);
#24094=ORIENTED_EDGE('',*,*,#16982,.T.);
#24095=ORIENTED_EDGE('',*,*,#16978,.T.);
#24096=ORIENTED_EDGE('',*,*,#16983,.F.);
#24097=ORIENTED_EDGE('',*,*,#16984,.T.);
#24098=ORIENTED_EDGE('',*,*,#16924,.F.);
#24099=ORIENTED_EDGE('',*,*,#16927,.T.);
#24100=ORIENTED_EDGE('',*,*,#16980,.T.);
#24101=ORIENTED_EDGE('',*,*,#16985,.T.);
#24102=ORIENTED_EDGE('',*,*,#16884,.T.);
#24103=ORIENTED_EDGE('',*,*,#16925,.F.);
#24104=ORIENTED_EDGE('',*,*,#16984,.F.);
#24105=ORIENTED_EDGE('',*,*,#16983,.T.);
#24106=ORIENTED_EDGE('',*,*,#16739,.T.);
#24107=ORIENTED_EDGE('',*,*,#16986,.F.);
#24108=ORIENTED_EDGE('',*,*,#16981,.T.);
#24109=ORIENTED_EDGE('',*,*,#16987,.F.);
#24110=ORIENTED_EDGE('',*,*,#16865,.F.);
#24111=ORIENTED_EDGE('',*,*,#16988,.T.);
#24112=ORIENTED_EDGE('',*,*,#16989,.F.);
#24113=ORIENTED_EDGE('',*,*,#16990,.F.);
#24114=ORIENTED_EDGE('',*,*,#16866,.F.);
#24115=ORIENTED_EDGE('',*,*,#16990,.T.);
#24116=ORIENTED_EDGE('',*,*,#16991,.F.);
#24117=ORIENTED_EDGE('',*,*,#16992,.F.);
#24118=ORIENTED_EDGE('',*,*,#16867,.F.);
#24119=ORIENTED_EDGE('',*,*,#16992,.T.);
#24120=ORIENTED_EDGE('',*,*,#16993,.F.);
#24121=ORIENTED_EDGE('',*,*,#16994,.F.);
#24122=ORIENTED_EDGE('',*,*,#16868,.F.);
#24123=ORIENTED_EDGE('',*,*,#16994,.T.);
#24124=ORIENTED_EDGE('',*,*,#16995,.F.);
#24125=ORIENTED_EDGE('',*,*,#16996,.F.);
#24126=ORIENTED_EDGE('',*,*,#16869,.F.);
#24127=ORIENTED_EDGE('',*,*,#16996,.T.);
#24128=ORIENTED_EDGE('',*,*,#16997,.F.);
#24129=ORIENTED_EDGE('',*,*,#16998,.F.);
#24130=ORIENTED_EDGE('',*,*,#16870,.F.);
#24131=ORIENTED_EDGE('',*,*,#16998,.T.);
#24132=ORIENTED_EDGE('',*,*,#16999,.F.);
#24133=ORIENTED_EDGE('',*,*,#17000,.F.);
#24134=ORIENTED_EDGE('',*,*,#16871,.F.);
#24135=ORIENTED_EDGE('',*,*,#17000,.T.);
#24136=ORIENTED_EDGE('',*,*,#17001,.F.);
#24137=ORIENTED_EDGE('',*,*,#17002,.F.);
#24138=ORIENTED_EDGE('',*,*,#16872,.F.);
#24139=ORIENTED_EDGE('',*,*,#17002,.T.);
#24140=ORIENTED_EDGE('',*,*,#17003,.F.);
#24141=ORIENTED_EDGE('',*,*,#17004,.F.);
#24142=ORIENTED_EDGE('',*,*,#16873,.F.);
#24143=ORIENTED_EDGE('',*,*,#17004,.T.);
#24144=ORIENTED_EDGE('',*,*,#17005,.F.);
#24145=ORIENTED_EDGE('',*,*,#16988,.F.);
#24146=ORIENTED_EDGE('',*,*,#17005,.T.);
#24147=ORIENTED_EDGE('',*,*,#17003,.T.);
#24148=ORIENTED_EDGE('',*,*,#17001,.T.);
#24149=ORIENTED_EDGE('',*,*,#16999,.T.);
#24150=ORIENTED_EDGE('',*,*,#16997,.T.);
#24151=ORIENTED_EDGE('',*,*,#16995,.T.);
#24152=ORIENTED_EDGE('',*,*,#16993,.T.);
#24153=ORIENTED_EDGE('',*,*,#16991,.T.);
#24154=ORIENTED_EDGE('',*,*,#16989,.T.);
#24155=ORIENTED_EDGE('',*,*,#16855,.F.);
#24156=ORIENTED_EDGE('',*,*,#17006,.T.);
#24157=ORIENTED_EDGE('',*,*,#17007,.F.);
#24158=ORIENTED_EDGE('',*,*,#17008,.F.);
#24159=ORIENTED_EDGE('',*,*,#16856,.F.);
#24160=ORIENTED_EDGE('',*,*,#17008,.T.);
#24161=ORIENTED_EDGE('',*,*,#17009,.F.);
#24162=ORIENTED_EDGE('',*,*,#17010,.F.);
#24163=ORIENTED_EDGE('',*,*,#16857,.F.);
#24164=ORIENTED_EDGE('',*,*,#17010,.T.);
#24165=ORIENTED_EDGE('',*,*,#17011,.F.);
#24166=ORIENTED_EDGE('',*,*,#17012,.F.);
#24167=ORIENTED_EDGE('',*,*,#16858,.F.);
#24168=ORIENTED_EDGE('',*,*,#17012,.T.);
#24169=ORIENTED_EDGE('',*,*,#17013,.F.);
#24170=ORIENTED_EDGE('',*,*,#17014,.F.);
#24171=ORIENTED_EDGE('',*,*,#16859,.F.);
#24172=ORIENTED_EDGE('',*,*,#17014,.T.);
#24173=ORIENTED_EDGE('',*,*,#17015,.F.);
#24174=ORIENTED_EDGE('',*,*,#17016,.F.);
#24175=ORIENTED_EDGE('',*,*,#16860,.F.);
#24176=ORIENTED_EDGE('',*,*,#17016,.T.);
#24177=ORIENTED_EDGE('',*,*,#17017,.F.);
#24178=ORIENTED_EDGE('',*,*,#17018,.F.);
#24179=ORIENTED_EDGE('',*,*,#16861,.F.);
#24180=ORIENTED_EDGE('',*,*,#17018,.T.);
#24181=ORIENTED_EDGE('',*,*,#17019,.F.);
#24182=ORIENTED_EDGE('',*,*,#17020,.F.);
#24183=ORIENTED_EDGE('',*,*,#16862,.F.);
#24184=ORIENTED_EDGE('',*,*,#17020,.T.);
#24185=ORIENTED_EDGE('',*,*,#17021,.F.);
#24186=ORIENTED_EDGE('',*,*,#17022,.F.);
#24187=ORIENTED_EDGE('',*,*,#16863,.F.);
#24188=ORIENTED_EDGE('',*,*,#17022,.T.);
#24189=ORIENTED_EDGE('',*,*,#17023,.F.);
#24190=ORIENTED_EDGE('',*,*,#17024,.F.);
#24191=ORIENTED_EDGE('',*,*,#16864,.F.);
#24192=ORIENTED_EDGE('',*,*,#17024,.T.);
#24193=ORIENTED_EDGE('',*,*,#17025,.F.);
#24194=ORIENTED_EDGE('',*,*,#17006,.F.);
#24195=ORIENTED_EDGE('',*,*,#17025,.T.);
#24196=ORIENTED_EDGE('',*,*,#17023,.T.);
#24197=ORIENTED_EDGE('',*,*,#17021,.T.);
#24198=ORIENTED_EDGE('',*,*,#17019,.T.);
#24199=ORIENTED_EDGE('',*,*,#17017,.T.);
#24200=ORIENTED_EDGE('',*,*,#17015,.T.);
#24201=ORIENTED_EDGE('',*,*,#17013,.T.);
#24202=ORIENTED_EDGE('',*,*,#17011,.T.);
#24203=ORIENTED_EDGE('',*,*,#17009,.T.);
#24204=ORIENTED_EDGE('',*,*,#17007,.T.);
#24205=ORIENTED_EDGE('',*,*,#17026,.F.);
#24206=ORIENTED_EDGE('',*,*,#17027,.T.);
#24207=ORIENTED_EDGE('',*,*,#17028,.F.);
#24208=ORIENTED_EDGE('',*,*,#17029,.F.);
#24209=ORIENTED_EDGE('',*,*,#17030,.F.);
#24210=ORIENTED_EDGE('',*,*,#17029,.T.);
#24211=ORIENTED_EDGE('',*,*,#17031,.F.);
#24212=ORIENTED_EDGE('',*,*,#17032,.F.);
#24213=ORIENTED_EDGE('',*,*,#17033,.F.);
#24214=ORIENTED_EDGE('',*,*,#17032,.T.);
#24215=ORIENTED_EDGE('',*,*,#17034,.F.);
#24216=ORIENTED_EDGE('',*,*,#17035,.F.);
#24217=ORIENTED_EDGE('',*,*,#17036,.F.);
#24218=ORIENTED_EDGE('',*,*,#17035,.T.);
#24219=ORIENTED_EDGE('',*,*,#17037,.F.);
#24220=ORIENTED_EDGE('',*,*,#17038,.F.);
#24221=ORIENTED_EDGE('',*,*,#17039,.F.);
#24222=ORIENTED_EDGE('',*,*,#17038,.T.);
#24223=ORIENTED_EDGE('',*,*,#17040,.F.);
#24224=ORIENTED_EDGE('',*,*,#17041,.F.);
#24225=ORIENTED_EDGE('',*,*,#17042,.F.);
#24226=ORIENTED_EDGE('',*,*,#17041,.T.);
#24227=ORIENTED_EDGE('',*,*,#17043,.F.);
#24228=ORIENTED_EDGE('',*,*,#17044,.F.);
#24229=ORIENTED_EDGE('',*,*,#17045,.F.);
#24230=ORIENTED_EDGE('',*,*,#17044,.T.);
#24231=ORIENTED_EDGE('',*,*,#17046,.F.);
#24232=ORIENTED_EDGE('',*,*,#17047,.F.);
#24233=ORIENTED_EDGE('',*,*,#17048,.F.);
#24234=ORIENTED_EDGE('',*,*,#17047,.T.);
#24235=ORIENTED_EDGE('',*,*,#17049,.F.);
#24236=ORIENTED_EDGE('',*,*,#17027,.F.);
#24237=ORIENTED_EDGE('',*,*,#16840,.F.);
#24238=ORIENTED_EDGE('',*,*,#17050,.T.);
#24239=ORIENTED_EDGE('',*,*,#17051,.F.);
#24240=ORIENTED_EDGE('',*,*,#17052,.F.);
#24241=ORIENTED_EDGE('',*,*,#16841,.F.);
#24242=ORIENTED_EDGE('',*,*,#17052,.T.);
#24243=ORIENTED_EDGE('',*,*,#17053,.F.);
#24244=ORIENTED_EDGE('',*,*,#17054,.F.);
#24245=ORIENTED_EDGE('',*,*,#16842,.F.);
#24246=ORIENTED_EDGE('',*,*,#17054,.T.);
#24247=ORIENTED_EDGE('',*,*,#17055,.F.);
#24248=ORIENTED_EDGE('',*,*,#17056,.F.);
#24249=ORIENTED_EDGE('',*,*,#16843,.F.);
#24250=ORIENTED_EDGE('',*,*,#17056,.T.);
#24251=ORIENTED_EDGE('',*,*,#17057,.F.);
#24252=ORIENTED_EDGE('',*,*,#17058,.F.);
#24253=ORIENTED_EDGE('',*,*,#16844,.F.);
#24254=ORIENTED_EDGE('',*,*,#17058,.T.);
#24255=ORIENTED_EDGE('',*,*,#17059,.F.);
#24256=ORIENTED_EDGE('',*,*,#17060,.F.);
#24257=ORIENTED_EDGE('',*,*,#16845,.F.);
#24258=ORIENTED_EDGE('',*,*,#17060,.T.);
#24259=ORIENTED_EDGE('',*,*,#17061,.F.);
#24260=ORIENTED_EDGE('',*,*,#17062,.F.);
#24261=ORIENTED_EDGE('',*,*,#16846,.F.);
#24262=ORIENTED_EDGE('',*,*,#17062,.T.);
#24263=ORIENTED_EDGE('',*,*,#17063,.F.);
#24264=ORIENTED_EDGE('',*,*,#17064,.F.);
#24265=ORIENTED_EDGE('',*,*,#16847,.F.);
#24266=ORIENTED_EDGE('',*,*,#17064,.T.);
#24267=ORIENTED_EDGE('',*,*,#17065,.F.);
#24268=ORIENTED_EDGE('',*,*,#17066,.F.);
#24269=ORIENTED_EDGE('',*,*,#16848,.F.);
#24270=ORIENTED_EDGE('',*,*,#17066,.T.);
#24271=ORIENTED_EDGE('',*,*,#17067,.F.);
#24272=ORIENTED_EDGE('',*,*,#17068,.F.);
#24273=ORIENTED_EDGE('',*,*,#16849,.F.);
#24274=ORIENTED_EDGE('',*,*,#17068,.T.);
#24275=ORIENTED_EDGE('',*,*,#17069,.F.);
#24276=ORIENTED_EDGE('',*,*,#17050,.F.);
#24277=ORIENTED_EDGE('',*,*,#17069,.T.);
#24278=ORIENTED_EDGE('',*,*,#17067,.T.);
#24279=ORIENTED_EDGE('',*,*,#17065,.T.);
#24280=ORIENTED_EDGE('',*,*,#17063,.T.);
#24281=ORIENTED_EDGE('',*,*,#17061,.T.);
#24282=ORIENTED_EDGE('',*,*,#17059,.T.);
#24283=ORIENTED_EDGE('',*,*,#17057,.T.);
#24284=ORIENTED_EDGE('',*,*,#17055,.T.);
#24285=ORIENTED_EDGE('',*,*,#17053,.T.);
#24286=ORIENTED_EDGE('',*,*,#17051,.T.);
#24287=ORIENTED_EDGE('',*,*,#17049,.T.);
#24288=ORIENTED_EDGE('',*,*,#17046,.T.);
#24289=ORIENTED_EDGE('',*,*,#17043,.T.);
#24290=ORIENTED_EDGE('',*,*,#17040,.T.);
#24291=ORIENTED_EDGE('',*,*,#17037,.T.);
#24292=ORIENTED_EDGE('',*,*,#17034,.T.);
#24293=ORIENTED_EDGE('',*,*,#17031,.T.);
#24294=ORIENTED_EDGE('',*,*,#17028,.T.);
#24295=ORIENTED_EDGE('',*,*,#16850,.F.);
#24296=ORIENTED_EDGE('',*,*,#17070,.T.);
#24297=ORIENTED_EDGE('',*,*,#17071,.F.);
#24298=ORIENTED_EDGE('',*,*,#17072,.F.);
#24299=ORIENTED_EDGE('',*,*,#16851,.F.);
#24300=ORIENTED_EDGE('',*,*,#17072,.T.);
#24301=ORIENTED_EDGE('',*,*,#17073,.F.);
#24302=ORIENTED_EDGE('',*,*,#17074,.F.);
#24303=ORIENTED_EDGE('',*,*,#16852,.F.);
#24304=ORIENTED_EDGE('',*,*,#17074,.T.);
#24305=ORIENTED_EDGE('',*,*,#17075,.F.);
#24306=ORIENTED_EDGE('',*,*,#17076,.F.);
#24307=ORIENTED_EDGE('',*,*,#16853,.F.);
#24308=ORIENTED_EDGE('',*,*,#17076,.T.);
#24309=ORIENTED_EDGE('',*,*,#17077,.F.);
#24310=ORIENTED_EDGE('',*,*,#17070,.F.);
#24311=ORIENTED_EDGE('',*,*,#17077,.T.);
#24312=ORIENTED_EDGE('',*,*,#17075,.T.);
#24313=ORIENTED_EDGE('',*,*,#17073,.T.);
#24314=ORIENTED_EDGE('',*,*,#17071,.T.);
#24315=ORIENTED_EDGE('',*,*,#17078,.T.);
#24316=ORIENTED_EDGE('',*,*,#16572,.F.);
#24317=ORIENTED_EDGE('',*,*,#17078,.F.);
#24318=ORIENTED_EDGE('',*,*,#17079,.T.);
#24319=ORIENTED_EDGE('',*,*,#16766,.F.);
#24320=ORIENTED_EDGE('',*,*,#17079,.F.);
#24321=ORIENTED_EDGE('',*,*,#17080,.T.);
#24322=ORIENTED_EDGE('',*,*,#16568,.F.);
#24323=ORIENTED_EDGE('',*,*,#17080,.F.);
#24324=ORIENTED_EDGE('',*,*,#17081,.T.);
#24325=ORIENTED_EDGE('',*,*,#16764,.F.);
#24326=ORIENTED_EDGE('',*,*,#17081,.F.);
#24327=ORIENTED_EDGE('',*,*,#16563,.F.);
#24328=ORIENTED_EDGE('',*,*,#17082,.T.);
#24329=ORIENTED_EDGE('',*,*,#16765,.F.);
#24330=ORIENTED_EDGE('',*,*,#17082,.F.);
#24331=ORIENTED_EDGE('',*,*,#16556,.F.);
#24332=ORIENTED_EDGE('',*,*,#17083,.T.);
#24333=ORIENTED_EDGE('',*,*,#16763,.F.);
#24334=ORIENTED_EDGE('',*,*,#17083,.F.);
#24335=ORIENTED_EDGE('',*,*,#16501,.F.);
#24336=ORIENTED_EDGE('',*,*,#16547,.T.);
#24337=ORIENTED_EDGE('',*,*,#17084,.F.);
#24338=ORIENTED_EDGE('',*,*,#16526,.F.);
#24339=ORIENTED_EDGE('',*,*,#16513,.F.);
#24340=ORIENTED_EDGE('',*,*,#17085,.T.);
#24341=ORIENTED_EDGE('',*,*,#16545,.T.);
#24342=ORIENTED_EDGE('',*,*,#16550,.F.);
#24343=ORIENTED_EDGE('',*,*,#16522,.F.);
#24344=ORIENTED_EDGE('',*,*,#17084,.T.);
#24345=ORIENTED_EDGE('',*,*,#16546,.T.);
#24346=ORIENTED_EDGE('',*,*,#17085,.F.);
#24347=ORIENTED_EDGE('',*,*,#16519,.F.);
#24348=ORIENTED_EDGE('',*,*,#16473,.F.);
#24349=ORIENTED_EDGE('',*,*,#16755,.F.);
#24350=ORIENTED_EDGE('',*,*,#16493,.T.);
#24351=ORIENTED_EDGE('',*,*,#16484,.F.);
#24352=ORIENTED_EDGE('',*,*,#17086,.T.);
#24353=ORIENTED_EDGE('',*,*,#17087,.F.);
#24354=ORIENTED_EDGE('',*,*,#16531,.T.);
#24355=ORIENTED_EDGE('',*,*,#16495,.F.);
#24356=ORIENTED_EDGE('',*,*,#16483,.F.);
#24357=ORIENTED_EDGE('',*,*,#16489,.F.);
#24358=ORIENTED_EDGE('',*,*,#17088,.F.);
#24359=ORIENTED_EDGE('',*,*,#17086,.F.);
#24360=ORIENTED_EDGE('',*,*,#16938,.T.);
#24361=ORIENTED_EDGE('',*,*,#17089,.T.);
#24362=ORIENTED_EDGE('',*,*,#16456,.T.);
#24363=ORIENTED_EDGE('',*,*,#16918,.F.);
#24364=ORIENTED_EDGE('',*,*,#16708,.T.);
#24365=ORIENTED_EDGE('',*,*,#16779,.T.);
#24366=ORIENTED_EDGE('',*,*,#17090,.T.);
#24367=ORIENTED_EDGE('',*,*,#17089,.F.);
#24368=ORIENTED_EDGE('',*,*,#16937,.T.);
#24369=ORIENTED_EDGE('',*,*,#16454,.F.);
#24370=ORIENTED_EDGE('',*,*,#16450,.F.);
#24371=ORIENTED_EDGE('',*,*,#16457,.F.);
#24372=ORIENTED_EDGE('',*,*,#17090,.F.);
#24373=ORIENTED_EDGE('',*,*,#16778,.T.);
#24374=ORIENTED_EDGE('',*,*,#16721,.T.);
#24375=ORIENTED_EDGE('',*,*,#17091,.F.);
#24376=ORIENTED_EDGE('',*,*,#17092,.F.);
#24377=ORIENTED_EDGE('',*,*,#16446,.F.);
#24378=ORIENTED_EDGE('',*,*,#16952,.T.);
#24379=ORIENTED_EDGE('',*,*,#16970,.F.);
#24380=ORIENTED_EDGE('',*,*,#17093,.T.);
#24381=ORIENTED_EDGE('',*,*,#17094,.T.);
#24382=ORIENTED_EDGE('',*,*,#16901,.T.);
#24383=ORIENTED_EDGE('',*,*,#16953,.T.);
#24384=ORIENTED_EDGE('',*,*,#17094,.F.);
#24385=ORIENTED_EDGE('',*,*,#17091,.T.);
#24386=ORIENTED_EDGE('',*,*,#16720,.T.);
#24387=ORIENTED_EDGE('',*,*,#16442,.F.);
#24388=ORIENTED_EDGE('',*,*,#17092,.T.);
#24389=ORIENTED_EDGE('',*,*,#17093,.F.);
#24390=ORIENTED_EDGE('',*,*,#16458,.F.);
#24391=ORIENTED_EDGE('',*,*,#17095,.T.);
#24392=ORIENTED_EDGE('',*,*,#17096,.T.);
#24393=ORIENTED_EDGE('',*,*,#16466,.T.);
#24394=ORIENTED_EDGE('',*,*,#17096,.F.);
#24395=ORIENTED_EDGE('',*,*,#17097,.F.);
#24396=ORIENTED_EDGE('',*,*,#17095,.F.);
#24397=ORIENTED_EDGE('',*,*,#17098,.T.);
#24398=ORIENTED_EDGE('',*,*,#17099,.T.);
#24399=ORIENTED_EDGE('',*,*,#16463,.T.);
#24400=ORIENTED_EDGE('',*,*,#17099,.F.);
#24401=ORIENTED_EDGE('',*,*,#17100,.F.);
#24402=ORIENTED_EDGE('',*,*,#17098,.F.);
#24403=ORIENTED_EDGE('',*,*,#16854,.T.);
#24404=ORIENTED_EDGE('',*,*,#17101,.T.);
#24405=ORIENTED_EDGE('',*,*,#17102,.T.);
#24406=ORIENTED_EDGE('',*,*,#17101,.F.);
#24407=ORIENTED_EDGE('',*,*,#17102,.F.);
#24408=ORIENTED_EDGE('',*,*,#17103,.T.);
#24409=ORIENTED_EDGE('',*,*,#17104,.F.);
#24410=ORIENTED_EDGE('',*,*,#17103,.F.);
#24411=ORIENTED_EDGE('',*,*,#17026,.T.);
#24412=ORIENTED_EDGE('',*,*,#17030,.T.);
#24413=ORIENTED_EDGE('',*,*,#17033,.T.);
#24414=ORIENTED_EDGE('',*,*,#17036,.T.);
#24415=ORIENTED_EDGE('',*,*,#17039,.T.);
#24416=ORIENTED_EDGE('',*,*,#17042,.T.);
#24417=ORIENTED_EDGE('',*,*,#17045,.T.);
#24418=ORIENTED_EDGE('',*,*,#17048,.T.);
#24419=ORIENTED_EDGE('',*,*,#17100,.T.);
#24420=ORIENTED_EDGE('',*,*,#17105,.T.);
#24421=ORIENTED_EDGE('',*,*,#17104,.T.);
#24422=ORIENTED_EDGE('',*,*,#17105,.F.);
#24423=ORIENTED_EDGE('',*,*,#16895,.T.);
#24424=ORIENTED_EDGE('',*,*,#17106,.T.);
#24425=ORIENTED_EDGE('',*,*,#17107,.T.);
#24426=ORIENTED_EDGE('',*,*,#17106,.F.);
#24427=ORIENTED_EDGE('',*,*,#17108,.F.);
#24428=ORIENTED_EDGE('',*,*,#17109,.T.);
#24429=ORIENTED_EDGE('',*,*,#17107,.F.);
#24430=ORIENTED_EDGE('',*,*,#17109,.F.);
#24431=ORIENTED_EDGE('',*,*,#17097,.T.);
#24432=ORIENTED_EDGE('',*,*,#17110,.T.);
#24433=ORIENTED_EDGE('',*,*,#17108,.T.);
#24434=ORIENTED_EDGE('',*,*,#17110,.F.);
#24435=ORIENTED_EDGE('',*,*,#16802,.T.);
#24436=ORIENTED_EDGE('',*,*,#16834,.T.);
#24437=ORIENTED_EDGE('',*,*,#17111,.T.);
#24438=ORIENTED_EDGE('',*,*,#17112,.T.);
#24439=ORIENTED_EDGE('',*,*,#16921,.T.);
#24440=ORIENTED_EDGE('',*,*,#16904,.T.);
#24441=ORIENTED_EDGE('',*,*,#16661,.T.);
#24442=ORIENTED_EDGE('',*,*,#16944,.T.);
#24443=ORIENTED_EDGE('',*,*,#17113,.T.);
#24444=ORIENTED_EDGE('',*,*,#16836,.T.);
#24445=ORIENTED_EDGE('',*,*,#17114,.T.);
#24446=ORIENTED_EDGE('',*,*,#16837,.T.);
#24447=ORIENTED_EDGE('',*,*,#17113,.F.);
#24448=ORIENTED_EDGE('',*,*,#16945,.T.);
#24449=ORIENTED_EDGE('',*,*,#17115,.T.);
#24450=ORIENTED_EDGE('',*,*,#16838,.T.);
#24451=ORIENTED_EDGE('',*,*,#17114,.F.);
#24452=ORIENTED_EDGE('',*,*,#17116,.T.);
#24453=ORIENTED_EDGE('',*,*,#16826,.T.);
#24454=ORIENTED_EDGE('',*,*,#16839,.T.);
#24455=ORIENTED_EDGE('',*,*,#17115,.F.);
#24456=ORIENTED_EDGE('',*,*,#16954,.T.);
#24457=ORIENTED_EDGE('',*,*,#17117,.T.);
#24458=ORIENTED_EDGE('',*,*,#16828,.T.);
#24459=ORIENTED_EDGE('',*,*,#16823,.F.);
#24460=ORIENTED_EDGE('',*,*,#16678,.T.);
#24461=ORIENTED_EDGE('',*,*,#16710,.T.);
#24462=ORIENTED_EDGE('',*,*,#17118,.T.);
#24463=ORIENTED_EDGE('',*,*,#16829,.T.);
#24464=ORIENTED_EDGE('',*,*,#17117,.F.);
#24465=ORIENTED_EDGE('',*,*,#16941,.T.);
#24466=ORIENTED_EDGE('',*,*,#16830,.T.);
#24467=ORIENTED_EDGE('',*,*,#17118,.F.);
#24468=ORIENTED_EDGE('',*,*,#16936,.T.);
#24469=ORIENTED_EDGE('',*,*,#16929,.T.);
#24470=ORIENTED_EDGE('',*,*,#17119,.T.);
#24471=ORIENTED_EDGE('',*,*,#16832,.T.);
#24472=ORIENTED_EDGE('',*,*,#16940,.F.);
#24473=ORIENTED_EDGE('',*,*,#16751,.T.);
#24474=ORIENTED_EDGE('',*,*,#16987,.T.);
#24475=ORIENTED_EDGE('',*,*,#16972,.T.);
#24476=ORIENTED_EDGE('',*,*,#16977,.T.);
#24477=ORIENTED_EDGE('',*,*,#17120,.T.);
#24478=ORIENTED_EDGE('',*,*,#17121,.F.);
#24479=ORIENTED_EDGE('',*,*,#17111,.F.);
#24480=ORIENTED_EDGE('',*,*,#16833,.T.);
#24481=ORIENTED_EDGE('',*,*,#17119,.F.);
#24482=ORIENTED_EDGE('',*,*,#17116,.F.);
#24483=ORIENTED_EDGE('',*,*,#16968,.F.);
#24484=ORIENTED_EDGE('',*,*,#17122,.F.);
#24485=ORIENTED_EDGE('',*,*,#16966,.F.);
#24486=ORIENTED_EDGE('',*,*,#16907,.T.);
#24487=ORIENTED_EDGE('',*,*,#17123,.F.);
#24488=ORIENTED_EDGE('',*,*,#16773,.F.);
#24489=ORIENTED_EDGE('',*,*,#17124,.T.);
#24490=ORIENTED_EDGE('',*,*,#16885,.T.);
#24491=ORIENTED_EDGE('',*,*,#16985,.F.);
#24492=ORIENTED_EDGE('',*,*,#16973,.T.);
#24493=ORIENTED_EDGE('',*,*,#16986,.T.);
#24494=ORIENTED_EDGE('',*,*,#16744,.T.);
#24495=ORIENTED_EDGE('',*,*,#16934,.T.);
#24496=ORIENTED_EDGE('',*,*,#17125,.T.);
#24497=ORIENTED_EDGE('',*,*,#16886,.T.);
#24498=ORIENTED_EDGE('',*,*,#17124,.F.);
#24499=ORIENTED_EDGE('',*,*,#16920,.T.);
#24500=ORIENTED_EDGE('',*,*,#16887,.T.);
#24501=ORIENTED_EDGE('',*,*,#17125,.F.);
#24502=ORIENTED_EDGE('',*,*,#16930,.T.);
#24503=ORIENTED_EDGE('',*,*,#16939,.T.);
#24504=ORIENTED_EDGE('',*,*,#16896,.T.);
#24505=ORIENTED_EDGE('',*,*,#16889,.T.);
#24506=ORIENTED_EDGE('',*,*,#16919,.F.);
#24507=ORIENTED_EDGE('',*,*,#16683,.T.);
#24508=ORIENTED_EDGE('',*,*,#17126,.T.);
#24509=ORIENTED_EDGE('',*,*,#16892,.T.);
#24510=ORIENTED_EDGE('',*,*,#16969,.F.);
#24511=ORIENTED_EDGE('',*,*,#16958,.T.);
#24512=ORIENTED_EDGE('',*,*,#17127,.T.);
#24513=ORIENTED_EDGE('',*,*,#16893,.T.);
#24514=ORIENTED_EDGE('',*,*,#17126,.F.);
#24515=ORIENTED_EDGE('',*,*,#17122,.T.);
#24516=ORIENTED_EDGE('',*,*,#16882,.T.);
#24517=ORIENTED_EDGE('',*,*,#16894,.T.);
#24518=ORIENTED_EDGE('',*,*,#17127,.F.);
#24519=ORIENTED_EDGE('',*,*,#16948,.T.);
#24520=ORIENTED_EDGE('',*,*,#17128,.T.);
#24521=ORIENTED_EDGE('',*,*,#17129,.T.);
#24522=ORIENTED_EDGE('',*,*,#17130,.T.);
#24523=ORIENTED_EDGE('',*,*,#16535,.T.);
#24524=ORIENTED_EDGE('',*,*,#17131,.T.);
#24525=ORIENTED_EDGE('',*,*,#17132,.T.);
#24526=ORIENTED_EDGE('',*,*,#17128,.F.);
#24527=ORIENTED_EDGE('',*,*,#16534,.T.);
#24528=ORIENTED_EDGE('',*,*,#17133,.T.);
#24529=ORIENTED_EDGE('',*,*,#17134,.T.);
#24530=ORIENTED_EDGE('',*,*,#17131,.F.);
#24531=ORIENTED_EDGE('',*,*,#16533,.T.);
#24532=ORIENTED_EDGE('',*,*,#17087,.T.);
#24533=ORIENTED_EDGE('',*,*,#17135,.T.);
#24534=ORIENTED_EDGE('',*,*,#17133,.F.);
#24535=ORIENTED_EDGE('',*,*,#16532,.T.);
#24536=ORIENTED_EDGE('',*,*,#17136,.T.);
#24537=ORIENTED_EDGE('',*,*,#17137,.T.);
#24538=ORIENTED_EDGE('',*,*,#16530,.F.);
#24539=ORIENTED_EDGE('',*,*,#16538,.T.);
#24540=ORIENTED_EDGE('',*,*,#17138,.T.);
#24541=ORIENTED_EDGE('',*,*,#17139,.T.);
#24542=ORIENTED_EDGE('',*,*,#17136,.F.);
#24543=ORIENTED_EDGE('',*,*,#16537,.T.);
#24544=ORIENTED_EDGE('',*,*,#17130,.F.);
#24545=ORIENTED_EDGE('',*,*,#17140,.T.);
#24546=ORIENTED_EDGE('',*,*,#17138,.F.);
#24547=ORIENTED_EDGE('',*,*,#16536,.T.);
#24548=ORIENTED_EDGE('',*,*,#17137,.F.);
#24549=ORIENTED_EDGE('',*,*,#17141,.T.);
#24550=ORIENTED_EDGE('',*,*,#17142,.F.);
#24551=ORIENTED_EDGE('',*,*,#16481,.T.);
#24552=ORIENTED_EDGE('',*,*,#17139,.F.);
#24553=ORIENTED_EDGE('',*,*,#17143,.F.);
#24554=ORIENTED_EDGE('',*,*,#17144,.F.);
#24555=ORIENTED_EDGE('',*,*,#17141,.F.);
#24556=ORIENTED_EDGE('',*,*,#17140,.F.);
#24557=ORIENTED_EDGE('',*,*,#17145,.T.);
#24558=ORIENTED_EDGE('',*,*,#17146,.F.);
#24559=ORIENTED_EDGE('',*,*,#17143,.T.);
#24560=ORIENTED_EDGE('',*,*,#17129,.F.);
#24561=ORIENTED_EDGE('',*,*,#17147,.F.);
#24562=ORIENTED_EDGE('',*,*,#17148,.F.);
#24563=ORIENTED_EDGE('',*,*,#17145,.F.);
#24564=ORIENTED_EDGE('',*,*,#16906,.T.);
#24565=ORIENTED_EDGE('',*,*,#16922,.T.);
#24566=ORIENTED_EDGE('',*,*,#17112,.F.);
#24567=ORIENTED_EDGE('',*,*,#17121,.T.);
#24568=ORIENTED_EDGE('',*,*,#17120,.F.);
#24569=ORIENTED_EDGE('',*,*,#16976,.T.);
#24570=ORIENTED_EDGE('',*,*,#16594,.T.);
#24571=ORIENTED_EDGE('',*,*,#16914,.T.);
#24572=ORIENTED_EDGE('',*,*,#16774,.T.);
#24573=ORIENTED_EDGE('',*,*,#17123,.T.);
#24574=ORIENTED_EDGE('',*,*,#16478,.T.);
#24575=ORIENTED_EDGE('',*,*,#17142,.T.);
#24576=ORIENTED_EDGE('',*,*,#17149,.T.);
#24577=ORIENTED_EDGE('',*,*,#16756,.T.);
#24578=ORIENTED_EDGE('',*,*,#17150,.T.);
#24579=ORIENTED_EDGE('',*,*,#17151,.T.);
#24580=ORIENTED_EDGE('',*,*,#16488,.F.);
#24581=ORIENTED_EDGE('',*,*,#16762,.T.);
#24582=ORIENTED_EDGE('',*,*,#17150,.F.);
#24583=ORIENTED_EDGE('',*,*,#16761,.T.);
#24584=ORIENTED_EDGE('',*,*,#17152,.T.);
#24585=ORIENTED_EDGE('',*,*,#17153,.T.);
#24586=ORIENTED_EDGE('',*,*,#17154,.T.);
#24587=ORIENTED_EDGE('',*,*,#17155,.T.);
#24588=ORIENTED_EDGE('',*,*,#17152,.F.);
#24589=ORIENTED_EDGE('',*,*,#16760,.T.);
#24590=ORIENTED_EDGE('',*,*,#17154,.F.);
#24591=ORIENTED_EDGE('',*,*,#16759,.T.);
#24592=ORIENTED_EDGE('',*,*,#17156,.T.);
#24593=ORIENTED_EDGE('',*,*,#17148,.T.);
#24594=ORIENTED_EDGE('',*,*,#17157,.T.);
#24595=ORIENTED_EDGE('',*,*,#17146,.T.);
#24596=ORIENTED_EDGE('',*,*,#17156,.F.);
#24597=ORIENTED_EDGE('',*,*,#16758,.T.);
#24598=ORIENTED_EDGE('',*,*,#17157,.F.);
#24599=ORIENTED_EDGE('',*,*,#16757,.T.);
#24600=ORIENTED_EDGE('',*,*,#17149,.F.);
#24601=ORIENTED_EDGE('',*,*,#17144,.T.);
#24602=ORIENTED_EDGE('',*,*,#17132,.F.);
#24603=ORIENTED_EDGE('',*,*,#17158,.T.);
#24604=ORIENTED_EDGE('',*,*,#17155,.F.);
#24605=ORIENTED_EDGE('',*,*,#17147,.T.);
#24606=ORIENTED_EDGE('',*,*,#17135,.F.);
#24607=ORIENTED_EDGE('',*,*,#17088,.T.);
#24608=ORIENTED_EDGE('',*,*,#17151,.F.);
#24609=ORIENTED_EDGE('',*,*,#17159,.T.);
#24610=ORIENTED_EDGE('',*,*,#17134,.F.);
#24611=ORIENTED_EDGE('',*,*,#17159,.F.);
#24612=ORIENTED_EDGE('',*,*,#17153,.F.);
#24613=ORIENTED_EDGE('',*,*,#17158,.F.);
#24614=ORIENTED_EDGE('',*,*,#17160,.F.);
#24615=ORIENTED_EDGE('',*,*,#17161,.T.);
#24616=ORIENTED_EDGE('',*,*,#17162,.T.);
#24617=ORIENTED_EDGE('',*,*,#17163,.T.);
#24618=ORIENTED_EDGE('',*,*,#17164,.F.);
#24619=ORIENTED_EDGE('',*,*,#17165,.T.);
#24620=ORIENTED_EDGE('',*,*,#17160,.T.);
#24621=ORIENTED_EDGE('',*,*,#17166,.T.);
#24622=ORIENTED_EDGE('',*,*,#17167,.F.);
#24623=ORIENTED_EDGE('',*,*,#17168,.T.);
#24624=ORIENTED_EDGE('',*,*,#17164,.T.);
#24625=ORIENTED_EDGE('',*,*,#17169,.T.);
#24626=ORIENTED_EDGE('',*,*,#17170,.F.);
#24627=ORIENTED_EDGE('',*,*,#17171,.T.);
#24628=ORIENTED_EDGE('',*,*,#17167,.T.);
#24629=ORIENTED_EDGE('',*,*,#17172,.T.);
#24630=ORIENTED_EDGE('',*,*,#17173,.F.);
#24631=ORIENTED_EDGE('',*,*,#17174,.T.);
#24632=ORIENTED_EDGE('',*,*,#17170,.T.);
#24633=ORIENTED_EDGE('',*,*,#17175,.T.);
#24634=ORIENTED_EDGE('',*,*,#17176,.F.);
#24635=ORIENTED_EDGE('',*,*,#17177,.T.);
#24636=ORIENTED_EDGE('',*,*,#17173,.T.);
#24637=ORIENTED_EDGE('',*,*,#17178,.T.);
#24638=ORIENTED_EDGE('',*,*,#17179,.F.);
#24639=ORIENTED_EDGE('',*,*,#17180,.T.);
#24640=ORIENTED_EDGE('',*,*,#17176,.T.);
#24641=ORIENTED_EDGE('',*,*,#17181,.T.);
#24642=ORIENTED_EDGE('',*,*,#17182,.F.);
#24643=ORIENTED_EDGE('',*,*,#17183,.T.);
#24644=ORIENTED_EDGE('',*,*,#17179,.T.);
#24645=ORIENTED_EDGE('',*,*,#17184,.T.);
#24646=ORIENTED_EDGE('',*,*,#17185,.F.);
#24647=ORIENTED_EDGE('',*,*,#17186,.T.);
#24648=ORIENTED_EDGE('',*,*,#17182,.T.);
#24649=ORIENTED_EDGE('',*,*,#17187,.T.);
#24650=ORIENTED_EDGE('',*,*,#17188,.F.);
#24651=ORIENTED_EDGE('',*,*,#17189,.T.);
#24652=ORIENTED_EDGE('',*,*,#17185,.T.);
#24653=ORIENTED_EDGE('',*,*,#17190,.T.);
#24654=ORIENTED_EDGE('',*,*,#17191,.F.);
#24655=ORIENTED_EDGE('',*,*,#17192,.T.);
#24656=ORIENTED_EDGE('',*,*,#17188,.T.);
#24657=ORIENTED_EDGE('',*,*,#17193,.T.);
#24658=ORIENTED_EDGE('',*,*,#17194,.F.);
#24659=ORIENTED_EDGE('',*,*,#17195,.T.);
#24660=ORIENTED_EDGE('',*,*,#17191,.T.);
#24661=ORIENTED_EDGE('',*,*,#17196,.T.);
#24662=ORIENTED_EDGE('',*,*,#17197,.F.);
#24663=ORIENTED_EDGE('',*,*,#17198,.T.);
#24664=ORIENTED_EDGE('',*,*,#17194,.T.);
#24665=ORIENTED_EDGE('',*,*,#17199,.T.);
#24666=ORIENTED_EDGE('',*,*,#17200,.F.);
#24667=ORIENTED_EDGE('',*,*,#17201,.T.);
#24668=ORIENTED_EDGE('',*,*,#17197,.T.);
#24669=ORIENTED_EDGE('',*,*,#17202,.T.);
#24670=ORIENTED_EDGE('',*,*,#17203,.F.);
#24671=ORIENTED_EDGE('',*,*,#17204,.F.);
#24672=ORIENTED_EDGE('',*,*,#17205,.T.);
#24673=ORIENTED_EDGE('',*,*,#17200,.T.);
#24674=ORIENTED_EDGE('',*,*,#17206,.T.);
#24675=ORIENTED_EDGE('',*,*,#17207,.F.);
#24676=ORIENTED_EDGE('',*,*,#17208,.T.);
#24677=ORIENTED_EDGE('',*,*,#17209,.F.);
#24678=ORIENTED_EDGE('',*,*,#17210,.F.);
#24679=ORIENTED_EDGE('',*,*,#17211,.F.);
#24680=ORIENTED_EDGE('',*,*,#17212,.T.);
#24681=ORIENTED_EDGE('',*,*,#17207,.T.);
#24682=ORIENTED_EDGE('',*,*,#17213,.F.);
#24683=ORIENTED_EDGE('',*,*,#17214,.F.);
#24684=ORIENTED_EDGE('',*,*,#17215,.T.);
#24685=ORIENTED_EDGE('',*,*,#17211,.T.);
#24686=ORIENTED_EDGE('',*,*,#17216,.F.);
#24687=ORIENTED_EDGE('',*,*,#17217,.F.);
#24688=ORIENTED_EDGE('',*,*,#17218,.T.);
#24689=ORIENTED_EDGE('',*,*,#17214,.T.);
#24690=ORIENTED_EDGE('',*,*,#17219,.F.);
#24691=ORIENTED_EDGE('',*,*,#17220,.F.);
#24692=ORIENTED_EDGE('',*,*,#17221,.T.);
#24693=ORIENTED_EDGE('',*,*,#17217,.T.);
#24694=ORIENTED_EDGE('',*,*,#17222,.F.);
#24695=ORIENTED_EDGE('',*,*,#17223,.F.);
#24696=ORIENTED_EDGE('',*,*,#17224,.T.);
#24697=ORIENTED_EDGE('',*,*,#17220,.T.);
#24698=ORIENTED_EDGE('',*,*,#17225,.F.);
#24699=ORIENTED_EDGE('',*,*,#17226,.F.);
#24700=ORIENTED_EDGE('',*,*,#17227,.T.);
#24701=ORIENTED_EDGE('',*,*,#17223,.T.);
#24702=ORIENTED_EDGE('',*,*,#17228,.F.);
#24703=ORIENTED_EDGE('',*,*,#17229,.F.);
#24704=ORIENTED_EDGE('',*,*,#17230,.T.);
#24705=ORIENTED_EDGE('',*,*,#17226,.T.);
#24706=ORIENTED_EDGE('',*,*,#17231,.F.);
#24707=ORIENTED_EDGE('',*,*,#17232,.F.);
#24708=ORIENTED_EDGE('',*,*,#17233,.T.);
#24709=ORIENTED_EDGE('',*,*,#17229,.T.);
#24710=ORIENTED_EDGE('',*,*,#17234,.F.);
#24711=ORIENTED_EDGE('',*,*,#17235,.F.);
#24712=ORIENTED_EDGE('',*,*,#17236,.T.);
#24713=ORIENTED_EDGE('',*,*,#17232,.T.);
#24714=ORIENTED_EDGE('',*,*,#17237,.F.);
#24715=ORIENTED_EDGE('',*,*,#17238,.F.);
#24716=ORIENTED_EDGE('',*,*,#17239,.T.);
#24717=ORIENTED_EDGE('',*,*,#17235,.T.);
#24718=ORIENTED_EDGE('',*,*,#17240,.F.);
#24719=ORIENTED_EDGE('',*,*,#17241,.F.);
#24720=ORIENTED_EDGE('',*,*,#17242,.T.);
#24721=ORIENTED_EDGE('',*,*,#17238,.T.);
#24722=ORIENTED_EDGE('',*,*,#17243,.F.);
#24723=ORIENTED_EDGE('',*,*,#17244,.F.);
#24724=ORIENTED_EDGE('',*,*,#17245,.T.);
#24725=ORIENTED_EDGE('',*,*,#17241,.T.);
#24726=ORIENTED_EDGE('',*,*,#17246,.F.);
#24727=ORIENTED_EDGE('',*,*,#17247,.F.);
#24728=ORIENTED_EDGE('',*,*,#17248,.T.);
#24729=ORIENTED_EDGE('',*,*,#17244,.T.);
#24730=ORIENTED_EDGE('',*,*,#17249,.F.);
#24731=ORIENTED_EDGE('',*,*,#17250,.F.);
#24732=ORIENTED_EDGE('',*,*,#17251,.T.);
#24733=ORIENTED_EDGE('',*,*,#17252,.T.);
#24734=ORIENTED_EDGE('',*,*,#17253,.F.);
#24735=ORIENTED_EDGE('',*,*,#17254,.F.);
#24736=ORIENTED_EDGE('',*,*,#17255,.T.);
#24737=ORIENTED_EDGE('',*,*,#17256,.T.);
#24738=ORIENTED_EDGE('',*,*,#17251,.F.);
#24739=ORIENTED_EDGE('',*,*,#17257,.F.);
#24740=ORIENTED_EDGE('',*,*,#17258,.T.);
#24741=ORIENTED_EDGE('',*,*,#17259,.T.);
#24742=ORIENTED_EDGE('',*,*,#17255,.F.);
#24743=ORIENTED_EDGE('',*,*,#17260,.F.);
#24744=ORIENTED_EDGE('',*,*,#17261,.T.);
#24745=ORIENTED_EDGE('',*,*,#17262,.T.);
#24746=ORIENTED_EDGE('',*,*,#17258,.F.);
#24747=ORIENTED_EDGE('',*,*,#17263,.F.);
#24748=ORIENTED_EDGE('',*,*,#17264,.T.);
#24749=ORIENTED_EDGE('',*,*,#17265,.T.);
#24750=ORIENTED_EDGE('',*,*,#17261,.F.);
#24751=ORIENTED_EDGE('',*,*,#17266,.F.);
#24752=ORIENTED_EDGE('',*,*,#17267,.T.);
#24753=ORIENTED_EDGE('',*,*,#17268,.T.);
#24754=ORIENTED_EDGE('',*,*,#17264,.F.);
#24755=ORIENTED_EDGE('',*,*,#17269,.F.);
#24756=ORIENTED_EDGE('',*,*,#17270,.T.);
#24757=ORIENTED_EDGE('',*,*,#17271,.T.);
#24758=ORIENTED_EDGE('',*,*,#17267,.F.);
#24759=ORIENTED_EDGE('',*,*,#17272,.F.);
#24760=ORIENTED_EDGE('',*,*,#17253,.T.);
#24761=ORIENTED_EDGE('',*,*,#17273,.T.);
#24762=ORIENTED_EDGE('',*,*,#17270,.F.);
#24763=ORIENTED_EDGE('',*,*,#17274,.F.);
#24764=ORIENTED_EDGE('',*,*,#17275,.T.);
#24765=ORIENTED_EDGE('',*,*,#17276,.T.);
#24766=ORIENTED_EDGE('',*,*,#17277,.F.);
#24767=ORIENTED_EDGE('',*,*,#17278,.F.);
#24768=ORIENTED_EDGE('',*,*,#17279,.T.);
#24769=ORIENTED_EDGE('',*,*,#17280,.T.);
#24770=ORIENTED_EDGE('',*,*,#17275,.F.);
#24771=ORIENTED_EDGE('',*,*,#17281,.F.);
#24772=ORIENTED_EDGE('',*,*,#17282,.T.);
#24773=ORIENTED_EDGE('',*,*,#17283,.T.);
#24774=ORIENTED_EDGE('',*,*,#17279,.F.);
#24775=ORIENTED_EDGE('',*,*,#17284,.F.);
#24776=ORIENTED_EDGE('',*,*,#17285,.T.);
#24777=ORIENTED_EDGE('',*,*,#17286,.T.);
#24778=ORIENTED_EDGE('',*,*,#17282,.F.);
#24779=ORIENTED_EDGE('',*,*,#17287,.F.);
#24780=ORIENTED_EDGE('',*,*,#17288,.T.);
#24781=ORIENTED_EDGE('',*,*,#17289,.T.);
#24782=ORIENTED_EDGE('',*,*,#17285,.F.);
#24783=ORIENTED_EDGE('',*,*,#17290,.F.);
#24784=ORIENTED_EDGE('',*,*,#17291,.T.);
#24785=ORIENTED_EDGE('',*,*,#17292,.T.);
#24786=ORIENTED_EDGE('',*,*,#17288,.F.);
#24787=ORIENTED_EDGE('',*,*,#17293,.F.);
#24788=ORIENTED_EDGE('',*,*,#17294,.T.);
#24789=ORIENTED_EDGE('',*,*,#17295,.T.);
#24790=ORIENTED_EDGE('',*,*,#17291,.F.);
#24791=ORIENTED_EDGE('',*,*,#17296,.F.);
#24792=ORIENTED_EDGE('',*,*,#17297,.T.);
#24793=ORIENTED_EDGE('',*,*,#17298,.T.);
#24794=ORIENTED_EDGE('',*,*,#17294,.F.);
#24795=ORIENTED_EDGE('',*,*,#17299,.F.);
#24796=ORIENTED_EDGE('',*,*,#17277,.T.);
#24797=ORIENTED_EDGE('',*,*,#17300,.T.);
#24798=ORIENTED_EDGE('',*,*,#17297,.F.);
#24799=ORIENTED_EDGE('',*,*,#17301,.F.);
#24800=ORIENTED_EDGE('',*,*,#17302,.T.);
#24801=ORIENTED_EDGE('',*,*,#17303,.T.);
#24802=ORIENTED_EDGE('',*,*,#17304,.F.);
#24803=ORIENTED_EDGE('',*,*,#17305,.F.);
#24804=ORIENTED_EDGE('',*,*,#17306,.T.);
#24805=ORIENTED_EDGE('',*,*,#17307,.T.);
#24806=ORIENTED_EDGE('',*,*,#17302,.F.);
#24807=ORIENTED_EDGE('',*,*,#17308,.F.);
#24808=ORIENTED_EDGE('',*,*,#17309,.T.);
#24809=ORIENTED_EDGE('',*,*,#17310,.T.);
#24810=ORIENTED_EDGE('',*,*,#17306,.F.);
#24811=ORIENTED_EDGE('',*,*,#17311,.F.);
#24812=ORIENTED_EDGE('',*,*,#17312,.T.);
#24813=ORIENTED_EDGE('',*,*,#17313,.T.);
#24814=ORIENTED_EDGE('',*,*,#17309,.F.);
#24815=ORIENTED_EDGE('',*,*,#17314,.F.);
#24816=ORIENTED_EDGE('',*,*,#17315,.T.);
#24817=ORIENTED_EDGE('',*,*,#17316,.T.);
#24818=ORIENTED_EDGE('',*,*,#17312,.F.);
#24819=ORIENTED_EDGE('',*,*,#17317,.F.);
#24820=ORIENTED_EDGE('',*,*,#17318,.T.);
#24821=ORIENTED_EDGE('',*,*,#17319,.T.);
#24822=ORIENTED_EDGE('',*,*,#17315,.F.);
#24823=ORIENTED_EDGE('',*,*,#17320,.F.);
#24824=ORIENTED_EDGE('',*,*,#17321,.T.);
#24825=ORIENTED_EDGE('',*,*,#17322,.T.);
#24826=ORIENTED_EDGE('',*,*,#17318,.F.);
#24827=ORIENTED_EDGE('',*,*,#17323,.F.);
#24828=ORIENTED_EDGE('',*,*,#17324,.T.);
#24829=ORIENTED_EDGE('',*,*,#17325,.T.);
#24830=ORIENTED_EDGE('',*,*,#17321,.F.);
#24831=ORIENTED_EDGE('',*,*,#17326,.F.);
#24832=ORIENTED_EDGE('',*,*,#17327,.T.);
#24833=ORIENTED_EDGE('',*,*,#17328,.T.);
#24834=ORIENTED_EDGE('',*,*,#17324,.F.);
#24835=ORIENTED_EDGE('',*,*,#17329,.F.);
#24836=ORIENTED_EDGE('',*,*,#17330,.T.);
#24837=ORIENTED_EDGE('',*,*,#17331,.T.);
#24838=ORIENTED_EDGE('',*,*,#17327,.F.);
#24839=ORIENTED_EDGE('',*,*,#17332,.F.);
#24840=ORIENTED_EDGE('',*,*,#17333,.T.);
#24841=ORIENTED_EDGE('',*,*,#17334,.T.);
#24842=ORIENTED_EDGE('',*,*,#17330,.F.);
#24843=ORIENTED_EDGE('',*,*,#17335,.F.);
#24844=ORIENTED_EDGE('',*,*,#17336,.T.);
#24845=ORIENTED_EDGE('',*,*,#17337,.T.);
#24846=ORIENTED_EDGE('',*,*,#17333,.F.);
#24847=ORIENTED_EDGE('',*,*,#17338,.F.);
#24848=ORIENTED_EDGE('',*,*,#17339,.T.);
#24849=ORIENTED_EDGE('',*,*,#17340,.T.);
#24850=ORIENTED_EDGE('',*,*,#17336,.F.);
#24851=ORIENTED_EDGE('',*,*,#17341,.F.);
#24852=ORIENTED_EDGE('',*,*,#17342,.T.);
#24853=ORIENTED_EDGE('',*,*,#17343,.T.);
#24854=ORIENTED_EDGE('',*,*,#17339,.F.);
#24855=ORIENTED_EDGE('',*,*,#17344,.F.);
#24856=ORIENTED_EDGE('',*,*,#17345,.T.);
#24857=ORIENTED_EDGE('',*,*,#17346,.T.);
#24858=ORIENTED_EDGE('',*,*,#17342,.F.);
#24859=ORIENTED_EDGE('',*,*,#17347,.F.);
#24860=ORIENTED_EDGE('',*,*,#17304,.T.);
#24861=ORIENTED_EDGE('',*,*,#17348,.T.);
#24862=ORIENTED_EDGE('',*,*,#17345,.F.);
#24863=ORIENTED_EDGE('',*,*,#17348,.F.);
#24864=ORIENTED_EDGE('',*,*,#17303,.F.);
#24865=ORIENTED_EDGE('',*,*,#17307,.F.);
#24866=ORIENTED_EDGE('',*,*,#17310,.F.);
#24867=ORIENTED_EDGE('',*,*,#17313,.F.);
#24868=ORIENTED_EDGE('',*,*,#17316,.F.);
#24869=ORIENTED_EDGE('',*,*,#17319,.F.);
#24870=ORIENTED_EDGE('',*,*,#17322,.F.);
#24871=ORIENTED_EDGE('',*,*,#17325,.F.);
#24872=ORIENTED_EDGE('',*,*,#17328,.F.);
#24873=ORIENTED_EDGE('',*,*,#17331,.F.);
#24874=ORIENTED_EDGE('',*,*,#17334,.F.);
#24875=ORIENTED_EDGE('',*,*,#17337,.F.);
#24876=ORIENTED_EDGE('',*,*,#17340,.F.);
#24877=ORIENTED_EDGE('',*,*,#17343,.F.);
#24878=ORIENTED_EDGE('',*,*,#17346,.F.);
#24879=ORIENTED_EDGE('',*,*,#17300,.F.);
#24880=ORIENTED_EDGE('',*,*,#17276,.F.);
#24881=ORIENTED_EDGE('',*,*,#17280,.F.);
#24882=ORIENTED_EDGE('',*,*,#17283,.F.);
#24883=ORIENTED_EDGE('',*,*,#17286,.F.);
#24884=ORIENTED_EDGE('',*,*,#17289,.F.);
#24885=ORIENTED_EDGE('',*,*,#17292,.F.);
#24886=ORIENTED_EDGE('',*,*,#17295,.F.);
#24887=ORIENTED_EDGE('',*,*,#17298,.F.);
#24888=ORIENTED_EDGE('',*,*,#17273,.F.);
#24889=ORIENTED_EDGE('',*,*,#17252,.F.);
#24890=ORIENTED_EDGE('',*,*,#17256,.F.);
#24891=ORIENTED_EDGE('',*,*,#17259,.F.);
#24892=ORIENTED_EDGE('',*,*,#17262,.F.);
#24893=ORIENTED_EDGE('',*,*,#17265,.F.);
#24894=ORIENTED_EDGE('',*,*,#17268,.F.);
#24895=ORIENTED_EDGE('',*,*,#17271,.F.);
#24896=ORIENTED_EDGE('',*,*,#17349,.F.);
#24897=ORIENTED_EDGE('',*,*,#17350,.T.);
#24898=ORIENTED_EDGE('',*,*,#17351,.T.);
#24899=ORIENTED_EDGE('',*,*,#17352,.F.);
#24900=ORIENTED_EDGE('',*,*,#17353,.F.);
#24901=ORIENTED_EDGE('',*,*,#17354,.T.);
#24902=ORIENTED_EDGE('',*,*,#17355,.T.);
#24903=ORIENTED_EDGE('',*,*,#17350,.F.);
#24904=ORIENTED_EDGE('',*,*,#17356,.F.);
#24905=ORIENTED_EDGE('',*,*,#17357,.T.);
#24906=ORIENTED_EDGE('',*,*,#17358,.T.);
#24907=ORIENTED_EDGE('',*,*,#17354,.F.);
#24908=ORIENTED_EDGE('',*,*,#17359,.F.);
#24909=ORIENTED_EDGE('',*,*,#17352,.T.);
#24910=ORIENTED_EDGE('',*,*,#17360,.T.);
#24911=ORIENTED_EDGE('',*,*,#17357,.F.);
#24912=ORIENTED_EDGE('',*,*,#17360,.F.);
#24913=ORIENTED_EDGE('',*,*,#17351,.F.);
#24914=ORIENTED_EDGE('',*,*,#17355,.F.);
#24915=ORIENTED_EDGE('',*,*,#17358,.F.);
#24916=ORIENTED_EDGE('',*,*,#17361,.F.);
#24917=ORIENTED_EDGE('',*,*,#17362,.T.);
#24918=ORIENTED_EDGE('',*,*,#17363,.T.);
#24919=ORIENTED_EDGE('',*,*,#17364,.F.);
#24920=ORIENTED_EDGE('',*,*,#17365,.F.);
#24921=ORIENTED_EDGE('',*,*,#17366,.T.);
#24922=ORIENTED_EDGE('',*,*,#17367,.T.);
#24923=ORIENTED_EDGE('',*,*,#17362,.F.);
#24924=ORIENTED_EDGE('',*,*,#17368,.F.);
#24925=ORIENTED_EDGE('',*,*,#17369,.T.);
#24926=ORIENTED_EDGE('',*,*,#17370,.T.);
#24927=ORIENTED_EDGE('',*,*,#17366,.F.);
#24928=ORIENTED_EDGE('',*,*,#17371,.F.);
#24929=ORIENTED_EDGE('',*,*,#17372,.T.);
#24930=ORIENTED_EDGE('',*,*,#17373,.T.);
#24931=ORIENTED_EDGE('',*,*,#17369,.F.);
#24932=ORIENTED_EDGE('',*,*,#17374,.F.);
#24933=ORIENTED_EDGE('',*,*,#17375,.T.);
#24934=ORIENTED_EDGE('',*,*,#17376,.T.);
#24935=ORIENTED_EDGE('',*,*,#17372,.F.);
#24936=ORIENTED_EDGE('',*,*,#17377,.F.);
#24937=ORIENTED_EDGE('',*,*,#17378,.T.);
#24938=ORIENTED_EDGE('',*,*,#17379,.T.);
#24939=ORIENTED_EDGE('',*,*,#17375,.F.);
#24940=ORIENTED_EDGE('',*,*,#17380,.F.);
#24941=ORIENTED_EDGE('',*,*,#17381,.T.);
#24942=ORIENTED_EDGE('',*,*,#17382,.T.);
#24943=ORIENTED_EDGE('',*,*,#17378,.F.);
#24944=ORIENTED_EDGE('',*,*,#17383,.F.);
#24945=ORIENTED_EDGE('',*,*,#17364,.T.);
#24946=ORIENTED_EDGE('',*,*,#17384,.T.);
#24947=ORIENTED_EDGE('',*,*,#17381,.F.);
#24948=ORIENTED_EDGE('',*,*,#17385,.F.);
#24949=ORIENTED_EDGE('',*,*,#17386,.T.);
#24950=ORIENTED_EDGE('',*,*,#17387,.T.);
#24951=ORIENTED_EDGE('',*,*,#17388,.F.);
#24952=ORIENTED_EDGE('',*,*,#17389,.F.);
#24953=ORIENTED_EDGE('',*,*,#17390,.T.);
#24954=ORIENTED_EDGE('',*,*,#17391,.T.);
#24955=ORIENTED_EDGE('',*,*,#17386,.F.);
#24956=ORIENTED_EDGE('',*,*,#17392,.F.);
#24957=ORIENTED_EDGE('',*,*,#17393,.T.);
#24958=ORIENTED_EDGE('',*,*,#17394,.T.);
#24959=ORIENTED_EDGE('',*,*,#17390,.F.);
#24960=ORIENTED_EDGE('',*,*,#17395,.F.);
#24961=ORIENTED_EDGE('',*,*,#17396,.T.);
#24962=ORIENTED_EDGE('',*,*,#17397,.T.);
#24963=ORIENTED_EDGE('',*,*,#17393,.F.);
#24964=ORIENTED_EDGE('',*,*,#17398,.F.);
#24965=ORIENTED_EDGE('',*,*,#17399,.T.);
#24966=ORIENTED_EDGE('',*,*,#17400,.T.);
#24967=ORIENTED_EDGE('',*,*,#17396,.F.);
#24968=ORIENTED_EDGE('',*,*,#17401,.F.);
#24969=ORIENTED_EDGE('',*,*,#17402,.T.);
#24970=ORIENTED_EDGE('',*,*,#17403,.T.);
#24971=ORIENTED_EDGE('',*,*,#17399,.F.);
#24972=ORIENTED_EDGE('',*,*,#17404,.F.);
#24973=ORIENTED_EDGE('',*,*,#17405,.T.);
#24974=ORIENTED_EDGE('',*,*,#17406,.T.);
#24975=ORIENTED_EDGE('',*,*,#17402,.F.);
#24976=ORIENTED_EDGE('',*,*,#17407,.F.);
#24977=ORIENTED_EDGE('',*,*,#17408,.T.);
#24978=ORIENTED_EDGE('',*,*,#17409,.T.);
#24979=ORIENTED_EDGE('',*,*,#17405,.F.);
#24980=ORIENTED_EDGE('',*,*,#17410,.F.);
#24981=ORIENTED_EDGE('',*,*,#17388,.T.);
#24982=ORIENTED_EDGE('',*,*,#17411,.T.);
#24983=ORIENTED_EDGE('',*,*,#17408,.F.);
#24984=ORIENTED_EDGE('',*,*,#17412,.F.);
#24985=ORIENTED_EDGE('',*,*,#17413,.T.);
#24986=ORIENTED_EDGE('',*,*,#17414,.T.);
#24987=ORIENTED_EDGE('',*,*,#17415,.F.);
#24988=ORIENTED_EDGE('',*,*,#17416,.F.);
#24989=ORIENTED_EDGE('',*,*,#17417,.T.);
#24990=ORIENTED_EDGE('',*,*,#17418,.T.);
#24991=ORIENTED_EDGE('',*,*,#17413,.F.);
#24992=ORIENTED_EDGE('',*,*,#17419,.F.);
#24993=ORIENTED_EDGE('',*,*,#17420,.T.);
#24994=ORIENTED_EDGE('',*,*,#17421,.T.);
#24995=ORIENTED_EDGE('',*,*,#17417,.F.);
#24996=ORIENTED_EDGE('',*,*,#17422,.F.);
#24997=ORIENTED_EDGE('',*,*,#17423,.T.);
#24998=ORIENTED_EDGE('',*,*,#17424,.T.);
#24999=ORIENTED_EDGE('',*,*,#17420,.F.);
#25000=ORIENTED_EDGE('',*,*,#17425,.F.);
#25001=ORIENTED_EDGE('',*,*,#17426,.T.);
#25002=ORIENTED_EDGE('',*,*,#17427,.T.);
#25003=ORIENTED_EDGE('',*,*,#17423,.F.);
#25004=ORIENTED_EDGE('',*,*,#17428,.F.);
#25005=ORIENTED_EDGE('',*,*,#17429,.T.);
#25006=ORIENTED_EDGE('',*,*,#17430,.T.);
#25007=ORIENTED_EDGE('',*,*,#17426,.F.);
#25008=ORIENTED_EDGE('',*,*,#17431,.F.);
#25009=ORIENTED_EDGE('',*,*,#17432,.T.);
#25010=ORIENTED_EDGE('',*,*,#17433,.T.);
#25011=ORIENTED_EDGE('',*,*,#17429,.F.);
#25012=ORIENTED_EDGE('',*,*,#17434,.F.);
#25013=ORIENTED_EDGE('',*,*,#17435,.T.);
#25014=ORIENTED_EDGE('',*,*,#17436,.T.);
#25015=ORIENTED_EDGE('',*,*,#17432,.F.);
#25016=ORIENTED_EDGE('',*,*,#17437,.F.);
#25017=ORIENTED_EDGE('',*,*,#17438,.T.);
#25018=ORIENTED_EDGE('',*,*,#17439,.T.);
#25019=ORIENTED_EDGE('',*,*,#17435,.F.);
#25020=ORIENTED_EDGE('',*,*,#17440,.F.);
#25021=ORIENTED_EDGE('',*,*,#17441,.T.);
#25022=ORIENTED_EDGE('',*,*,#17442,.T.);
#25023=ORIENTED_EDGE('',*,*,#17438,.F.);
#25024=ORIENTED_EDGE('',*,*,#17443,.F.);
#25025=ORIENTED_EDGE('',*,*,#17444,.T.);
#25026=ORIENTED_EDGE('',*,*,#17445,.T.);
#25027=ORIENTED_EDGE('',*,*,#17441,.F.);
#25028=ORIENTED_EDGE('',*,*,#17446,.F.);
#25029=ORIENTED_EDGE('',*,*,#17447,.T.);
#25030=ORIENTED_EDGE('',*,*,#17448,.T.);
#25031=ORIENTED_EDGE('',*,*,#17444,.F.);
#25032=ORIENTED_EDGE('',*,*,#17449,.F.);
#25033=ORIENTED_EDGE('',*,*,#17450,.T.);
#25034=ORIENTED_EDGE('',*,*,#17451,.T.);
#25035=ORIENTED_EDGE('',*,*,#17447,.F.);
#25036=ORIENTED_EDGE('',*,*,#17452,.F.);
#25037=ORIENTED_EDGE('',*,*,#17453,.T.);
#25038=ORIENTED_EDGE('',*,*,#17454,.T.);
#25039=ORIENTED_EDGE('',*,*,#17450,.F.);
#25040=ORIENTED_EDGE('',*,*,#17455,.F.);
#25041=ORIENTED_EDGE('',*,*,#17456,.T.);
#25042=ORIENTED_EDGE('',*,*,#17457,.T.);
#25043=ORIENTED_EDGE('',*,*,#17453,.F.);
#25044=ORIENTED_EDGE('',*,*,#17458,.F.);
#25045=ORIENTED_EDGE('',*,*,#17415,.T.);
#25046=ORIENTED_EDGE('',*,*,#17459,.T.);
#25047=ORIENTED_EDGE('',*,*,#17456,.F.);
#25048=ORIENTED_EDGE('',*,*,#17459,.F.);
#25049=ORIENTED_EDGE('',*,*,#17414,.F.);
#25050=ORIENTED_EDGE('',*,*,#17418,.F.);
#25051=ORIENTED_EDGE('',*,*,#17421,.F.);
#25052=ORIENTED_EDGE('',*,*,#17424,.F.);
#25053=ORIENTED_EDGE('',*,*,#17427,.F.);
#25054=ORIENTED_EDGE('',*,*,#17430,.F.);
#25055=ORIENTED_EDGE('',*,*,#17433,.F.);
#25056=ORIENTED_EDGE('',*,*,#17436,.F.);
#25057=ORIENTED_EDGE('',*,*,#17439,.F.);
#25058=ORIENTED_EDGE('',*,*,#17442,.F.);
#25059=ORIENTED_EDGE('',*,*,#17445,.F.);
#25060=ORIENTED_EDGE('',*,*,#17448,.F.);
#25061=ORIENTED_EDGE('',*,*,#17451,.F.);
#25062=ORIENTED_EDGE('',*,*,#17454,.F.);
#25063=ORIENTED_EDGE('',*,*,#17457,.F.);
#25064=ORIENTED_EDGE('',*,*,#17411,.F.);
#25065=ORIENTED_EDGE('',*,*,#17387,.F.);
#25066=ORIENTED_EDGE('',*,*,#17391,.F.);
#25067=ORIENTED_EDGE('',*,*,#17394,.F.);
#25068=ORIENTED_EDGE('',*,*,#17397,.F.);
#25069=ORIENTED_EDGE('',*,*,#17400,.F.);
#25070=ORIENTED_EDGE('',*,*,#17403,.F.);
#25071=ORIENTED_EDGE('',*,*,#17406,.F.);
#25072=ORIENTED_EDGE('',*,*,#17409,.F.);
#25073=ORIENTED_EDGE('',*,*,#17384,.F.);
#25074=ORIENTED_EDGE('',*,*,#17363,.F.);
#25075=ORIENTED_EDGE('',*,*,#17367,.F.);
#25076=ORIENTED_EDGE('',*,*,#17370,.F.);
#25077=ORIENTED_EDGE('',*,*,#17373,.F.);
#25078=ORIENTED_EDGE('',*,*,#17376,.F.);
#25079=ORIENTED_EDGE('',*,*,#17379,.F.);
#25080=ORIENTED_EDGE('',*,*,#17382,.F.);
#25081=ORIENTED_EDGE('',*,*,#17385,.T.);
#25082=ORIENTED_EDGE('',*,*,#17410,.T.);
#25083=ORIENTED_EDGE('',*,*,#17407,.T.);
#25084=ORIENTED_EDGE('',*,*,#17404,.T.);
#25085=ORIENTED_EDGE('',*,*,#17401,.T.);
#25086=ORIENTED_EDGE('',*,*,#17398,.T.);
#25087=ORIENTED_EDGE('',*,*,#17395,.T.);
#25088=ORIENTED_EDGE('',*,*,#17392,.T.);
#25089=ORIENTED_EDGE('',*,*,#17389,.T.);
#25090=ORIENTED_EDGE('',*,*,#17361,.T.);
#25091=ORIENTED_EDGE('',*,*,#17383,.T.);
#25092=ORIENTED_EDGE('',*,*,#17380,.T.);
#25093=ORIENTED_EDGE('',*,*,#17377,.T.);
#25094=ORIENTED_EDGE('',*,*,#17374,.T.);
#25095=ORIENTED_EDGE('',*,*,#17371,.T.);
#25096=ORIENTED_EDGE('',*,*,#17368,.T.);
#25097=ORIENTED_EDGE('',*,*,#17365,.T.);
#25098=ORIENTED_EDGE('',*,*,#17274,.T.);
#25099=ORIENTED_EDGE('',*,*,#17299,.T.);
#25100=ORIENTED_EDGE('',*,*,#17296,.T.);
#25101=ORIENTED_EDGE('',*,*,#17293,.T.);
#25102=ORIENTED_EDGE('',*,*,#17290,.T.);
#25103=ORIENTED_EDGE('',*,*,#17287,.T.);
#25104=ORIENTED_EDGE('',*,*,#17284,.T.);
#25105=ORIENTED_EDGE('',*,*,#17281,.T.);
#25106=ORIENTED_EDGE('',*,*,#17278,.T.);
#25107=ORIENTED_EDGE('',*,*,#17250,.T.);
#25108=ORIENTED_EDGE('',*,*,#17272,.T.);
#25109=ORIENTED_EDGE('',*,*,#17269,.T.);
#25110=ORIENTED_EDGE('',*,*,#17266,.T.);
#25111=ORIENTED_EDGE('',*,*,#17263,.T.);
#25112=ORIENTED_EDGE('',*,*,#17260,.T.);
#25113=ORIENTED_EDGE('',*,*,#17257,.T.);
#25114=ORIENTED_EDGE('',*,*,#17254,.T.);
#25115=ORIENTED_EDGE('',*,*,#17209,.T.);
#25116=ORIENTED_EDGE('',*,*,#17460,.T.);
#25117=ORIENTED_EDGE('',*,*,#17461,.F.);
#25118=ORIENTED_EDGE('',*,*,#17462,.F.);
#25119=ORIENTED_EDGE('',*,*,#17463,.T.);
#25120=ORIENTED_EDGE('',*,*,#17463,.F.);
#25121=ORIENTED_EDGE('',*,*,#17464,.F.);
#25122=ORIENTED_EDGE('',*,*,#17206,.F.);
#25123=ORIENTED_EDGE('',*,*,#17202,.F.);
#25124=ORIENTED_EDGE('',*,*,#17199,.F.);
#25125=ORIENTED_EDGE('',*,*,#17196,.F.);
#25126=ORIENTED_EDGE('',*,*,#17193,.F.);
#25127=ORIENTED_EDGE('',*,*,#17190,.F.);
#25128=ORIENTED_EDGE('',*,*,#17187,.F.);
#25129=ORIENTED_EDGE('',*,*,#17184,.F.);
#25130=ORIENTED_EDGE('',*,*,#17181,.F.);
#25131=ORIENTED_EDGE('',*,*,#17178,.F.);
#25132=ORIENTED_EDGE('',*,*,#17175,.F.);
#25133=ORIENTED_EDGE('',*,*,#17172,.F.);
#25134=ORIENTED_EDGE('',*,*,#17169,.F.);
#25135=ORIENTED_EDGE('',*,*,#17166,.F.);
#25136=ORIENTED_EDGE('',*,*,#17163,.F.);
#25137=ORIENTED_EDGE('',*,*,#17465,.F.);
#25138=ORIENTED_EDGE('',*,*,#17466,.T.);
#25139=ORIENTED_EDGE('',*,*,#17249,.T.);
#25140=ORIENTED_EDGE('',*,*,#17246,.T.);
#25141=ORIENTED_EDGE('',*,*,#17243,.T.);
#25142=ORIENTED_EDGE('',*,*,#17240,.T.);
#25143=ORIENTED_EDGE('',*,*,#17237,.T.);
#25144=ORIENTED_EDGE('',*,*,#17234,.T.);
#25145=ORIENTED_EDGE('',*,*,#17231,.T.);
#25146=ORIENTED_EDGE('',*,*,#17228,.T.);
#25147=ORIENTED_EDGE('',*,*,#17225,.T.);
#25148=ORIENTED_EDGE('',*,*,#17222,.T.);
#25149=ORIENTED_EDGE('',*,*,#17219,.T.);
#25150=ORIENTED_EDGE('',*,*,#17216,.T.);
#25151=ORIENTED_EDGE('',*,*,#17213,.T.);
#25152=ORIENTED_EDGE('',*,*,#17210,.T.);
#25153=ORIENTED_EDGE('',*,*,#17467,.T.);
#25154=ORIENTED_EDGE('',*,*,#17468,.T.);
#25155=ORIENTED_EDGE('',*,*,#17469,.T.);
#25156=ORIENTED_EDGE('',*,*,#17470,.T.);
#25157=ORIENTED_EDGE('',*,*,#17465,.T.);
#25158=ORIENTED_EDGE('',*,*,#17247,.T.);
#25159=ORIENTED_EDGE('',*,*,#17466,.F.);
#25160=ORIENTED_EDGE('',*,*,#17470,.F.);
#25161=ORIENTED_EDGE('',*,*,#17471,.T.);
#25162=ORIENTED_EDGE('',*,*,#17460,.F.);
#25163=ORIENTED_EDGE('',*,*,#17208,.F.);
#25164=ORIENTED_EDGE('',*,*,#17212,.F.);
#25165=ORIENTED_EDGE('',*,*,#17215,.F.);
#25166=ORIENTED_EDGE('',*,*,#17218,.F.);
#25167=ORIENTED_EDGE('',*,*,#17221,.F.);
#25168=ORIENTED_EDGE('',*,*,#17224,.F.);
#25169=ORIENTED_EDGE('',*,*,#17227,.F.);
#25170=ORIENTED_EDGE('',*,*,#17230,.F.);
#25171=ORIENTED_EDGE('',*,*,#17233,.F.);
#25172=ORIENTED_EDGE('',*,*,#17236,.F.);
#25173=ORIENTED_EDGE('',*,*,#17239,.F.);
#25174=ORIENTED_EDGE('',*,*,#17242,.F.);
#25175=ORIENTED_EDGE('',*,*,#17245,.F.);
#25176=ORIENTED_EDGE('',*,*,#17248,.F.);
#25177=ORIENTED_EDGE('',*,*,#17471,.F.);
#25178=ORIENTED_EDGE('',*,*,#17469,.F.);
#25179=ORIENTED_EDGE('',*,*,#17161,.F.);
#25180=ORIENTED_EDGE('',*,*,#17165,.F.);
#25181=ORIENTED_EDGE('',*,*,#17168,.F.);
#25182=ORIENTED_EDGE('',*,*,#17171,.F.);
#25183=ORIENTED_EDGE('',*,*,#17174,.F.);
#25184=ORIENTED_EDGE('',*,*,#17177,.F.);
#25185=ORIENTED_EDGE('',*,*,#17180,.F.);
#25186=ORIENTED_EDGE('',*,*,#17183,.F.);
#25187=ORIENTED_EDGE('',*,*,#17186,.F.);
#25188=ORIENTED_EDGE('',*,*,#17189,.F.);
#25189=ORIENTED_EDGE('',*,*,#17192,.F.);
#25190=ORIENTED_EDGE('',*,*,#17195,.F.);
#25191=ORIENTED_EDGE('',*,*,#17198,.F.);
#25192=ORIENTED_EDGE('',*,*,#17201,.F.);
#25193=ORIENTED_EDGE('',*,*,#17205,.F.);
#25194=ORIENTED_EDGE('',*,*,#17472,.T.);
#25195=ORIENTED_EDGE('',*,*,#17473,.T.);
#25196=ORIENTED_EDGE('',*,*,#17461,.T.);
#25197=ORIENTED_EDGE('',*,*,#17204,.T.);
#25198=ORIENTED_EDGE('',*,*,#17474,.T.);
#25199=ORIENTED_EDGE('',*,*,#17462,.T.);
#25200=ORIENTED_EDGE('',*,*,#17473,.F.);
#25201=ORIENTED_EDGE('',*,*,#17475,.F.);
#25202=ORIENTED_EDGE('',*,*,#17476,.F.);
#25203=ORIENTED_EDGE('',*,*,#17477,.F.);
#25204=ORIENTED_EDGE('',*,*,#17478,.F.);
#25205=ORIENTED_EDGE('',*,*,#17479,.F.);
#25206=ORIENTED_EDGE('',*,*,#17480,.F.);
#25207=ORIENTED_EDGE('',*,*,#17472,.F.);
#25208=ORIENTED_EDGE('',*,*,#17203,.T.);
#25209=ORIENTED_EDGE('',*,*,#17464,.T.);
#25210=ORIENTED_EDGE('',*,*,#17474,.F.);
#25211=ORIENTED_EDGE('',*,*,#17481,.F.);
#25212=ORIENTED_EDGE('',*,*,#17482,.F.);
#25213=ORIENTED_EDGE('',*,*,#17483,.F.);
#25214=ORIENTED_EDGE('',*,*,#17484,.F.);
#25215=ORIENTED_EDGE('',*,*,#17485,.F.);
#25216=ORIENTED_EDGE('',*,*,#17486,.T.);
#25217=ORIENTED_EDGE('',*,*,#17487,.F.);
#25218=ORIENTED_EDGE('',*,*,#17486,.F.);
#25219=ORIENTED_EDGE('',*,*,#17488,.F.);
#25220=ORIENTED_EDGE('',*,*,#17489,.F.);
#25221=ORIENTED_EDGE('',*,*,#17484,.T.);
#25222=ORIENTED_EDGE('',*,*,#17490,.F.);
#25223=ORIENTED_EDGE('',*,*,#17479,.T.);
#25224=ORIENTED_EDGE('',*,*,#17491,.T.);
#25225=ORIENTED_EDGE('',*,*,#17483,.T.);
#25226=ORIENTED_EDGE('',*,*,#17492,.F.);
#25227=ORIENTED_EDGE('',*,*,#17480,.T.);
#25228=ORIENTED_EDGE('',*,*,#17490,.T.);
#25229=ORIENTED_EDGE('',*,*,#17482,.T.);
#25230=ORIENTED_EDGE('',*,*,#17493,.F.);
#25231=ORIENTED_EDGE('',*,*,#17475,.T.);
#25232=ORIENTED_EDGE('',*,*,#17492,.T.);
#25233=ORIENTED_EDGE('',*,*,#17481,.T.);
#25234=ORIENTED_EDGE('',*,*,#17494,.F.);
#25235=ORIENTED_EDGE('',*,*,#17476,.T.);
#25236=ORIENTED_EDGE('',*,*,#17493,.T.);
#25237=ORIENTED_EDGE('',*,*,#17489,.T.);
#25238=ORIENTED_EDGE('',*,*,#17495,.F.);
#25239=ORIENTED_EDGE('',*,*,#17477,.T.);
#25240=ORIENTED_EDGE('',*,*,#17494,.T.);
#25241=ORIENTED_EDGE('',*,*,#17488,.T.);
#25242=ORIENTED_EDGE('',*,*,#17485,.T.);
#25243=ORIENTED_EDGE('',*,*,#17491,.F.);
#25244=ORIENTED_EDGE('',*,*,#17478,.T.);
#25245=ORIENTED_EDGE('',*,*,#17495,.T.);
#25246=ORIENTED_EDGE('',*,*,#17487,.T.);
#25247=ORIENTED_EDGE('',*,*,#17412,.T.);
#25248=ORIENTED_EDGE('',*,*,#17458,.T.);
#25249=ORIENTED_EDGE('',*,*,#17455,.T.);
#25250=ORIENTED_EDGE('',*,*,#17452,.T.);
#25251=ORIENTED_EDGE('',*,*,#17449,.T.);
#25252=ORIENTED_EDGE('',*,*,#17446,.T.);
#25253=ORIENTED_EDGE('',*,*,#17443,.T.);
#25254=ORIENTED_EDGE('',*,*,#17440,.T.);
#25255=ORIENTED_EDGE('',*,*,#17437,.T.);
#25256=ORIENTED_EDGE('',*,*,#17434,.T.);
#25257=ORIENTED_EDGE('',*,*,#17431,.T.);
#25258=ORIENTED_EDGE('',*,*,#17428,.T.);
#25259=ORIENTED_EDGE('',*,*,#17425,.T.);
#25260=ORIENTED_EDGE('',*,*,#17422,.T.);
#25261=ORIENTED_EDGE('',*,*,#17419,.T.);
#25262=ORIENTED_EDGE('',*,*,#17416,.T.);
#25263=ORIENTED_EDGE('',*,*,#17349,.T.);
#25264=ORIENTED_EDGE('',*,*,#17359,.T.);
#25265=ORIENTED_EDGE('',*,*,#17356,.T.);
#25266=ORIENTED_EDGE('',*,*,#17353,.T.);
#25267=ORIENTED_EDGE('',*,*,#17301,.T.);
#25268=ORIENTED_EDGE('',*,*,#17347,.T.);
#25269=ORIENTED_EDGE('',*,*,#17344,.T.);
#25270=ORIENTED_EDGE('',*,*,#17341,.T.);
#25271=ORIENTED_EDGE('',*,*,#17338,.T.);
#25272=ORIENTED_EDGE('',*,*,#17335,.T.);
#25273=ORIENTED_EDGE('',*,*,#17332,.T.);
#25274=ORIENTED_EDGE('',*,*,#17329,.T.);
#25275=ORIENTED_EDGE('',*,*,#17326,.T.);
#25276=ORIENTED_EDGE('',*,*,#17323,.T.);
#25277=ORIENTED_EDGE('',*,*,#17320,.T.);
#25278=ORIENTED_EDGE('',*,*,#17317,.T.);
#25279=ORIENTED_EDGE('',*,*,#17314,.T.);
#25280=ORIENTED_EDGE('',*,*,#17311,.T.);
#25281=ORIENTED_EDGE('',*,*,#17308,.T.);
#25282=ORIENTED_EDGE('',*,*,#17305,.T.);
#25283=ORIENTED_EDGE('',*,*,#17496,.F.);
#25284=ORIENTED_EDGE('',*,*,#17467,.F.);
#25285=ORIENTED_EDGE('',*,*,#17162,.F.);
#25286=ORIENTED_EDGE('',*,*,#17468,.F.);
#25287=ORIENTED_EDGE('',*,*,#17497,.T.);
#25288=ORIENTED_EDGE('',*,*,#17496,.T.);
#25289=ORIENTED_EDGE('',*,*,#17497,.F.);
#25290=CONICAL_SURFACE('',#27055,6.175,0.785398163397445);
#25291=CONICAL_SURFACE('',#27098,6.175,0.785398163397448);
#25292=CONICAL_SURFACE('',#27143,2.95,0.785398163397439);
#25293=CONICAL_SURFACE('',#27149,6.175,0.785398163397442);
#25294=CONICAL_SURFACE('',#27150,6.175,0.785398163397442);
#25295=CONICAL_SURFACE('',#27156,2.95,0.785398163397439);
#25296=CONICAL_SURFACE('',#27273,1.85,0.785398163397447);
#25297=CONICAL_SURFACE('',#27279,1.225,0.785398163397477);
#25298=CONICAL_SURFACE('',#27280,1.125,0.785398163397453);
#25299=CONICAL_SURFACE('',#27288,15.65,0.785398163397448);
#25300=CONICAL_SURFACE('',#27295,1.325,0.785398163397448);
#25301=CONICAL_SURFACE('',#27308,15.65,0.785398163397448);
#25302=CONICAL_SURFACE('',#27315,2.825,0.785398163397448);
#25303=CONICAL_SURFACE('',#27317,15.65,0.785398163397448);
#25304=CONICAL_SURFACE('',#27322,2.08,0.785398163397448);
#25305=CONICAL_SURFACE('',#27334,15.65,0.785398163397448);
#25306=CONICAL_SURFACE('',#27336,2.075,0.785398163397447);
#25307=CONICAL_SURFACE('',#27349,3.575,0.785398163397447);
#25308=CONICAL_SURFACE('',#27354,15.5353553390593,1.17809724509618);
#25309=CONICAL_SURFACE('',#27357,15.5353553390593,1.17809724509617);
#25310=CONICAL_SURFACE('',#27360,15.5353553390593,1.17809724509617);
#25311=CONICAL_SURFACE('',#27362,15.5353553390593,1.17809724509616);
#25312=CONICAL_SURFACE('',#27365,2.8,0.785398163397448);
#25313=CONICAL_SURFACE('',#27368,3.55,0.785398163397451);
#25314=CONICAL_SURFACE('',#27371,1.3,0.785398163397448);
#25315=CONICAL_SURFACE('',#27374,2.05,0.785398163397451);
#25316=CONICAL_SURFACE('',#27377,15.65,0.785398163397448);
#25317=CONICAL_SURFACE('',#27378,15.65,0.785398163397448);
#25318=CONICAL_SURFACE('',#27381,2.055,0.785398163397448);
#25319=CONICAL_SURFACE('',#27384,15.65,0.785398163397448);
#25320=CONICAL_SURFACE('',#27388,15.65,0.785398163397448);
#25321=CONICAL_SURFACE('',#27392,1.925,0.785398163397448);
#25322=CONICAL_SURFACE('',#27396,1.925,0.785398163397448);
#25323=CONICAL_SURFACE('',#27422,3.0525,0.785398163397439);
#25324=CONICAL_SURFACE('',#27426,7.4,0.785398163397448);
#25325=CONICAL_SURFACE('',#27427,7.4,0.785398163397448);
#25326=CONICAL_SURFACE('',#27431,3.0525,0.785398163397448);
#25327=CONICAL_SURFACE('',#27470,0.288675134594813,1.02910423288134);
#25328=CONICAL_SURFACE('',#27504,0.875,0.785398163397448);
#25329=CONICAL_SURFACE('',#27507,0.96,0.785398163397449);
#25330=CONICAL_SURFACE('',#27629,0.23094010767585,1.02878638855047);
#25331=CONICAL_SURFACE('',#27663,0.7,0.785398163397448);
#25332=CONICAL_SURFACE('',#27666,0.76,0.785398163397449);
#25333=CONICAL_SURFACE('',#27670,0.845,0.785398163397448);
#25334=CONICAL_SURFACE('',#27677,0.845,0.785398163397448);
#25335=CONICAL_SURFACE('',#27681,1.28782032302755,1.0471975511966);
#25336=CONICAL_SURFACE('',#27685,1.28782032302755,1.0471975511966);
#25337=CONICAL_SURFACE('',#27751,0.23094010767585,1.02878638855047);
#25338=CONICAL_SURFACE('',#27785,0.7,0.785398163397448);
#25339=CONICAL_SURFACE('',#27788,0.76,0.785398163397449);
#25340=CONICAL_SURFACE('',#27796,1.08,0.785398163397454);
#25341=CONICAL_SURFACE('',#27812,3.0525,0.785398163397448);
#25342=CONICAL_SURFACE('',#27816,7.4,0.785398163397448);
#25343=CONICAL_SURFACE('',#27817,7.4,0.785398163397448);
#25344=CONICAL_SURFACE('',#28283,0.855,0.785398163397457);
#25345=CONICAL_SURFACE('',#28284,1.83,0.785398163397454);
#25346=CONICAL_SURFACE('',#28285,1.755,1.02974425867665);
#25347=CONICAL_SURFACE('',#28387,1.205,1.02974425867666);
#25348=CONICAL_SURFACE('',#28390,2.4,0.785398163397442);
#25349=CONICAL_SURFACE('',#28657,2.65,0.785398163397453);
#25350=CONICAL_SURFACE('',#28674,3.85000000000001,0.78539816339744);
#25351=CONICAL_SURFACE('',#28676,3.85000000000001,0.78539816339744);
#25352=CONICAL_SURFACE('',#28694,11.85,0.785398163397442);
#25353=CONICAL_SURFACE('',#28704,3.85000000000001,0.78539816339744);
#25354=CONICAL_SURFACE('',#28728,3.85000000000002,0.785398163397439);
#25355=CONICAL_SURFACE('',#28729,2.65,0.785398163397453);
#25356=CONICAL_SURFACE('',#28731,2.65,0.785398163397453);
#25357=CONICAL_SURFACE('',#28737,2.65,0.785398163397453);
#25358=CONICAL_SURFACE('',#28745,8.15,0.785398163397451);
#25359=CONICAL_SURFACE('',#28763,3.85000000000001,0.78539816339744);
#25360=CONICAL_SURFACE('',#28775,8.15,0.785398163397448);
#25361=CONICAL_SURFACE('',#28820,6.355,0.785398163397448);
#25362=CONICAL_SURFACE('',#28824,6.355,0.785398163397448);
#25363=CONICAL_SURFACE('',#28828,10.15,0.785398163397448);
#25364=CONICAL_SURFACE('',#28833,9.85,0.785398163397448);
#25365=CONICAL_SURFACE('',#28834,10.15,0.785398163397448);
#25366=CONICAL_SURFACE('',#28838,9.85,0.785398163397448);
#25367=CONICAL_SURFACE('',#28841,11.85,0.785398163397442);
#25368=CONICAL_SURFACE('',#28843,5.15,0.785398163397438);
#25369=CONICAL_SURFACE('',#28847,3.85000000000002,0.785398163397439);
#25370=CONICAL_SURFACE('',#28850,8.15,0.785398163397448);
#25371=CONICAL_SURFACE('',#28856,8.15,0.785398163397451);
#25372=CONICAL_SURFACE('',#28860,5.15,0.785398163397438);
#25373=CONICAL_SURFACE('',#28863,1.4,0.785398163397447);
#25374=CONICAL_SURFACE('',#28866,1.4,0.785398163397447);
#25375=CONICAL_SURFACE('',#28868,1.4,0.785398163397447);
#25376=CONICAL_SURFACE('',#28871,1.4,0.785398163397447);
#25377=CONICAL_SURFACE('',#28880,1.35,0.785398163397446);
#25378=CONICAL_SURFACE('',#28881,1.35,0.785398163397446);
#25379=CONICAL_SURFACE('',#28884,1.35,0.785398163397455);
#25380=CONICAL_SURFACE('',#28887,1.35,0.785398163397455);
#25381=CONICAL_SURFACE('',#28950,1.28782032302755,1.0471975511966);
#25382=CONICAL_SURFACE('',#28961,0.75,0.785398163397448);
#25383=ADVANCED_FACE('',(#2570),#25290,.T.);
#25384=ADVANCED_FACE('',(#2571,#845),#1680,.T.);
#25385=ADVANCED_FACE('',(#2572),#518,.T.);
#25386=ADVANCED_FACE('',(#2573),#25291,.T.);
#25387=ADVANCED_FACE('',(#2574,#846),#1681,.T.);
#25388=ADVANCED_FACE('',(#2575),#519,.T.);
#25389=ADVANCED_FACE('',(#2576),#1682,.T.);
#25390=ADVANCED_FACE('',(#2577),#25292,.T.);
#25391=ADVANCED_FACE('',(#2578),#520,.T.);
#25392=ADVANCED_FACE('',(#2579,#847),#1683,.T.);
#25393=ADVANCED_FACE('',(#2580),#25293,.T.);
#25394=ADVANCED_FACE('',(#2581),#25294,.T.);
#25395=ADVANCED_FACE('',(#2582,#848),#1684,.T.);
#25396=ADVANCED_FACE('',(#2583),#521,.T.);
#25397=ADVANCED_FACE('',(#2584),#25295,.T.);
#25398=ADVANCED_FACE('',(#2585),#1685,.T.);
#25399=ADVANCED_FACE('',(#2586),#482,.F.);
#25400=ADVANCED_FACE('',(#2587),#522,.T.);
#25401=ADVANCED_FACE('',(#2588),#1686,.F.);
#25402=ADVANCED_FACE('',(#2589),#483,.F.);
#25403=ADVANCED_FACE('',(#2590),#1687,.F.);
#25404=ADVANCED_FACE('',(#2591),#484,.F.);
#25405=ADVANCED_FACE('',(#2592),#523,.T.);
#25406=ADVANCED_FACE('',(#2593),#1688,.F.);
#25407=ADVANCED_FACE('',(#2594),#485,.F.);
#25408=ADVANCED_FACE('',(#2595),#1689,.F.);
#25409=ADVANCED_FACE('',(#2596),#486,.F.);
#25410=ADVANCED_FACE('',(#2597),#524,.T.);
#25411=ADVANCED_FACE('',(#2598),#1690,.F.);
#25412=ADVANCED_FACE('',(#2599),#487,.F.);
#25413=ADVANCED_FACE('',(#2600),#1691,.F.);
#25414=ADVANCED_FACE('',(#2601),#488,.F.);
#25415=ADVANCED_FACE('',(#2602),#525,.T.);
#25416=ADVANCED_FACE('',(#2603),#1692,.F.);
#25417=ADVANCED_FACE('',(#2604),#489,.F.);
#25418=ADVANCED_FACE('',(#2605),#1693,.F.);
#25419=ADVANCED_FACE('',(#2606),#490,.F.);
#25420=ADVANCED_FACE('',(#2607),#526,.T.);
#25421=ADVANCED_FACE('',(#2608),#1694,.F.);
#25422=ADVANCED_FACE('',(#2609),#491,.F.);
#25423=ADVANCED_FACE('',(#2610),#1695,.F.);
#25424=ADVANCED_FACE('',(#2611),#492,.F.);
#25425=ADVANCED_FACE('',(#2612),#527,.T.);
#25426=ADVANCED_FACE('',(#2613),#1696,.F.);
#25427=ADVANCED_FACE('',(#2614),#493,.F.);
#25428=ADVANCED_FACE('',(#2615),#1697,.F.);
#25429=ADVANCED_FACE('',(#2616),#494,.F.);
#25430=ADVANCED_FACE('',(#2617),#528,.T.);
#25431=ADVANCED_FACE('',(#2618),#1698,.F.);
#25432=ADVANCED_FACE('',(#2619),#495,.F.);
#25433=ADVANCED_FACE('',(#2620),#1699,.F.);
#25434=ADVANCED_FACE('',(#2621),#496,.F.);
#25435=ADVANCED_FACE('',(#2622),#529,.T.);
#25436=ADVANCED_FACE('',(#2623),#1700,.F.);
#25437=ADVANCED_FACE('',(#2624),#497,.F.);
#25438=ADVANCED_FACE('',(#2625),#1701,.F.);
#25439=ADVANCED_FACE('',(#2626),#498,.F.);
#25440=ADVANCED_FACE('',(#2627),#530,.T.);
#25441=ADVANCED_FACE('',(#2628),#1702,.F.);
#25442=ADVANCED_FACE('',(#2629),#499,.F.);
#25443=ADVANCED_FACE('',(#2630),#1703,.F.);
#25444=ADVANCED_FACE('',(#2631),#500,.F.);
#25445=ADVANCED_FACE('',(#2632),#531,.T.);
#25446=ADVANCED_FACE('',(#2633),#1704,.F.);
#25447=ADVANCED_FACE('',(#2634),#501,.F.);
#25448=ADVANCED_FACE('',(#2635),#1705,.F.);
#25449=ADVANCED_FACE('',(#2636),#502,.F.);
#25450=ADVANCED_FACE('',(#2637),#532,.T.);
#25451=ADVANCED_FACE('',(#2638),#1706,.F.);
#25452=ADVANCED_FACE('',(#2639),#503,.F.);
#25453=ADVANCED_FACE('',(#2640),#1707,.F.);
#25454=ADVANCED_FACE('',(#2641),#504,.F.);
#25455=ADVANCED_FACE('',(#2642),#533,.T.);
#25456=ADVANCED_FACE('',(#2643),#1708,.F.);
#25457=ADVANCED_FACE('',(#2644),#505,.F.);
#25458=ADVANCED_FACE('',(#2645),#1709,.F.);
#25459=ADVANCED_FACE('',(#2646),#506,.F.);
#25460=ADVANCED_FACE('',(#2647),#534,.T.);
#25461=ADVANCED_FACE('',(#2648),#1710,.F.);
#25462=ADVANCED_FACE('',(#2649),#507,.F.);
#25463=ADVANCED_FACE('',(#2650),#1711,.F.);
#25464=ADVANCED_FACE('',(#2651),#508,.F.);
#25465=ADVANCED_FACE('',(#2652),#535,.T.);
#25466=ADVANCED_FACE('',(#2653),#1712,.F.);
#25467=ADVANCED_FACE('',(#2654),#509,.F.);
#25468=ADVANCED_FACE('',(#2655),#1713,.F.);
#25469=ADVANCED_FACE('',(#2656),#510,.F.);
#25470=ADVANCED_FACE('',(#2657),#536,.T.);
#25471=ADVANCED_FACE('',(#2658),#1714,.F.);
#25472=ADVANCED_FACE('',(#2659),#511,.F.);
#25473=ADVANCED_FACE('',(#2660),#1715,.F.);
#25474=ADVANCED_FACE('',(#2661),#512,.F.);
#25475=ADVANCED_FACE('',(#2662),#537,.T.);
#25476=ADVANCED_FACE('',(#2663),#1716,.F.);
#25477=ADVANCED_FACE('',(#2664),#513,.F.);
#25478=ADVANCED_FACE('',(#2665),#1717,.F.);
#25479=ADVANCED_FACE('',(#2666),#514,.F.);
#25480=ADVANCED_FACE('',(#2667),#538,.T.);
#25481=ADVANCED_FACE('',(#2668),#1718,.F.);
#25482=ADVANCED_FACE('',(#2669),#515,.F.);
#25483=ADVANCED_FACE('',(#2670),#1719,.F.);
#25484=ADVANCED_FACE('',(#2671),#516,.F.);
#25485=ADVANCED_FACE('',(#2672),#539,.T.);
#25486=ADVANCED_FACE('',(#2673),#1720,.F.);
#25487=ADVANCED_FACE('',(#2674),#517,.F.);
#25488=ADVANCED_FACE('',(#2675),#1721,.F.);
#25489=ADVANCED_FACE('',(#2676),#540,.T.);
#25490=ADVANCED_FACE('',(#2677),#541,.T.);
#25491=ADVANCED_FACE('',(#2678),#542,.T.);
#25492=ADVANCED_FACE('',(#2679),#543,.T.);
#25493=ADVANCED_FACE('',(#2680),#544,.T.);
#25494=ADVANCED_FACE('',(#2681),#545,.T.);
#25495=ADVANCED_FACE('',(#2682),#546,.T.);
#25496=ADVANCED_FACE('',(#2683),#547,.T.);
#25497=ADVANCED_FACE('',(#2684),#548,.T.);
#25498=ADVANCED_FACE('',(#2685),#549,.T.);
#25499=ADVANCED_FACE('',(#2686),#550,.T.);
#25500=ADVANCED_FACE('',(#2687),#551,.T.);
#25501=ADVANCED_FACE('',(#2688),#552,.T.);
#25502=ADVANCED_FACE('',(#2689),#553,.T.);
#25503=ADVANCED_FACE('',(#2690),#554,.T.);
#25504=ADVANCED_FACE('',(#2691),#555,.T.);
#25505=ADVANCED_FACE('',(#2692),#556,.T.);
#25506=ADVANCED_FACE('',(#2693),#557,.T.);
#25507=ADVANCED_FACE('',(#2694),#558,.T.);
#25508=ADVANCED_FACE('',(#2695),#559,.T.);
#25509=ADVANCED_FACE('',(#2696),#560,.T.);
#25510=ADVANCED_FACE('',(#2697),#561,.T.);
#25511=ADVANCED_FACE('',(#2698),#562,.T.);
#25512=ADVANCED_FACE('',(#2699),#563,.T.);
#25513=ADVANCED_FACE('',(#2700),#564,.T.);
#25514=ADVANCED_FACE('',(#2701),#565,.T.);
#25515=ADVANCED_FACE('',(#2702),#566,.T.);
#25516=ADVANCED_FACE('',(#2703),#567,.T.);
#25517=ADVANCED_FACE('',(#2704),#568,.T.);
#25518=ADVANCED_FACE('',(#2705),#569,.T.);
#25519=ADVANCED_FACE('',(#2706),#570,.T.);
#25520=ADVANCED_FACE('',(#2707),#571,.T.);
#25521=ADVANCED_FACE('',(#2708),#572,.T.);
#25522=ADVANCED_FACE('',(#2709),#573,.T.);
#25523=ADVANCED_FACE('',(#2710),#574,.T.);
#25524=ADVANCED_FACE('',(#2711),#575,.T.);
#25525=ADVANCED_FACE('',(#2712),#576,.T.);
#25526=ADVANCED_FACE('',(#2713),#577,.T.);
#25527=ADVANCED_FACE('',(#2714),#578,.T.);
#25528=ADVANCED_FACE('',(#2715),#579,.T.);
#25529=ADVANCED_FACE('',(#2716),#580,.T.);
#25530=ADVANCED_FACE('',(#2717),#581,.T.);
#25531=ADVANCED_FACE('',(#2718),#582,.T.);
#25532=ADVANCED_FACE('',(#2719),#583,.T.);
#25533=ADVANCED_FACE('',(#2720),#1722,.F.);
#25534=ADVANCED_FACE('',(#2721),#270,.F.);
#25535=ADVANCED_FACE('',(#2722),#1723,.T.);
#25536=ADVANCED_FACE('',(#2723),#584,.T.);
#25537=ADVANCED_FACE('',(#2724),#271,.F.);
#25538=ADVANCED_FACE('',(#2725),#585,.T.);
#25539=ADVANCED_FACE('',(#2726),#1724,.T.);
#25540=ADVANCED_FACE('',(#2727),#25296,.T.);
#25541=ADVANCED_FACE('',(#2728),#586,.T.);
#25542=ADVANCED_FACE('',(#2729,#849),#1725,.T.);
#25543=ADVANCED_FACE('',(#2730),#25297,.T.);
#25544=ADVANCED_FACE('',(#2731),#25298,.T.);
#25545=ADVANCED_FACE('',(#2732),#1726,.T.);
#25546=ADVANCED_FACE('',(#2733),#1727,.T.);
#25547=ADVANCED_FACE('',(#2734),#587,.T.);
#25548=ADVANCED_FACE('',(#2735),#25299,.T.);
#25549=ADVANCED_FACE('',(#2736),#1728,.T.);
#25550=ADVANCED_FACE('',(#2737),#1729,.T.);
#25551=ADVANCED_FACE('',(#2738),#1730,.T.);
#25552=ADVANCED_FACE('',(#2739),#1731,.F.);
#25553=ADVANCED_FACE('',(#2740),#1732,.T.);
#25554=ADVANCED_FACE('',(#2741),#25300,.F.);
#25555=ADVANCED_FACE('',(#2742),#1733,.T.);
#25556=ADVANCED_FACE('',(#2743,#850),#1734,.F.);
#25557=ADVANCED_FACE('',(#2744),#25301,.T.);
#25558=ADVANCED_FACE('',(#2745),#1735,.T.);
#25559=ADVANCED_FACE('',(#2746),#1736,.T.);
#25560=ADVANCED_FACE('',(#2747),#1737,.F.);
#25561=ADVANCED_FACE('',(#2748),#1738,.T.);
#25562=ADVANCED_FACE('',(#2749),#1739,.T.);
#25563=ADVANCED_FACE('',(#2750),#1740,.T.);
#25564=ADVANCED_FACE('',(#2751),#25302,.F.);
#25565=ADVANCED_FACE('',(#2752),#25303,.T.);
#25566=ADVANCED_FACE('',(#2753),#588,.F.);
#25567=ADVANCED_FACE('',(#2754),#1741,.F.);
#25568=ADVANCED_FACE('',(#2755),#25304,.F.);
#25569=ADVANCED_FACE('',(#2756),#589,.F.);
#25570=ADVANCED_FACE('',(#2757),#1742,.T.);
#25571=ADVANCED_FACE('',(#2758),#1743,.T.);
#25572=ADVANCED_FACE('',(#2759),#1744,.F.);
#25573=ADVANCED_FACE('',(#2760),#1745,.T.);
#25574=ADVANCED_FACE('',(#2761),#1746,.T.);
#25575=ADVANCED_FACE('',(#2762),#590,.T.);
#25576=ADVANCED_FACE('',(#2763),#25305,.T.);
#25577=ADVANCED_FACE('',(#2764),#1747,.T.);
#25578=ADVANCED_FACE('',(#2765),#25306,.F.);
#25579=ADVANCED_FACE('',(#2766),#591,.F.);
#25580=ADVANCED_FACE('',(#2767),#1748,.F.);
#25581=ADVANCED_FACE('',(#2768),#1749,.T.);
#25582=ADVANCED_FACE('',(#2769),#1750,.T.);
#25583=ADVANCED_FACE('',(#2770),#1751,.F.);
#25584=ADVANCED_FACE('',(#2771),#1752,.T.);
#25585=ADVANCED_FACE('',(#2772),#1753,.T.);
#25586=ADVANCED_FACE('',(#2773),#592,.T.);
#25587=ADVANCED_FACE('',(#2774),#1754,.T.);
#25588=ADVANCED_FACE('',(#2775),#25307,.F.);
#25589=ADVANCED_FACE('',(#2776),#593,.F.);
#25590=ADVANCED_FACE('',(#2777),#1755,.F.);
#25591=ADVANCED_FACE('',(#2778),#25308,.T.);
#25592=ADVANCED_FACE('',(#2779),#25309,.T.);
#25593=ADVANCED_FACE('',(#2780),#25310,.T.);
#25594=ADVANCED_FACE('',(#2781),#25311,.T.);
#25595=ADVANCED_FACE('',(#2782),#25312,.F.);
#25596=ADVANCED_FACE('',(#2783),#1756,.T.);
#25597=ADVANCED_FACE('',(#2784),#25313,.F.);
#25598=ADVANCED_FACE('',(#2785),#1757,.T.);
#25599=ADVANCED_FACE('',(#2786),#25314,.F.);
#25600=ADVANCED_FACE('',(#2787),#25315,.F.);
#25601=ADVANCED_FACE('',(#2788),#1758,.T.);
#25602=ADVANCED_FACE('',(#2789),#25316,.T.);
#25603=ADVANCED_FACE('',(#2790),#25317,.T.);
#25604=ADVANCED_FACE('',(#2791,#851),#1759,.T.);
#25605=ADVANCED_FACE('',(#2792),#25318,.F.);
#25606=ADVANCED_FACE('',(#2793),#594,.F.);
#25607=ADVANCED_FACE('',(#2794),#1760,.F.);
#25608=ADVANCED_FACE('',(#2795),#25319,.T.);
#25609=ADVANCED_FACE('',(#2796),#595,.T.);
#25610=ADVANCED_FACE('',(#2797),#25320,.T.);
#25611=ADVANCED_FACE('',(#2798),#1761,.T.);
#25612=ADVANCED_FACE('',(#2799),#25321,.T.);
#25613=ADVANCED_FACE('',(#2800),#596,.T.);
#25614=ADVANCED_FACE('',(#2801),#25322,.T.);
#25615=ADVANCED_FACE('',(#2802),#1762,.T.);
#25616=ADVANCED_FACE('',(#2803),#272,.T.);
#25617=ADVANCED_FACE('',(#2804),#597,.F.);
#25618=ADVANCED_FACE('',(#2805,#852,#853,#854,#855,#856,#857),#598,.T.);
#25619=ADVANCED_FACE('',(#2806),#273,.T.);
#25620=ADVANCED_FACE('',(#2807,#858),#599,.F.);
#25621=ADVANCED_FACE('',(#2808),#142,.T.);
#25622=ADVANCED_FACE('',(#2809),#600,.T.);
#25623=ADVANCED_FACE('',(#2810),#601,.T.);
#25624=ADVANCED_FACE('',(#2811),#602,.T.);
#25625=ADVANCED_FACE('',(#2812),#603,.T.);
#25626=ADVANCED_FACE('',(#2813),#604,.T.);
#25627=ADVANCED_FACE('',(#2814),#605,.T.);
#25628=ADVANCED_FACE('',(#2815),#25323,.F.);
#25629=ADVANCED_FACE('',(#2816,#859),#1763,.T.);
#25630=ADVANCED_FACE('',(#2817),#25324,.T.);
#25631=ADVANCED_FACE('',(#2818),#25325,.T.);
#25632=ADVANCED_FACE('',(#2819,#860),#1764,.T.);
#25633=ADVANCED_FACE('',(#2820),#25326,.F.);
#25634=ADVANCED_FACE('',(#2821),#606,.T.);
#25635=ADVANCED_FACE('',(#2822),#607,.T.);
#25636=ADVANCED_FACE('',(#2823),#608,.T.);
#25637=ADVANCED_FACE('',(#2824),#609,.T.);
#25638=ADVANCED_FACE('',(#2825),#610,.T.);
#25639=ADVANCED_FACE('',(#2826),#611,.T.);
#25640=ADVANCED_FACE('',(#2827),#612,.T.);
#25641=ADVANCED_FACE('',(#2828),#613,.T.);
#25642=ADVANCED_FACE('',(#2829),#614,.T.);
#25643=ADVANCED_FACE('',(#2830),#615,.T.);
#25644=ADVANCED_FACE('',(#2831),#616,.T.);
#25645=ADVANCED_FACE('',(#2832),#617,.T.);
#25646=ADVANCED_FACE('',(#2833),#618,.T.);
#25647=ADVANCED_FACE('',(#2834),#619,.T.);
#25648=ADVANCED_FACE('',(#2835),#1765,.F.);
#25649=ADVANCED_FACE('',(#2836),#274,.F.);
#25650=ADVANCED_FACE('',(#2837),#1766,.T.);
#25651=ADVANCED_FACE('',(#2838),#620,.T.);
#25652=ADVANCED_FACE('',(#2839),#275,.F.);
#25653=ADVANCED_FACE('',(#2840),#1767,.F.);
#25654=ADVANCED_FACE('',(#2841),#1768,.F.);
#25655=ADVANCED_FACE('',(#2842),#1769,.F.);
#25656=ADVANCED_FACE('',(#2843),#1770,.F.);
#25657=ADVANCED_FACE('',(#2844),#1771,.F.);
#25658=ADVANCED_FACE('',(#2845),#1772,.F.);
#25659=ADVANCED_FACE('',(#2846),#25327,.F.);
#25660=ADVANCED_FACE('',(#2847),#1773,.F.);
#25661=ADVANCED_FACE('',(#2848),#1774,.F.);
#25662=ADVANCED_FACE('',(#2849),#1775,.F.);
#25663=ADVANCED_FACE('',(#2850),#1776,.F.);
#25664=ADVANCED_FACE('',(#2851),#1777,.F.);
#25665=ADVANCED_FACE('',(#2852),#1778,.F.);
#25666=ADVANCED_FACE('',(#2853),#1779,.F.);
#25667=ADVANCED_FACE('',(#2854),#1780,.F.);
#25668=ADVANCED_FACE('',(#2855),#1781,.F.);
#25669=ADVANCED_FACE('',(#2856),#1782,.F.);
#25670=ADVANCED_FACE('',(#2857),#1783,.F.);
#25671=ADVANCED_FACE('',(#2858),#1784,.F.);
#25672=ADVANCED_FACE('',(#2859),#1785,.F.);
#25673=ADVANCED_FACE('',(#2860),#1786,.F.);
#25674=ADVANCED_FACE('',(#2861),#1787,.F.);
#25675=ADVANCED_FACE('',(#2862),#1788,.F.);
#25676=ADVANCED_FACE('',(#2863),#1789,.F.);
#25677=ADVANCED_FACE('',(#2864),#1790,.F.);
#25678=ADVANCED_FACE('',(#2865),#1791,.F.);
#25679=ADVANCED_FACE('',(#2866),#1792,.F.);
#25680=ADVANCED_FACE('',(#2867),#1793,.F.);
#25681=ADVANCED_FACE('',(#2868),#1794,.F.);
#25682=ADVANCED_FACE('',(#2869),#1795,.F.);
#25683=ADVANCED_FACE('',(#2870),#1796,.F.);
#25684=ADVANCED_FACE('',(#2871),#1797,.T.);
#25685=ADVANCED_FACE('',(#2872),#25328,.T.);
#25686=ADVANCED_FACE('',(#2873),#621,.T.);
#25687=ADVANCED_FACE('',(#2874),#25329,.T.);
#25688=ADVANCED_FACE('',(#2875,#861),#1798,.T.);
#25689=ADVANCED_FACE('',(#2876),#1799,.F.);
#25690=ADVANCED_FACE('',(#2877),#1800,.F.);
#25691=ADVANCED_FACE('',(#2878),#1801,.F.);
#25692=ADVANCED_FACE('',(#2879),#1802,.F.);
#25693=ADVANCED_FACE('',(#2880),#1803,.F.);
#25694=ADVANCED_FACE('',(#2881),#1804,.F.);
#25695=ADVANCED_FACE('',(#2882),#1805,.F.);
#25696=ADVANCED_FACE('',(#2883),#1806,.F.);
#25697=ADVANCED_FACE('',(#2884),#1807,.F.);
#25698=ADVANCED_FACE('',(#2885),#1808,.F.);
#25699=ADVANCED_FACE('',(#2886),#1809,.T.);
#25700=ADVANCED_FACE('',(#2887),#1810,.T.);
#25701=ADVANCED_FACE('',(#2888),#1811,.T.);
#25702=ADVANCED_FACE('',(#2889),#1812,.T.);
#25703=ADVANCED_FACE('',(#2890),#1813,.T.);
#25704=ADVANCED_FACE('',(#2891),#1814,.T.);
#25705=ADVANCED_FACE('',(#2892),#1815,.T.);
#25706=ADVANCED_FACE('',(#2893),#1816,.T.);
#25707=ADVANCED_FACE('',(#2894),#1817,.T.);
#25708=ADVANCED_FACE('',(#2895),#1818,.T.);
#25709=ADVANCED_FACE('',(#2896),#1819,.T.);
#25710=ADVANCED_FACE('',(#2897),#1820,.T.);
#25711=ADVANCED_FACE('',(#2898),#1821,.T.);
#25712=ADVANCED_FACE('',(#2899),#1822,.T.);
#25713=ADVANCED_FACE('',(#2900),#1823,.T.);
#25714=ADVANCED_FACE('',(#2901),#1824,.T.);
#25715=ADVANCED_FACE('',(#2902),#1825,.T.);
#25716=ADVANCED_FACE('',(#2903),#1826,.T.);
#25717=ADVANCED_FACE('',(#2904),#1827,.T.);
#25718=ADVANCED_FACE('',(#2905),#1828,.T.);
#25719=ADVANCED_FACE('',(#2906),#1829,.T.);
#25720=ADVANCED_FACE('',(#2907),#1830,.F.);
#25721=ADVANCED_FACE('',(#2908),#1831,.T.);
#25722=ADVANCED_FACE('',(#2909),#1832,.T.);
#25723=ADVANCED_FACE('',(#2910,#862,#863),#1833,.T.);
#25724=ADVANCED_FACE('',(#2911),#1834,.T.);
#25725=ADVANCED_FACE('',(#2912),#622,.T.);
#25726=ADVANCED_FACE('',(#2913),#623,.T.);
#25727=ADVANCED_FACE('',(#2914),#624,.T.);
#25728=ADVANCED_FACE('',(#2915),#625,.T.);
#25729=ADVANCED_FACE('',(#2916),#626,.T.);
#25730=ADVANCED_FACE('',(#2917),#627,.T.);
#25731=ADVANCED_FACE('',(#2918),#628,.T.);
#25732=ADVANCED_FACE('',(#2919),#629,.T.);
#25733=ADVANCED_FACE('',(#2920),#630,.T.);
#25734=ADVANCED_FACE('',(#2921),#631,.T.);
#25735=ADVANCED_FACE('',(#2922),#632,.T.);
#25736=ADVANCED_FACE('',(#2923),#633,.T.);
#25737=ADVANCED_FACE('',(#2924),#634,.T.);
#25738=ADVANCED_FACE('',(#2925),#635,.T.);
#25739=ADVANCED_FACE('',(#2926),#636,.T.);
#25740=ADVANCED_FACE('',(#2927),#637,.T.);
#25741=ADVANCED_FACE('',(#2928),#638,.T.);
#25742=ADVANCED_FACE('',(#2929),#639,.T.);
#25743=ADVANCED_FACE('',(#2930),#640,.T.);
#25744=ADVANCED_FACE('',(#2931),#641,.T.);
#25745=ADVANCED_FACE('',(#2932),#642,.T.);
#25746=ADVANCED_FACE('',(#2933),#643,.T.);
#25747=ADVANCED_FACE('',(#2934),#644,.T.);
#25748=ADVANCED_FACE('',(#2935),#645,.T.);
#25749=ADVANCED_FACE('',(#2936),#646,.T.);
#25750=ADVANCED_FACE('',(#2937),#647,.T.);
#25751=ADVANCED_FACE('',(#2938),#648,.T.);
#25752=ADVANCED_FACE('',(#2939),#649,.T.);
#25753=ADVANCED_FACE('',(#2940),#650,.T.);
#25754=ADVANCED_FACE('',(#2941),#651,.T.);
#25755=ADVANCED_FACE('',(#2942),#652,.T.);
#25756=ADVANCED_FACE('',(#2943),#653,.T.);
#25757=ADVANCED_FACE('',(#2944),#654,.T.);
#25758=ADVANCED_FACE('',(#2945),#655,.T.);
#25759=ADVANCED_FACE('',(#2946),#656,.T.);
#25760=ADVANCED_FACE('',(#2947),#657,.T.);
#25761=ADVANCED_FACE('',(#2948),#658,.T.);
#25762=ADVANCED_FACE('',(#2949),#659,.T.);
#25763=ADVANCED_FACE('',(#2950),#660,.T.);
#25764=ADVANCED_FACE('',(#2951),#661,.T.);
#25765=ADVANCED_FACE('',(#2952),#662,.T.);
#25766=ADVANCED_FACE('',(#2953),#663,.T.);
#25767=ADVANCED_FACE('',(#2954),#664,.T.);
#25768=ADVANCED_FACE('',(#2955),#665,.T.);
#25769=ADVANCED_FACE('',(#2956),#666,.T.);
#25770=ADVANCED_FACE('',(#2957),#667,.T.);
#25771=ADVANCED_FACE('',(#2958),#668,.T.);
#25772=ADVANCED_FACE('',(#2959),#669,.T.);
#25773=ADVANCED_FACE('',(#2960),#670,.T.);
#25774=ADVANCED_FACE('',(#2961),#671,.T.);
#25775=ADVANCED_FACE('',(#2962),#672,.T.);
#25776=ADVANCED_FACE('',(#2963),#673,.T.);
#25777=ADVANCED_FACE('',(#2964),#674,.T.);
#25778=ADVANCED_FACE('',(#2965),#675,.T.);
#25779=ADVANCED_FACE('',(#2966),#676,.T.);
#25780=ADVANCED_FACE('',(#2967),#677,.T.);
#25781=ADVANCED_FACE('',(#2968),#678,.T.);
#25782=ADVANCED_FACE('',(#2969),#679,.T.);
#25783=ADVANCED_FACE('',(#2970),#1835,.F.);
#25784=ADVANCED_FACE('',(#2971),#276,.F.);
#25785=ADVANCED_FACE('',(#2972),#1836,.T.);
#25786=ADVANCED_FACE('',(#2973),#680,.T.);
#25787=ADVANCED_FACE('',(#2974),#277,.F.);
#25788=ADVANCED_FACE('',(#2975),#1837,.F.);
#25789=ADVANCED_FACE('',(#2976),#1838,.F.);
#25790=ADVANCED_FACE('',(#2977),#1839,.F.);
#25791=ADVANCED_FACE('',(#2978),#1840,.F.);
#25792=ADVANCED_FACE('',(#2979),#1841,.F.);
#25793=ADVANCED_FACE('',(#2980),#1842,.F.);
#25794=ADVANCED_FACE('',(#2981),#25330,.F.);
#25795=ADVANCED_FACE('',(#2982),#1843,.F.);
#25796=ADVANCED_FACE('',(#2983),#1844,.F.);
#25797=ADVANCED_FACE('',(#2984),#1845,.F.);
#25798=ADVANCED_FACE('',(#2985),#1846,.F.);
#25799=ADVANCED_FACE('',(#2986),#1847,.F.);
#25800=ADVANCED_FACE('',(#2987),#1848,.F.);
#25801=ADVANCED_FACE('',(#2988),#1849,.F.);
#25802=ADVANCED_FACE('',(#2989),#1850,.F.);
#25803=ADVANCED_FACE('',(#2990),#1851,.F.);
#25804=ADVANCED_FACE('',(#2991),#1852,.F.);
#25805=ADVANCED_FACE('',(#2992),#1853,.F.);
#25806=ADVANCED_FACE('',(#2993),#1854,.F.);
#25807=ADVANCED_FACE('',(#2994),#1855,.F.);
#25808=ADVANCED_FACE('',(#2995),#1856,.F.);
#25809=ADVANCED_FACE('',(#2996),#1857,.F.);
#25810=ADVANCED_FACE('',(#2997),#1858,.F.);
#25811=ADVANCED_FACE('',(#2998),#1859,.F.);
#25812=ADVANCED_FACE('',(#2999),#1860,.F.);
#25813=ADVANCED_FACE('',(#3000),#1861,.F.);
#25814=ADVANCED_FACE('',(#3001),#1862,.F.);
#25815=ADVANCED_FACE('',(#3002),#1863,.F.);
#25816=ADVANCED_FACE('',(#3003),#1864,.F.);
#25817=ADVANCED_FACE('',(#3004),#1865,.F.);
#25818=ADVANCED_FACE('',(#3005),#1866,.F.);
#25819=ADVANCED_FACE('',(#3006),#1867,.T.);
#25820=ADVANCED_FACE('',(#3007),#25331,.T.);
#25821=ADVANCED_FACE('',(#3008),#681,.T.);
#25822=ADVANCED_FACE('',(#3009),#25332,.T.);
#25823=ADVANCED_FACE('',(#3010,#864),#1868,.T.);
#25824=ADVANCED_FACE('',(#3011),#25333,.F.);
#25825=ADVANCED_FACE('',(#3012),#682,.F.);
#25826=ADVANCED_FACE('',(#3013,#865),#1869,.F.);
#25827=ADVANCED_FACE('',(#3014),#25334,.F.);
#25828=ADVANCED_FACE('',(#3015,#866),#1870,.T.);
#25829=ADVANCED_FACE('',(#3016),#25335,.T.);
#25830=ADVANCED_FACE('',(#3017),#1871,.T.);
#25831=ADVANCED_FACE('',(#3018),#1872,.T.);
#25832=ADVANCED_FACE('',(#3019),#1873,.T.);
#25833=ADVANCED_FACE('',(#3020),#25336,.T.);
#25834=ADVANCED_FACE('',(#3021),#1874,.T.);
#25835=ADVANCED_FACE('',(#3022),#1875,.T.);
#25836=ADVANCED_FACE('',(#3023),#1876,.T.);
#25837=ADVANCED_FACE('',(#3024),#683,.T.);
#25838=ADVANCED_FACE('',(#3025),#684,.T.);
#25839=ADVANCED_FACE('',(#3026),#685,.T.);
#25840=ADVANCED_FACE('',(#3027),#686,.T.);
#25841=ADVANCED_FACE('',(#3028),#687,.T.);
#25842=ADVANCED_FACE('',(#3029),#688,.T.);
#25843=ADVANCED_FACE('',(#3030),#689,.T.);
#25844=ADVANCED_FACE('',(#3031),#690,.T.);
#25845=ADVANCED_FACE('',(#3032),#691,.T.);
#25846=ADVANCED_FACE('',(#3033),#692,.T.);
#25847=ADVANCED_FACE('',(#3034),#693,.T.);
#25848=ADVANCED_FACE('',(#3035),#694,.T.);
#25849=ADVANCED_FACE('',(#3036),#695,.T.);
#25850=ADVANCED_FACE('',(#3037),#696,.T.);
#25851=ADVANCED_FACE('',(#3038),#697,.T.);
#25852=ADVANCED_FACE('',(#3039),#698,.T.);
#25853=ADVANCED_FACE('',(#3040),#699,.T.);
#25854=ADVANCED_FACE('',(#3041),#700,.T.);
#25855=ADVANCED_FACE('',(#3042),#701,.T.);
#25856=ADVANCED_FACE('',(#3043),#702,.T.);
#25857=ADVANCED_FACE('',(#3044),#703,.T.);
#25858=ADVANCED_FACE('',(#3045),#704,.T.);
#25859=ADVANCED_FACE('',(#3046),#705,.T.);
#25860=ADVANCED_FACE('',(#3047),#706,.T.);
#25861=ADVANCED_FACE('',(#3048),#707,.T.);
#25862=ADVANCED_FACE('',(#3049),#708,.T.);
#25863=ADVANCED_FACE('',(#3050),#709,.T.);
#25864=ADVANCED_FACE('',(#3051),#710,.T.);
#25865=ADVANCED_FACE('',(#3052),#711,.T.);
#25866=ADVANCED_FACE('',(#3053),#712,.T.);
#25867=ADVANCED_FACE('',(#3054),#713,.T.);
#25868=ADVANCED_FACE('',(#3055),#714,.T.);
#25869=ADVANCED_FACE('',(#3056),#715,.T.);
#25870=ADVANCED_FACE('',(#3057),#716,.T.);
#25871=ADVANCED_FACE('',(#3058),#717,.T.);
#25872=ADVANCED_FACE('',(#3059),#718,.T.);
#25873=ADVANCED_FACE('',(#3060),#719,.T.);
#25874=ADVANCED_FACE('',(#3061),#720,.T.);
#25875=ADVANCED_FACE('',(#3062),#1877,.F.);
#25876=ADVANCED_FACE('',(#3063),#278,.F.);
#25877=ADVANCED_FACE('',(#3064),#1878,.T.);
#25878=ADVANCED_FACE('',(#3065),#721,.T.);
#25879=ADVANCED_FACE('',(#3066),#279,.F.);
#25880=ADVANCED_FACE('',(#3067),#1879,.F.);
#25881=ADVANCED_FACE('',(#3068),#1880,.F.);
#25882=ADVANCED_FACE('',(#3069),#1881,.F.);
#25883=ADVANCED_FACE('',(#3070),#1882,.F.);
#25884=ADVANCED_FACE('',(#3071),#1883,.F.);
#25885=ADVANCED_FACE('',(#3072),#1884,.F.);
#25886=ADVANCED_FACE('',(#3073),#25337,.F.);
#25887=ADVANCED_FACE('',(#3074),#1885,.F.);
#25888=ADVANCED_FACE('',(#3075),#1886,.F.);
#25889=ADVANCED_FACE('',(#3076),#1887,.F.);
#25890=ADVANCED_FACE('',(#3077),#1888,.F.);
#25891=ADVANCED_FACE('',(#3078),#1889,.F.);
#25892=ADVANCED_FACE('',(#3079),#1890,.F.);
#25893=ADVANCED_FACE('',(#3080),#1891,.F.);
#25894=ADVANCED_FACE('',(#3081),#1892,.F.);
#25895=ADVANCED_FACE('',(#3082),#1893,.F.);
#25896=ADVANCED_FACE('',(#3083),#1894,.F.);
#25897=ADVANCED_FACE('',(#3084),#1895,.F.);
#25898=ADVANCED_FACE('',(#3085),#1896,.F.);
#25899=ADVANCED_FACE('',(#3086),#1897,.F.);
#25900=ADVANCED_FACE('',(#3087),#1898,.F.);
#25901=ADVANCED_FACE('',(#3088),#1899,.F.);
#25902=ADVANCED_FACE('',(#3089),#1900,.F.);
#25903=ADVANCED_FACE('',(#3090),#1901,.F.);
#25904=ADVANCED_FACE('',(#3091),#1902,.F.);
#25905=ADVANCED_FACE('',(#3092),#1903,.F.);
#25906=ADVANCED_FACE('',(#3093),#1904,.F.);
#25907=ADVANCED_FACE('',(#3094),#1905,.F.);
#25908=ADVANCED_FACE('',(#3095),#1906,.F.);
#25909=ADVANCED_FACE('',(#3096),#1907,.F.);
#25910=ADVANCED_FACE('',(#3097),#1908,.F.);
#25911=ADVANCED_FACE('',(#3098),#1909,.T.);
#25912=ADVANCED_FACE('',(#3099),#25338,.T.);
#25913=ADVANCED_FACE('',(#3100),#722,.T.);
#25914=ADVANCED_FACE('',(#3101),#25339,.T.);
#25915=ADVANCED_FACE('',(#3102,#867),#1910,.T.);
#25916=ADVANCED_FACE('',(#3103),#280,.T.);
#25917=ADVANCED_FACE('',(#3104,#868,#869,#870),#723,.T.);
#25918=ADVANCED_FACE('',(#3105,#871),#724,.F.);
#25919=ADVANCED_FACE('',(#3106),#281,.T.);
#25920=ADVANCED_FACE('',(#3107),#25340,.F.);
#25921=ADVANCED_FACE('',(#3108),#725,.F.);
#25922=ADVANCED_FACE('',(#3109,#872),#1911,.T.);
#25923=ADVANCED_FACE('',(#3110),#282,.T.);
#25924=ADVANCED_FACE('',(#3111),#283,.T.);
#25925=ADVANCED_FACE('',(#3112),#284,.T.);
#25926=ADVANCED_FACE('',(#3113),#726,.F.);
#25927=ADVANCED_FACE('',(#3114,#873),#727,.F.);
#25928=ADVANCED_FACE('',(#3115),#285,.T.);
#25929=ADVANCED_FACE('',(#3116),#1912,.F.);
#25930=ADVANCED_FACE('',(#3117),#1913,.F.);
#25931=ADVANCED_FACE('',(#3118),#1914,.T.);
#25932=ADVANCED_FACE('',(#3119),#25341,.F.);
#25933=ADVANCED_FACE('',(#3120,#874),#1915,.T.);
#25934=ADVANCED_FACE('',(#3121),#25342,.T.);
#25935=ADVANCED_FACE('',(#3122),#25343,.T.);
#25936=ADVANCED_FACE('',(#3123),#1916,.T.);
#25937=ADVANCED_FACE('',(#3124),#1917,.T.);
#25938=ADVANCED_FACE('',(#3125),#1918,.F.);
#25939=ADVANCED_FACE('',(#3126),#1919,.T.);
#25940=ADVANCED_FACE('',(#3127),#1920,.T.);
#25941=ADVANCED_FACE('',(#3128),#1921,.T.);
#25942=ADVANCED_FACE('',(#3129),#1922,.F.);
#25943=ADVANCED_FACE('',(#3130),#1923,.T.);
#25944=ADVANCED_FACE('',(#3131),#1924,.T.);
#25945=ADVANCED_FACE('',(#3132),#1925,.F.);
#25946=ADVANCED_FACE('',(#3133),#1926,.T.);
#25947=ADVANCED_FACE('',(#3134),#1927,.T.);
#25948=ADVANCED_FACE('',(#3135),#1928,.T.);
#25949=ADVANCED_FACE('',(#3136),#1929,.T.);
#25950=ADVANCED_FACE('',(#3137),#1930,.F.);
#25951=ADVANCED_FACE('',(#3138),#1931,.T.);
#25952=ADVANCED_FACE('',(#3139),#1932,.T.);
#25953=ADVANCED_FACE('',(#3140),#1933,.T.);
#25954=ADVANCED_FACE('',(#3141),#1934,.T.);
#25955=ADVANCED_FACE('',(#3142),#1935,.T.);
#25956=ADVANCED_FACE('',(#3143),#1936,.T.);
#25957=ADVANCED_FACE('',(#3144),#1937,.T.);
#25958=ADVANCED_FACE('',(#3145),#1938,.T.);
#25959=ADVANCED_FACE('',(#3146),#1939,.T.);
#25960=ADVANCED_FACE('',(#3147),#1940,.T.);
#25961=ADVANCED_FACE('',(#3148),#1941,.T.);
#25962=ADVANCED_FACE('',(#3149),#1942,.T.);
#25963=ADVANCED_FACE('',(#3150),#1943,.F.);
#25964=ADVANCED_FACE('',(#3151),#1944,.T.);
#25965=ADVANCED_FACE('',(#3152),#1945,.T.);
#25966=ADVANCED_FACE('',(#3153),#1946,.T.);
#25967=ADVANCED_FACE('',(#3154),#1947,.T.);
#25968=ADVANCED_FACE('',(#3155),#1948,.T.);
#25969=ADVANCED_FACE('',(#3156),#1949,.T.);
#25970=ADVANCED_FACE('',(#3157),#1950,.T.);
#25971=ADVANCED_FACE('',(#3158),#1951,.T.);
#25972=ADVANCED_FACE('',(#3159),#1952,.T.);
#25973=ADVANCED_FACE('',(#3160),#1953,.T.);
#25974=ADVANCED_FACE('',(#3161),#1954,.T.);
#25975=ADVANCED_FACE('',(#3162),#1955,.T.);
#25976=ADVANCED_FACE('',(#3163),#1956,.T.);
#25977=ADVANCED_FACE('',(#3164),#1957,.F.);
#25978=ADVANCED_FACE('',(#3165),#1958,.T.);
#25979=ADVANCED_FACE('',(#3166),#1959,.T.);
#25980=ADVANCED_FACE('',(#3167),#1960,.T.);
#25981=ADVANCED_FACE('',(#3168),#1961,.T.);
#25982=ADVANCED_FACE('',(#3169),#1962,.T.);
#25983=ADVANCED_FACE('',(#3170),#1963,.T.);
#25984=ADVANCED_FACE('',(#3171),#1964,.T.);
#25985=ADVANCED_FACE('',(#3172),#1965,.T.);
#25986=ADVANCED_FACE('',(#3173),#1966,.T.);
#25987=ADVANCED_FACE('',(#3174),#1967,.F.);
#25988=ADVANCED_FACE('',(#3175),#1968,.T.);
#25989=ADVANCED_FACE('',(#3176),#1969,.T.);
#25990=ADVANCED_FACE('',(#3177),#1970,.T.);
#25991=ADVANCED_FACE('',(#3178),#1971,.F.);
#25992=ADVANCED_FACE('',(#3179),#1972,.T.);
#25993=ADVANCED_FACE('',(#3180),#1973,.T.);
#25994=ADVANCED_FACE('',(#3181),#1974,.T.);
#25995=ADVANCED_FACE('',(#3182),#1975,.T.);
#25996=ADVANCED_FACE('',(#3183),#1976,.T.);
#25997=ADVANCED_FACE('',(#3184),#1977,.T.);
#25998=ADVANCED_FACE('',(#3185),#1978,.T.);
#25999=ADVANCED_FACE('',(#3186),#1979,.T.);
#26000=ADVANCED_FACE('',(#3187),#1980,.T.);
#26001=ADVANCED_FACE('',(#3188),#1981,.T.);
#26002=ADVANCED_FACE('',(#3189),#1982,.T.);
#26003=ADVANCED_FACE('',(#3190),#1983,.T.);
#26004=ADVANCED_FACE('',(#3191),#1984,.T.);
#26005=ADVANCED_FACE('',(#3192),#1985,.T.);
#26006=ADVANCED_FACE('',(#3193),#1986,.T.);
#26007=ADVANCED_FACE('',(#3194),#1987,.T.);
#26008=ADVANCED_FACE('',(#3195),#1988,.F.);
#26009=ADVANCED_FACE('',(#3196),#1989,.T.);
#26010=ADVANCED_FACE('',(#3197),#1990,.T.);
#26011=ADVANCED_FACE('',(#3198),#1991,.T.);
#26012=ADVANCED_FACE('',(#3199),#1992,.T.);
#26013=ADVANCED_FACE('',(#3200),#1993,.T.);
#26014=ADVANCED_FACE('',(#3201),#1994,.T.);
#26015=ADVANCED_FACE('',(#3202),#1995,.T.);
#26016=ADVANCED_FACE('',(#3203),#1996,.T.);
#26017=ADVANCED_FACE('',(#3204),#1997,.T.);
#26018=ADVANCED_FACE('',(#3205),#1998,.T.);
#26019=ADVANCED_FACE('',(#3206),#1999,.T.);
#26020=ADVANCED_FACE('',(#3207),#2000,.T.);
#26021=ADVANCED_FACE('',(#3208),#2001,.T.);
#26022=ADVANCED_FACE('',(#3209),#2002,.T.);
#26023=ADVANCED_FACE('',(#3210),#2003,.T.);
#26024=ADVANCED_FACE('',(#3211),#2004,.F.);
#26025=ADVANCED_FACE('',(#3212),#2005,.T.);
#26026=ADVANCED_FACE('',(#3213),#2006,.T.);
#26027=ADVANCED_FACE('',(#3214,#875),#2007,.F.);
#26028=ADVANCED_FACE('',(#3215),#2008,.T.);
#26029=ADVANCED_FACE('',(#3216),#2009,.T.);
#26030=ADVANCED_FACE('',(#3217),#2010,.T.);
#26031=ADVANCED_FACE('',(#3218),#2011,.T.);
#26032=ADVANCED_FACE('',(#3219),#2012,.T.);
#26033=ADVANCED_FACE('',(#3220),#2013,.T.);
#26034=ADVANCED_FACE('',(#3221),#2014,.T.);
#26035=ADVANCED_FACE('',(#3222),#2015,.T.);
#26036=ADVANCED_FACE('',(#3223),#2016,.T.);
#26037=ADVANCED_FACE('',(#3224),#2017,.T.);
#26038=ADVANCED_FACE('',(#3225),#2018,.T.);
#26039=ADVANCED_FACE('',(#3226),#2019,.T.);
#26040=ADVANCED_FACE('',(#3227),#2020,.T.);
#26041=ADVANCED_FACE('',(#3228),#2021,.T.);
#26042=ADVANCED_FACE('',(#3229),#2022,.T.);
#26043=ADVANCED_FACE('',(#3230),#2023,.T.);
#26044=ADVANCED_FACE('',(#3231),#2024,.T.);
#26045=ADVANCED_FACE('',(#3232),#2025,.T.);
#26046=ADVANCED_FACE('',(#3233),#2026,.T.);
#26047=ADVANCED_FACE('',(#3234),#2027,.T.);
#26048=ADVANCED_FACE('',(#3235),#2028,.T.);
#26049=ADVANCED_FACE('',(#3236),#2029,.T.);
#26050=ADVANCED_FACE('',(#3237),#2030,.T.);
#26051=ADVANCED_FACE('',(#3238),#2031,.T.);
#26052=ADVANCED_FACE('',(#3239),#2032,.T.);
#26053=ADVANCED_FACE('',(#3240),#2033,.T.);
#26054=ADVANCED_FACE('',(#3241),#2034,.T.);
#26055=ADVANCED_FACE('',(#3242),#2035,.T.);
#26056=ADVANCED_FACE('',(#3243),#2036,.T.);
#26057=ADVANCED_FACE('',(#3244),#2037,.T.);
#26058=ADVANCED_FACE('',(#3245),#2038,.T.);
#26059=ADVANCED_FACE('',(#3246),#2039,.T.);
#26060=ADVANCED_FACE('',(#3247),#2040,.T.);
#26061=ADVANCED_FACE('',(#3248),#2041,.T.);
#26062=ADVANCED_FACE('',(#3249),#2042,.T.);
#26063=ADVANCED_FACE('',(#3250),#2043,.F.);
#26064=ADVANCED_FACE('',(#3251),#2044,.T.);
#26065=ADVANCED_FACE('',(#3252),#2045,.T.);
#26066=ADVANCED_FACE('',(#3253),#2046,.T.);
#26067=ADVANCED_FACE('',(#3254),#2047,.F.);
#26068=ADVANCED_FACE('',(#3255),#2048,.F.);
#26069=ADVANCED_FACE('',(#3256),#2049,.T.);
#26070=ADVANCED_FACE('',(#3257),#2050,.F.);
#26071=ADVANCED_FACE('',(#3258),#2051,.F.);
#26072=ADVANCED_FACE('',(#3259),#2052,.F.);
#26073=ADVANCED_FACE('',(#3260),#2053,.T.);
#26074=ADVANCED_FACE('',(#3261),#2054,.F.);
#26075=ADVANCED_FACE('',(#3262),#2055,.F.);
#26076=ADVANCED_FACE('',(#3263),#2056,.T.);
#26077=ADVANCED_FACE('',(#3264),#2057,.T.);
#26078=ADVANCED_FACE('',(#3265),#2058,.F.);
#26079=ADVANCED_FACE('',(#3266),#2059,.F.);
#26080=ADVANCED_FACE('',(#3267),#2060,.T.);
#26081=ADVANCED_FACE('',(#3268),#2061,.F.);
#26082=ADVANCED_FACE('',(#3269),#2062,.F.);
#26083=ADVANCED_FACE('',(#3270),#2063,.F.);
#26084=ADVANCED_FACE('',(#3271),#2064,.T.);
#26085=ADVANCED_FACE('',(#3272),#2065,.F.);
#26086=ADVANCED_FACE('',(#3273),#2066,.F.);
#26087=ADVANCED_FACE('',(#3274),#2067,.F.);
#26088=ADVANCED_FACE('',(#3275),#2068,.T.);
#26089=ADVANCED_FACE('',(#3276),#2069,.F.);
#26090=ADVANCED_FACE('',(#3277),#2070,.F.);
#26091=ADVANCED_FACE('',(#3278),#2071,.F.);
#26092=ADVANCED_FACE('',(#3279),#2072,.T.);
#26093=ADVANCED_FACE('',(#3280),#2073,.F.);
#26094=ADVANCED_FACE('',(#3281),#2074,.F.);
#26095=ADVANCED_FACE('',(#3282),#2075,.T.);
#26096=ADVANCED_FACE('',(#3283),#2076,.T.);
#26097=ADVANCED_FACE('',(#3284),#2077,.T.);
#26098=ADVANCED_FACE('',(#3285),#2078,.T.);
#26099=ADVANCED_FACE('',(#3286),#2079,.T.);
#26100=ADVANCED_FACE('',(#3287),#2080,.T.);
#26101=ADVANCED_FACE('',(#3288),#2081,.T.);
#26102=ADVANCED_FACE('',(#3289),#2082,.T.);
#26103=ADVANCED_FACE('',(#3290),#2083,.T.);
#26104=ADVANCED_FACE('',(#3291),#2084,.T.);
#26105=ADVANCED_FACE('',(#3292),#2085,.T.);
#26106=ADVANCED_FACE('',(#3293),#2086,.T.);
#26107=ADVANCED_FACE('',(#3294),#2087,.T.);
#26108=ADVANCED_FACE('',(#3295),#2088,.T.);
#26109=ADVANCED_FACE('',(#3296),#2089,.F.);
#26110=ADVANCED_FACE('',(#3297),#2090,.T.);
#26111=ADVANCED_FACE('',(#3298),#2091,.F.);
#26112=ADVANCED_FACE('',(#3299),#2092,.F.);
#26113=ADVANCED_FACE('',(#3300),#2093,.F.);
#26114=ADVANCED_FACE('',(#3301),#2094,.T.);
#26115=ADVANCED_FACE('',(#3302),#2095,.F.);
#26116=ADVANCED_FACE('',(#3303),#2096,.F.);
#26117=ADVANCED_FACE('',(#3304),#2097,.T.);
#26118=ADVANCED_FACE('',(#3305),#2098,.F.);
#26119=ADVANCED_FACE('',(#3306),#2099,.F.);
#26120=ADVANCED_FACE('',(#3307),#2100,.F.);
#26121=ADVANCED_FACE('',(#3308),#2101,.T.);
#26122=ADVANCED_FACE('',(#3309),#2102,.T.);
#26123=ADVANCED_FACE('',(#3310),#2103,.F.);
#26124=ADVANCED_FACE('',(#3311),#2104,.F.);
#26125=ADVANCED_FACE('',(#3312),#2105,.T.);
#26126=ADVANCED_FACE('',(#3313),#2106,.F.);
#26127=ADVANCED_FACE('',(#3314),#2107,.F.);
#26128=ADVANCED_FACE('',(#3315),#2108,.T.);
#26129=ADVANCED_FACE('',(#3316),#2109,.F.);
#26130=ADVANCED_FACE('',(#3317),#2110,.F.);
#26131=ADVANCED_FACE('',(#3318),#2111,.T.);
#26132=ADVANCED_FACE('',(#3319),#2112,.F.);
#26133=ADVANCED_FACE('',(#3320),#2113,.F.);
#26134=ADVANCED_FACE('',(#3321),#2114,.T.);
#26135=ADVANCED_FACE('',(#3322),#2115,.F.);
#26136=ADVANCED_FACE('',(#3323),#2116,.F.);
#26137=ADVANCED_FACE('',(#3324),#2117,.F.);
#26138=ADVANCED_FACE('',(#3325),#2118,.T.);
#26139=ADVANCED_FACE('',(#3326),#2119,.T.);
#26140=ADVANCED_FACE('',(#3327),#2120,.T.);
#26141=ADVANCED_FACE('',(#3328),#2121,.T.);
#26142=ADVANCED_FACE('',(#3329),#2122,.T.);
#26143=ADVANCED_FACE('',(#3330),#2123,.T.);
#26144=ADVANCED_FACE('',(#3331),#2124,.T.);
#26145=ADVANCED_FACE('',(#3332),#2125,.T.);
#26146=ADVANCED_FACE('',(#3333),#2126,.T.);
#26147=ADVANCED_FACE('',(#3334),#2127,.T.);
#26148=ADVANCED_FACE('',(#3335),#2128,.T.);
#26149=ADVANCED_FACE('',(#3336),#2129,.T.);
#26150=ADVANCED_FACE('',(#3337),#2130,.T.);
#26151=ADVANCED_FACE('',(#3338),#2131,.T.);
#26152=ADVANCED_FACE('',(#3339),#2132,.T.);
#26153=ADVANCED_FACE('',(#3340),#2133,.T.);
#26154=ADVANCED_FACE('',(#3341),#2134,.T.);
#26155=ADVANCED_FACE('',(#3342),#2135,.T.);
#26156=ADVANCED_FACE('',(#3343),#2136,.T.);
#26157=ADVANCED_FACE('',(#3344),#2137,.F.);
#26158=ADVANCED_FACE('',(#3345),#2138,.T.);
#26159=ADVANCED_FACE('',(#3346),#2139,.T.);
#26160=ADVANCED_FACE('',(#3347),#2140,.T.);
#26161=ADVANCED_FACE('',(#3348),#2141,.F.);
#26162=ADVANCED_FACE('',(#3349),#2142,.T.);
#26163=ADVANCED_FACE('',(#3350),#2143,.T.);
#26164=ADVANCED_FACE('',(#3351),#2144,.T.);
#26165=ADVANCED_FACE('',(#3352),#2145,.T.);
#26166=ADVANCED_FACE('',(#3353),#2146,.T.);
#26167=ADVANCED_FACE('',(#3354),#2147,.T.);
#26168=ADVANCED_FACE('',(#3355),#2148,.T.);
#26169=ADVANCED_FACE('',(#3356),#2149,.T.);
#26170=ADVANCED_FACE('',(#3357),#2150,.T.);
#26171=ADVANCED_FACE('',(#3358),#2151,.T.);
#26172=ADVANCED_FACE('',(#3359),#2152,.T.);
#26173=ADVANCED_FACE('',(#3360),#2153,.T.);
#26174=ADVANCED_FACE('',(#3361),#2154,.T.);
#26175=ADVANCED_FACE('',(#3362),#2155,.T.);
#26176=ADVANCED_FACE('',(#3363),#2156,.T.);
#26177=ADVANCED_FACE('',(#3364),#2157,.T.);
#26178=ADVANCED_FACE('',(#3365),#2158,.F.);
#26179=ADVANCED_FACE('',(#3366),#2159,.T.);
#26180=ADVANCED_FACE('',(#3367),#2160,.T.);
#26181=ADVANCED_FACE('',(#3368),#2161,.F.);
#26182=ADVANCED_FACE('',(#3369),#2162,.F.);
#26183=ADVANCED_FACE('',(#3370),#2163,.T.);
#26184=ADVANCED_FACE('',(#3371),#2164,.F.);
#26185=ADVANCED_FACE('',(#3372),#2165,.F.);
#26186=ADVANCED_FACE('',(#3373),#2166,.F.);
#26187=ADVANCED_FACE('',(#3374),#2167,.T.);
#26188=ADVANCED_FACE('',(#3375),#2168,.T.);
#26189=ADVANCED_FACE('',(#3376),#2169,.F.);
#26190=ADVANCED_FACE('',(#3377),#2170,.F.);
#26191=ADVANCED_FACE('',(#3378),#2171,.T.);
#26192=ADVANCED_FACE('',(#3379),#2172,.F.);
#26193=ADVANCED_FACE('',(#3380),#2173,.F.);
#26194=ADVANCED_FACE('',(#3381),#2174,.T.);
#26195=ADVANCED_FACE('',(#3382),#2175,.F.);
#26196=ADVANCED_FACE('',(#3383),#2176,.F.);
#26197=ADVANCED_FACE('',(#3384),#2177,.F.);
#26198=ADVANCED_FACE('',(#3385),#2178,.T.);
#26199=ADVANCED_FACE('',(#3386),#2179,.F.);
#26200=ADVANCED_FACE('',(#3387),#2180,.F.);
#26201=ADVANCED_FACE('',(#3388),#2181,.F.);
#26202=ADVANCED_FACE('',(#3389),#2182,.T.);
#26203=ADVANCED_FACE('',(#3390),#2183,.F.);
#26204=ADVANCED_FACE('',(#3391),#2184,.F.);
#26205=ADVANCED_FACE('',(#3392),#2185,.T.);
#26206=ADVANCED_FACE('',(#3393),#2186,.F.);
#26207=ADVANCED_FACE('',(#3394),#2187,.F.);
#26208=ADVANCED_FACE('',(#3395),#2188,.T.);
#26209=ADVANCED_FACE('',(#3396),#2189,.F.);
#26210=ADVANCED_FACE('',(#3397),#2190,.F.);
#26211=ADVANCED_FACE('',(#3398),#2191,.F.);
#26212=ADVANCED_FACE('',(#3399),#2192,.T.);
#26213=ADVANCED_FACE('',(#3400),#2193,.T.);
#26214=ADVANCED_FACE('',(#3401),#2194,.T.);
#26215=ADVANCED_FACE('',(#3402),#2195,.T.);
#26216=ADVANCED_FACE('',(#3403),#2196,.T.);
#26217=ADVANCED_FACE('',(#3404),#2197,.T.);
#26218=ADVANCED_FACE('',(#3405),#2198,.T.);
#26219=ADVANCED_FACE('',(#3406),#2199,.T.);
#26220=ADVANCED_FACE('',(#3407),#2200,.T.);
#26221=ADVANCED_FACE('',(#3408),#2201,.T.);
#26222=ADVANCED_FACE('',(#3409),#2202,.T.);
#26223=ADVANCED_FACE('',(#3410),#2203,.T.);
#26224=ADVANCED_FACE('',(#3411),#2204,.T.);
#26225=ADVANCED_FACE('',(#3412),#2205,.T.);
#26226=ADVANCED_FACE('',(#3413),#2206,.T.);
#26227=ADVANCED_FACE('',(#3414),#2207,.T.);
#26228=ADVANCED_FACE('',(#3415),#2208,.T.);
#26229=ADVANCED_FACE('',(#3416),#2209,.T.);
#26230=ADVANCED_FACE('',(#3417),#2210,.T.);
#26231=ADVANCED_FACE('',(#3418),#2211,.T.);
#26232=ADVANCED_FACE('',(#3419),#2212,.T.);
#26233=ADVANCED_FACE('',(#3420),#2213,.T.);
#26234=ADVANCED_FACE('',(#3421),#2214,.T.);
#26235=ADVANCED_FACE('',(#3422),#2215,.T.);
#26236=ADVANCED_FACE('',(#3423),#2216,.T.);
#26237=ADVANCED_FACE('',(#3424),#2217,.T.);
#26238=ADVANCED_FACE('',(#3425),#2218,.T.);
#26239=ADVANCED_FACE('',(#3426),#2219,.T.);
#26240=ADVANCED_FACE('',(#3427),#2220,.T.);
#26241=ADVANCED_FACE('',(#3428),#2221,.T.);
#26242=ADVANCED_FACE('',(#3429),#2222,.T.);
#26243=ADVANCED_FACE('',(#3430),#2223,.T.);
#26244=ADVANCED_FACE('',(#3431),#2224,.T.);
#26245=ADVANCED_FACE('',(#3432),#2225,.T.);
#26246=ADVANCED_FACE('',(#3433),#2226,.T.);
#26247=ADVANCED_FACE('',(#3434),#2227,.T.);
#26248=ADVANCED_FACE('',(#3435),#2228,.T.);
#26249=ADVANCED_FACE('',(#3436),#2229,.T.);
#26250=ADVANCED_FACE('',(#3437),#2230,.F.);
#26251=ADVANCED_FACE('',(#3438),#2231,.T.);
#26252=ADVANCED_FACE('',(#3439),#2232,.T.);
#26253=ADVANCED_FACE('',(#3440),#2233,.F.);
#26254=ADVANCED_FACE('',(#3441),#2234,.F.);
#26255=ADVANCED_FACE('',(#3442),#2235,.T.);
#26256=ADVANCED_FACE('',(#3443),#2236,.F.);
#26257=ADVANCED_FACE('',(#3444),#2237,.F.);
#26258=ADVANCED_FACE('',(#3445),#2238,.F.);
#26259=ADVANCED_FACE('',(#3446),#2239,.T.);
#26260=ADVANCED_FACE('',(#3447),#2240,.F.);
#26261=ADVANCED_FACE('',(#3448),#2241,.F.);
#26262=ADVANCED_FACE('',(#3449),#2242,.F.);
#26263=ADVANCED_FACE('',(#3450),#2243,.T.);
#26264=ADVANCED_FACE('',(#3451),#2244,.F.);
#26265=ADVANCED_FACE('',(#3452),#2245,.F.);
#26266=ADVANCED_FACE('',(#3453),#2246,.F.);
#26267=ADVANCED_FACE('',(#3454),#2247,.T.);
#26268=ADVANCED_FACE('',(#3455),#2248,.F.);
#26269=ADVANCED_FACE('',(#3456),#2249,.F.);
#26270=ADVANCED_FACE('',(#3457),#2250,.F.);
#26271=ADVANCED_FACE('',(#3458),#2251,.T.);
#26272=ADVANCED_FACE('',(#3459),#2252,.F.);
#26273=ADVANCED_FACE('',(#3460),#2253,.F.);
#26274=ADVANCED_FACE('',(#3461),#2254,.F.);
#26275=ADVANCED_FACE('',(#3462),#2255,.T.);
#26276=ADVANCED_FACE('',(#3463),#2256,.F.);
#26277=ADVANCED_FACE('',(#3464),#2257,.F.);
#26278=ADVANCED_FACE('',(#3465),#2258,.T.);
#26279=ADVANCED_FACE('',(#3466),#2259,.T.);
#26280=ADVANCED_FACE('',(#3467),#2260,.T.);
#26281=ADVANCED_FACE('',(#3468),#2261,.T.);
#26282=ADVANCED_FACE('',(#3469,#876),#2262,.T.);
#26283=ADVANCED_FACE('',(#3470),#2263,.T.);
#26284=ADVANCED_FACE('',(#3471),#2264,.T.);
#26285=ADVANCED_FACE('',(#3472),#2265,.T.);
#26286=ADVANCED_FACE('',(#3473),#2266,.T.);
#26287=ADVANCED_FACE('',(#3474),#2267,.T.);
#26288=ADVANCED_FACE('',(#3475),#2268,.T.);
#26289=ADVANCED_FACE('',(#3476),#2269,.T.);
#26290=ADVANCED_FACE('',(#3477),#2270,.T.);
#26291=ADVANCED_FACE('',(#3478),#2271,.T.);
#26292=ADVANCED_FACE('',(#3479),#2272,.T.);
#26293=ADVANCED_FACE('',(#3480),#2273,.T.);
#26294=ADVANCED_FACE('',(#3481),#2274,.T.);
#26295=ADVANCED_FACE('',(#3482),#2275,.T.);
#26296=ADVANCED_FACE('',(#3483),#2276,.T.);
#26297=ADVANCED_FACE('',(#3484),#2277,.T.);
#26298=ADVANCED_FACE('',(#3485),#2278,.T.);
#26299=ADVANCED_FACE('',(#3486),#2279,.T.);
#26300=ADVANCED_FACE('',(#3487),#2280,.T.);
#26301=ADVANCED_FACE('',(#3488),#2281,.T.);
#26302=ADVANCED_FACE('',(#3489),#2282,.T.);
#26303=ADVANCED_FACE('',(#3490),#2283,.T.);
#26304=ADVANCED_FACE('',(#3491),#2284,.T.);
#26305=ADVANCED_FACE('',(#3492),#2285,.T.);
#26306=ADVANCED_FACE('',(#3493),#2286,.T.);
#26307=ADVANCED_FACE('',(#3494),#2287,.T.);
#26308=ADVANCED_FACE('',(#3495),#2288,.T.);
#26309=ADVANCED_FACE('',(#3496),#2289,.T.);
#26310=ADVANCED_FACE('',(#3497),#2290,.T.);
#26311=ADVANCED_FACE('',(#3498),#2291,.T.);
#26312=ADVANCED_FACE('',(#3499),#2292,.T.);
#26313=ADVANCED_FACE('',(#3500),#2293,.T.);
#26314=ADVANCED_FACE('',(#3501),#2294,.T.);
#26315=ADVANCED_FACE('',(#3502),#2295,.T.);
#26316=ADVANCED_FACE('',(#3503),#2296,.T.);
#26317=ADVANCED_FACE('',(#3504),#2297,.T.);
#26318=ADVANCED_FACE('',(#3505),#2298,.T.);
#26319=ADVANCED_FACE('',(#3506),#2299,.T.);
#26320=ADVANCED_FACE('',(#3507),#2300,.T.);
#26321=ADVANCED_FACE('',(#3508),#2301,.T.);
#26322=ADVANCED_FACE('',(#3509),#2302,.T.);
#26323=ADVANCED_FACE('',(#3510),#2303,.T.);
#26324=ADVANCED_FACE('',(#3511),#2304,.T.);
#26325=ADVANCED_FACE('',(#3512),#2305,.T.);
#26326=ADVANCED_FACE('',(#3513),#2306,.T.);
#26327=ADVANCED_FACE('',(#3514),#2307,.T.);
#26328=ADVANCED_FACE('',(#3515),#2308,.T.);
#26329=ADVANCED_FACE('',(#3516),#2309,.T.);
#26330=ADVANCED_FACE('',(#3517),#2310,.T.);
#26331=ADVANCED_FACE('',(#3518),#2311,.T.);
#26332=ADVANCED_FACE('',(#3519),#2312,.T.);
#26333=ADVANCED_FACE('',(#3520),#2313,.T.);
#26334=ADVANCED_FACE('',(#3521),#2314,.T.);
#26335=ADVANCED_FACE('',(#3522),#2315,.T.);
#26336=ADVANCED_FACE('',(#3523),#2316,.T.);
#26337=ADVANCED_FACE('',(#3524),#2317,.T.);
#26338=ADVANCED_FACE('',(#3525),#2318,.T.);
#26339=ADVANCED_FACE('',(#3526),#2319,.T.);
#26340=ADVANCED_FACE('',(#3527),#2320,.T.);
#26341=ADVANCED_FACE('',(#3528),#2321,.T.);
#26342=ADVANCED_FACE('',(#3529),#2322,.T.);
#26343=ADVANCED_FACE('',(#3530),#2323,.T.);
#26344=ADVANCED_FACE('',(#3531),#2324,.T.);
#26345=ADVANCED_FACE('',(#3532),#2325,.T.);
#26346=ADVANCED_FACE('',(#3533),#2326,.T.);
#26347=ADVANCED_FACE('',(#3534),#2327,.T.);
#26348=ADVANCED_FACE('',(#3535),#2328,.T.);
#26349=ADVANCED_FACE('',(#3536),#2329,.T.);
#26350=ADVANCED_FACE('',(#3537),#2330,.T.);
#26351=ADVANCED_FACE('',(#3538),#2331,.T.);
#26352=ADVANCED_FACE('',(#3539),#2332,.T.);
#26353=ADVANCED_FACE('',(#3540),#2333,.T.);
#26354=ADVANCED_FACE('',(#3541),#2334,.T.);
#26355=ADVANCED_FACE('',(#3542),#2335,.T.);
#26356=ADVANCED_FACE('',(#3543),#2336,.T.);
#26357=ADVANCED_FACE('',(#3544),#2337,.T.);
#26358=ADVANCED_FACE('',(#3545),#2338,.T.);
#26359=ADVANCED_FACE('',(#3546),#2339,.T.);
#26360=ADVANCED_FACE('',(#3547),#2340,.T.);
#26361=ADVANCED_FACE('',(#3548),#2341,.T.);
#26362=ADVANCED_FACE('',(#3549),#2342,.T.);
#26363=ADVANCED_FACE('',(#3550),#2343,.T.);
#26364=ADVANCED_FACE('',(#3551),#2344,.T.);
#26365=ADVANCED_FACE('',(#3552),#2345,.T.);
#26366=ADVANCED_FACE('',(#3553),#2346,.T.);
#26367=ADVANCED_FACE('',(#3554),#2347,.T.);
#26368=ADVANCED_FACE('',(#3555),#2348,.T.);
#26369=ADVANCED_FACE('',(#3556),#2349,.T.);
#26370=ADVANCED_FACE('',(#3557),#2350,.T.);
#26371=ADVANCED_FACE('',(#3558),#2351,.T.);
#26372=ADVANCED_FACE('',(#3559),#2352,.T.);
#26373=ADVANCED_FACE('',(#3560),#2353,.T.);
#26374=ADVANCED_FACE('',(#3561),#2354,.T.);
#26375=ADVANCED_FACE('',(#3562),#2355,.T.);
#26376=ADVANCED_FACE('',(#3563),#2356,.T.);
#26377=ADVANCED_FACE('',(#3564),#2357,.T.);
#26378=ADVANCED_FACE('',(#3565),#2358,.T.);
#26379=ADVANCED_FACE('',(#3566),#2359,.T.);
#26380=ADVANCED_FACE('',(#3567),#2360,.T.);
#26381=ADVANCED_FACE('',(#3568),#2361,.T.);
#26382=ADVANCED_FACE('',(#3569),#2362,.T.);
#26383=ADVANCED_FACE('',(#3570),#2363,.T.);
#26384=ADVANCED_FACE('',(#3571),#2364,.T.);
#26385=ADVANCED_FACE('',(#3572),#2365,.T.);
#26386=ADVANCED_FACE('',(#3573),#2366,.T.);
#26387=ADVANCED_FACE('',(#3574),#2367,.T.);
#26388=ADVANCED_FACE('',(#3575),#2368,.T.);
#26389=ADVANCED_FACE('',(#3576),#2369,.T.);
#26390=ADVANCED_FACE('',(#3577),#2370,.T.);
#26391=ADVANCED_FACE('',(#3578),#2371,.T.);
#26392=ADVANCED_FACE('',(#3579),#2372,.T.);
#26393=ADVANCED_FACE('',(#3580),#286,.T.);
#26394=ADVANCED_FACE('',(#3581),#728,.F.);
#26395=ADVANCED_FACE('',(#3582,#877),#729,.F.);
#26396=ADVANCED_FACE('',(#3583),#25344,.F.);
#26397=ADVANCED_FACE('',(#3584),#25345,.F.);
#26398=ADVANCED_FACE('',(#3585),#25346,.F.);
#26399=ADVANCED_FACE('',(#3586),#2373,.T.);
#26400=ADVANCED_FACE('',(#3587),#2374,.T.);
#26401=ADVANCED_FACE('',(#3588),#2375,.T.);
#26402=ADVANCED_FACE('',(#3589),#2376,.T.);
#26403=ADVANCED_FACE('',(#3590),#2377,.T.);
#26404=ADVANCED_FACE('',(#3591),#2378,.T.);
#26405=ADVANCED_FACE('',(#3592),#2379,.T.);
#26406=ADVANCED_FACE('',(#3593),#2380,.T.);
#26407=ADVANCED_FACE('',(#3594),#2381,.T.);
#26408=ADVANCED_FACE('',(#3595),#2382,.T.);
#26409=ADVANCED_FACE('',(#3596),#2383,.T.);
#26410=ADVANCED_FACE('',(#3597),#2384,.T.);
#26411=ADVANCED_FACE('',(#3598),#2385,.T.);
#26412=ADVANCED_FACE('',(#3599),#2386,.T.);
#26413=ADVANCED_FACE('',(#3600),#2387,.T.);
#26414=ADVANCED_FACE('',(#3601),#2388,.T.);
#26415=ADVANCED_FACE('',(#3602),#2389,.T.);
#26416=ADVANCED_FACE('',(#3603),#2390,.T.);
#26417=ADVANCED_FACE('',(#3604),#2391,.T.);
#26418=ADVANCED_FACE('',(#3605),#2392,.T.);
#26419=ADVANCED_FACE('',(#3606),#730,.F.);
#26420=ADVANCED_FACE('',(#3607),#2393,.T.);
#26421=ADVANCED_FACE('',(#3608),#2394,.T.);
#26422=ADVANCED_FACE('',(#3609),#731,.F.);
#26423=ADVANCED_FACE('',(#3610),#2395,.T.);
#26424=ADVANCED_FACE('',(#3611),#2396,.T.);
#26425=ADVANCED_FACE('',(#3612),#732,.F.);
#26426=ADVANCED_FACE('',(#3613),#2397,.T.);
#26427=ADVANCED_FACE('',(#3614),#2398,.T.);
#26428=ADVANCED_FACE('',(#3615),#733,.F.);
#26429=ADVANCED_FACE('',(#3616),#2399,.T.);
#26430=ADVANCED_FACE('',(#3617),#2400,.T.);
#26431=ADVANCED_FACE('',(#3618),#734,.F.);
#26432=ADVANCED_FACE('',(#3619),#2401,.T.);
#26433=ADVANCED_FACE('',(#3620),#2402,.T.);
#26434=ADVANCED_FACE('',(#3621),#735,.F.);
#26435=ADVANCED_FACE('',(#3622),#2403,.T.);
#26436=ADVANCED_FACE('',(#3623),#2404,.T.);
#26437=ADVANCED_FACE('',(#3624),#736,.F.);
#26438=ADVANCED_FACE('',(#3625),#2405,.T.);
#26439=ADVANCED_FACE('',(#3626),#2406,.T.);
#26440=ADVANCED_FACE('',(#3627),#737,.F.);
#26441=ADVANCED_FACE('',(#3628),#2407,.T.);
#26442=ADVANCED_FACE('',(#3629),#2408,.F.);
#26443=ADVANCED_FACE('',(#3630),#2409,.T.);
#26444=ADVANCED_FACE('',(#3631),#2410,.F.);
#26445=ADVANCED_FACE('',(#3632),#2411,.T.);
#26446=ADVANCED_FACE('',(#3633),#2412,.F.);
#26447=ADVANCED_FACE('',(#3634),#2413,.T.);
#26448=ADVANCED_FACE('',(#3635),#2414,.T.);
#26449=ADVANCED_FACE('',(#3636),#2415,.F.);
#26450=ADVANCED_FACE('',(#3637),#2416,.F.);
#26451=ADVANCED_FACE('',(#3638),#2417,.T.);
#26452=ADVANCED_FACE('',(#3639),#2418,.T.);
#26453=ADVANCED_FACE('',(#3640),#2419,.F.);
#26454=ADVANCED_FACE('',(#3641),#2420,.F.);
#26455=ADVANCED_FACE('',(#3642),#2421,.T.);
#26456=ADVANCED_FACE('',(#3643),#2422,.T.);
#26457=ADVANCED_FACE('',(#3644),#2423,.F.);
#26458=ADVANCED_FACE('',(#3645),#738,.F.);
#26459=ADVANCED_FACE('',(#3646,#878),#2424,.F.);
#26460=ADVANCED_FACE('',(#3647),#739,.F.);
#26461=ADVANCED_FACE('',(#3648),#25347,.F.);
#26462=ADVANCED_FACE('',(#3649,#879),#2425,.T.);
#26463=ADVANCED_FACE('',(#3650),#25348,.T.);
#26464=ADVANCED_FACE('',(#3651,#880,#881,#882,#883,#884,#885,#886),#740,
 .T.);
#26465=ADVANCED_FACE('',(#3652),#135,.T.);
#26466=ADVANCED_FACE('',(#3653),#143,.T.);
#26467=ADVANCED_FACE('',(#3654),#741,.T.);
#26468=ADVANCED_FACE('',(#3655),#742,.T.);
#26469=ADVANCED_FACE('',(#3656),#144,.T.);
#26470=ADVANCED_FACE('',(#3657),#2426,.F.);
#26471=ADVANCED_FACE('',(#3658),#2427,.F.);
#26472=ADVANCED_FACE('',(#3659),#743,.F.);
#26473=ADVANCED_FACE('',(#3660),#744,.T.);
#26474=ADVANCED_FACE('',(#3661),#2428,.F.);
#26475=ADVANCED_FACE('',(#3662),#2429,.T.);
#26476=ADVANCED_FACE('',(#3663),#2430,.T.);
#26477=ADVANCED_FACE('',(#3664),#745,.T.);
#26478=ADVANCED_FACE('',(#3665),#2431,.T.);
#26479=ADVANCED_FACE('',(#3666),#2432,.F.);
#26480=ADVANCED_FACE('',(#3667),#746,.T.);
#26481=ADVANCED_FACE('',(#3668),#136,.T.);
#26482=ADVANCED_FACE('',(#3669),#747,.T.);
#26483=ADVANCED_FACE('',(#3670),#137,.T.);
#26484=ADVANCED_FACE('',(#3671),#748,.T.);
#26485=ADVANCED_FACE('',(#3672),#749,.T.);
#26486=ADVANCED_FACE('',(#3673),#750,.T.);
#26487=ADVANCED_FACE('',(#3674),#751,.T.);
#26488=ADVANCED_FACE('',(#3675),#752,.T.);
#26489=ADVANCED_FACE('',(#3676),#145,.T.);
#26490=ADVANCED_FACE('',(#3677),#753,.T.);
#26491=ADVANCED_FACE('',(#3678),#754,.T.);
#26492=ADVANCED_FACE('',(#3679),#755,.T.);
#26493=ADVANCED_FACE('',(#3680),#756,.T.);
#26494=ADVANCED_FACE('',(#3681),#2433,.T.);
#26495=ADVANCED_FACE('',(#3682,#887,#888,#889,#890),#2434,.F.);
#26496=ADVANCED_FACE('',(#3683,#891),#2435,.F.);
#26497=ADVANCED_FACE('',(#3684),#2436,.F.);
#26498=ADVANCED_FACE('',(#3685),#2437,.F.);
#26499=ADVANCED_FACE('',(#3686),#146,.T.);
#26500=ADVANCED_FACE('',(#3687),#757,.F.);
#26501=ADVANCED_FACE('',(#3688,#892),#2438,.F.);
#26502=ADVANCED_FACE('',(#3689),#147,.T.);
#26503=ADVANCED_FACE('',(#3690),#148,.T.);
#26504=ADVANCED_FACE('',(#3691),#758,.F.);
#26505=ADVANCED_FACE('',(#3692,#893),#2439,.F.);
#26506=ADVANCED_FACE('',(#3693),#149,.T.);
#26507=ADVANCED_FACE('',(#3694),#150,.T.);
#26508=ADVANCED_FACE('',(#3695),#759,.F.);
#26509=ADVANCED_FACE('',(#3696),#151,.T.);
#26510=ADVANCED_FACE('',(#3697),#760,.F.);
#26511=ADVANCED_FACE('',(#3698),#138,.T.);
#26512=ADVANCED_FACE('',(#3699),#139,.T.);
#26513=ADVANCED_FACE('',(#3700),#761,.T.);
#26514=ADVANCED_FACE('',(#3701),#762,.T.);
#26515=ADVANCED_FACE('',(#3702),#152,.T.);
#26516=ADVANCED_FACE('',(#3703),#153,.T.);
#26517=ADVANCED_FACE('',(#3704),#763,.T.);
#26518=ADVANCED_FACE('',(#3705),#2440,.F.);
#26519=ADVANCED_FACE('',(#3706),#2441,.T.);
#26520=ADVANCED_FACE('',(#3707),#764,.T.);
#26521=ADVANCED_FACE('',(#3708),#765,.T.);
#26522=ADVANCED_FACE('',(#3709),#140,.T.);
#26523=ADVANCED_FACE('',(#3710),#766,.F.);
#26524=ADVANCED_FACE('',(#3711),#2442,.T.);
#26525=ADVANCED_FACE('',(#3712),#154,.T.);
#26526=ADVANCED_FACE('',(#3713,#894),#767,.T.);
#26527=ADVANCED_FACE('',(#3714),#768,.T.);
#26528=ADVANCED_FACE('',(#3715),#769,.T.);
#26529=ADVANCED_FACE('',(#3716),#141,.T.);
#26530=ADVANCED_FACE('',(#3717),#155,.T.);
#26531=ADVANCED_FACE('',(#3718),#2443,.F.);
#26532=ADVANCED_FACE('',(#3719),#770,.F.);
#26533=ADVANCED_FACE('',(#3720),#771,.T.);
#26534=ADVANCED_FACE('',(#3721),#2444,.F.);
#26535=ADVANCED_FACE('',(#3722),#156,.T.);
#26536=ADVANCED_FACE('',(#3723,#895,#896,#897),#2445,.T.);
#26537=ADVANCED_FACE('',(#3724),#772,.F.);
#26538=ADVANCED_FACE('',(#3725),#157,.T.);
#26539=ADVANCED_FACE('',(#3726),#773,.F.);
#26540=ADVANCED_FACE('',(#3727),#158,.T.);
#26541=ADVANCED_FACE('',(#3728),#774,.F.);
#26542=ADVANCED_FACE('',(#3729),#159,.T.);
#26543=ADVANCED_FACE('',(#3730),#775,.T.);
#26544=ADVANCED_FACE('',(#3731),#776,.F.);
#26545=ADVANCED_FACE('',(#3732),#777,.T.);
#26546=ADVANCED_FACE('',(#3733,#898,#899,#900,#901),#2446,.F.);
#26547=ADVANCED_FACE('',(#3734),#160,.T.);
#26548=ADVANCED_FACE('',(#3735),#778,.F.);
#26549=ADVANCED_FACE('',(#3736),#161,.T.);
#26550=ADVANCED_FACE('',(#3737),#779,.F.);
#26551=ADVANCED_FACE('',(#3738),#2447,.T.);
#26552=ADVANCED_FACE('',(#3739),#162,.T.);
#26553=ADVANCED_FACE('',(#3740),#2448,.F.);
#26554=ADVANCED_FACE('',(#3741),#2449,.T.);
#26555=ADVANCED_FACE('',(#3742),#163,.T.);
#26556=ADVANCED_FACE('',(#3743,#902,#903,#904,#905,#906,#907),#2450,.T.);
#26557=ADVANCED_FACE('',(#3744),#780,.T.);
#26558=ADVANCED_FACE('',(#3745),#164,.T.);
#26559=ADVANCED_FACE('',(#3746),#165,.T.);
#26560=ADVANCED_FACE('',(#3747),#166,.T.);
#26561=ADVANCED_FACE('',(#3748),#167,.T.);
#26562=ADVANCED_FACE('',(#3749),#781,.T.);
#26563=ADVANCED_FACE('',(#3750),#782,.T.);
#26564=ADVANCED_FACE('',(#3751),#2451,.T.);
#26565=ADVANCED_FACE('',(#3752),#25349,.F.);
#26566=ADVANCED_FACE('',(#3753),#2452,.F.);
#26567=ADVANCED_FACE('',(#3754),#2453,.T.);
#26568=ADVANCED_FACE('',(#3755),#168,.T.);
#26569=ADVANCED_FACE('',(#3756),#2454,.F.);
#26570=ADVANCED_FACE('',(#3757),#169,.T.);
#26571=ADVANCED_FACE('',(#3758),#2455,.F.);
#26572=ADVANCED_FACE('',(#3759),#783,.T.);
#26573=ADVANCED_FACE('',(#3760),#2456,.T.);
#26574=ADVANCED_FACE('',(#3761),#2457,.T.);
#26575=ADVANCED_FACE('',(#3762),#2458,.T.);
#26576=ADVANCED_FACE('',(#3763),#25350,.T.);
#26577=ADVANCED_FACE('',(#3764),#25351,.T.);
#26578=ADVANCED_FACE('',(#3765,#908,#909,#910,#911,#912),#2459,.F.);
#26579=ADVANCED_FACE('',(#3766),#784,.F.);
#26580=ADVANCED_FACE('',(#3767),#2460,.F.);
#26581=ADVANCED_FACE('',(#3768),#2461,.T.);
#26582=ADVANCED_FACE('',(#3769),#2462,.T.);
#26583=ADVANCED_FACE('',(#3770),#785,.F.);
#26584=ADVANCED_FACE('',(#3771),#25352,.T.);
#26585=ADVANCED_FACE('',(#3772,#913),#2463,.T.);
#26586=ADVANCED_FACE('',(#3773),#25353,.T.);
#26587=ADVANCED_FACE('',(#3774),#786,.F.);
#26588=ADVANCED_FACE('',(#3775),#2464,.T.);
#26589=ADVANCED_FACE('',(#3776),#787,.F.);
#26590=ADVANCED_FACE('',(#3777),#788,.F.);
#26591=ADVANCED_FACE('',(#3778),#2465,.T.);
#26592=ADVANCED_FACE('',(#3779),#2466,.F.);
#26593=ADVANCED_FACE('',(#3780),#2467,.F.);
#26594=ADVANCED_FACE('',(#3781),#2468,.T.);
#26595=ADVANCED_FACE('',(#3782),#789,.F.);
#26596=ADVANCED_FACE('',(#3783),#790,.F.);
#26597=ADVANCED_FACE('',(#3784),#2469,.T.);
#26598=ADVANCED_FACE('',(#3785),#25354,.T.);
#26599=ADVANCED_FACE('',(#3786),#25355,.F.);
#26600=ADVANCED_FACE('',(#3787),#25356,.F.);
#26601=ADVANCED_FACE('',(#3788),#2470,.T.);
#26602=ADVANCED_FACE('',(#3789),#791,.F.);
#26603=ADVANCED_FACE('',(#3790),#25357,.F.);
#26604=ADVANCED_FACE('',(#3791),#2471,.T.);
#26605=ADVANCED_FACE('',(#3792),#2472,.T.);
#26606=ADVANCED_FACE('',(#3793),#792,.T.);
#26607=ADVANCED_FACE('',(#3794),#793,.T.);
#26608=ADVANCED_FACE('',(#3795),#2473,.T.);
#26609=ADVANCED_FACE('',(#3796),#2474,.T.);
#26610=ADVANCED_FACE('',(#3797),#25358,.F.);
#26611=ADVANCED_FACE('',(#3798),#794,.F.);
#26612=ADVANCED_FACE('',(#3799),#2475,.T.);
#26613=ADVANCED_FACE('',(#3800),#2476,.T.);
#26614=ADVANCED_FACE('',(#3801),#2477,.T.);
#26615=ADVANCED_FACE('',(#3802),#2478,.T.);
#26616=ADVANCED_FACE('',(#3803),#2479,.T.);
#26617=ADVANCED_FACE('',(#3804),#795,.F.);
#26618=ADVANCED_FACE('',(#3805),#2480,.F.);
#26619=ADVANCED_FACE('',(#3806),#796,.F.);
#26620=ADVANCED_FACE('',(#3807),#797,.T.);
#26621=ADVANCED_FACE('',(#3808),#2481,.T.);
#26622=ADVANCED_FACE('',(#3809),#25359,.T.);
#26623=ADVANCED_FACE('',(#3810),#2482,.T.);
#26624=ADVANCED_FACE('',(#3811),#2483,.T.);
#26625=ADVANCED_FACE('',(#3812),#2484,.T.);
#26626=ADVANCED_FACE('',(#3813),#798,.T.);
#26627=ADVANCED_FACE('',(#3814),#799,.T.);
#26628=ADVANCED_FACE('',(#3815),#800,.F.);
#26629=ADVANCED_FACE('',(#3816),#2485,.T.);
#26630=ADVANCED_FACE('',(#3817),#2486,.T.);
#26631=ADVANCED_FACE('',(#3818),#25360,.F.);
#26632=ADVANCED_FACE('',(#3819),#2487,.T.);
#26633=ADVANCED_FACE('',(#3820),#2488,.T.);
#26634=ADVANCED_FACE('',(#3821),#2489,.T.);
#26635=ADVANCED_FACE('',(#3822),#2490,.T.);
#26636=ADVANCED_FACE('',(#3823),#287,.T.);
#26637=ADVANCED_FACE('',(#3824),#288,.T.);
#26638=ADVANCED_FACE('',(#3825),#2491,.T.);
#26639=ADVANCED_FACE('',(#3826),#289,.T.);
#26640=ADVANCED_FACE('',(#3827),#290,.T.);
#26641=ADVANCED_FACE('',(#3828),#2492,.T.);
#26642=ADVANCED_FACE('',(#3829),#2493,.F.);
#26643=ADVANCED_FACE('',(#3830),#2494,.T.);
#26644=ADVANCED_FACE('',(#3831),#2495,.T.);
#26645=ADVANCED_FACE('',(#3832),#2496,.T.);
#26646=ADVANCED_FACE('',(#3833),#2497,.T.);
#26647=ADVANCED_FACE('',(#3834),#2498,.T.);
#26648=ADVANCED_FACE('',(#3835),#2499,.T.);
#26649=ADVANCED_FACE('',(#3836),#2500,.T.);
#26650=ADVANCED_FACE('',(#3837),#2501,.T.);
#26651=ADVANCED_FACE('',(#3838),#2502,.T.);
#26652=ADVANCED_FACE('',(#3839),#2503,.T.);
#26653=ADVANCED_FACE('',(#3840),#2504,.T.);
#26654=ADVANCED_FACE('',(#3841),#291,.T.);
#26655=ADVANCED_FACE('',(#3842),#292,.T.);
#26656=ADVANCED_FACE('',(#3843),#293,.T.);
#26657=ADVANCED_FACE('',(#3844),#294,.T.);
#26658=ADVANCED_FACE('',(#3845),#295,.T.);
#26659=ADVANCED_FACE('',(#3846),#296,.T.);
#26660=ADVANCED_FACE('',(#3847),#297,.T.);
#26661=ADVANCED_FACE('',(#3848),#298,.T.);
#26662=ADVANCED_FACE('',(#3849),#299,.T.);
#26663=ADVANCED_FACE('',(#3850),#300,.T.);
#26664=ADVANCED_FACE('',(#3851),#301,.T.);
#26665=ADVANCED_FACE('',(#3852),#302,.T.);
#26666=ADVANCED_FACE('',(#3853),#303,.T.);
#26667=ADVANCED_FACE('',(#3854),#304,.T.);
#26668=ADVANCED_FACE('',(#3855),#305,.T.);
#26669=ADVANCED_FACE('',(#3856),#306,.T.);
#26670=ADVANCED_FACE('',(#3857),#307,.T.);
#26671=ADVANCED_FACE('',(#3858),#308,.T.);
#26672=ADVANCED_FACE('',(#3859,#914),#2505,.F.);
#26673=ADVANCED_FACE('',(#3860),#2506,.T.);
#26674=ADVANCED_FACE('',(#3861),#2507,.T.);
#26675=ADVANCED_FACE('',(#3862),#2508,.T.);
#26676=ADVANCED_FACE('',(#3863),#2509,.T.);
#26677=ADVANCED_FACE('',(#3864),#2510,.T.);
#26678=ADVANCED_FACE('',(#3865,#915),#2511,.F.);
#26679=ADVANCED_FACE('',(#3866),#801,.F.);
#26680=ADVANCED_FACE('',(#3867,#916),#2512,.F.);
#26681=ADVANCED_FACE('',(#3868),#802,.F.);
#26682=ADVANCED_FACE('',(#3869),#803,.F.);
#26683=ADVANCED_FACE('',(#3870),#804,.F.);
#26684=ADVANCED_FACE('',(#3871),#2513,.F.);
#26685=ADVANCED_FACE('',(#3872),#2514,.F.);
#26686=ADVANCED_FACE('',(#3873),#2515,.F.);
#26687=ADVANCED_FACE('',(#3874),#805,.F.);
#26688=ADVANCED_FACE('',(#3875),#2516,.T.);
#26689=ADVANCED_FACE('',(#3876),#2517,.T.);
#26690=ADVANCED_FACE('',(#3877),#2518,.T.);
#26691=ADVANCED_FACE('',(#3878),#2519,.T.);
#26692=ADVANCED_FACE('',(#3879),#2520,.F.);
#26693=ADVANCED_FACE('',(#3880),#2521,.T.);
#26694=ADVANCED_FACE('',(#3881),#2522,.T.);
#26695=ADVANCED_FACE('',(#3882),#2523,.F.);
#26696=ADVANCED_FACE('',(#3883),#25361,.F.);
#26697=ADVANCED_FACE('',(#3884,#917),#2524,.T.);
#26698=ADVANCED_FACE('',(#3885),#25362,.F.);
#26699=ADVANCED_FACE('',(#3886,#918),#2525,.F.);
#26700=ADVANCED_FACE('',(#3887),#25363,.T.);
#26701=ADVANCED_FACE('',(#3888),#806,.T.);
#26702=ADVANCED_FACE('',(#3889),#2526,.F.);
#26703=ADVANCED_FACE('',(#3890),#25364,.T.);
#26704=ADVANCED_FACE('',(#3891),#25365,.T.);
#26705=ADVANCED_FACE('',(#3892),#807,.T.);
#26706=ADVANCED_FACE('',(#3893),#25366,.T.);
#26707=ADVANCED_FACE('',(#3894),#2527,.T.);
#26708=ADVANCED_FACE('',(#3895),#25367,.T.);
#26709=ADVANCED_FACE('',(#3896),#2528,.T.);
#26710=ADVANCED_FACE('',(#3897),#25368,.F.);
#26711=ADVANCED_FACE('',(#3898),#2529,.T.);
#26712=ADVANCED_FACE('',(#3899),#2530,.T.);
#26713=ADVANCED_FACE('',(#3900),#25369,.T.);
#26714=ADVANCED_FACE('',(#3901),#2531,.T.);
#26715=ADVANCED_FACE('',(#3902),#2532,.T.);
#26716=ADVANCED_FACE('',(#3903),#25370,.F.);
#26717=ADVANCED_FACE('',(#3904),#808,.F.);
#26718=ADVANCED_FACE('',(#3905),#809,.F.);
#26719=ADVANCED_FACE('',(#3906),#2533,.T.);
#26720=ADVANCED_FACE('',(#3907),#25371,.F.);
#26721=ADVANCED_FACE('',(#3908),#2534,.T.);
#26722=ADVANCED_FACE('',(#3909),#2535,.T.);
#26723=ADVANCED_FACE('',(#3910),#2536,.T.);
#26724=ADVANCED_FACE('',(#3911),#25372,.F.);
#26725=ADVANCED_FACE('',(#3912),#2537,.T.);
#26726=ADVANCED_FACE('',(#3913),#2538,.T.);
#26727=ADVANCED_FACE('',(#3914),#25373,.T.);
#26728=ADVANCED_FACE('',(#3915),#2539,.T.);
#26729=ADVANCED_FACE('',(#3916),#25374,.T.);
#26730=ADVANCED_FACE('',(#3917),#25375,.T.);
#26731=ADVANCED_FACE('',(#3918),#2540,.T.);
#26732=ADVANCED_FACE('',(#3919),#25376,.T.);
#26733=ADVANCED_FACE('',(#3920),#810,.T.);
#26734=ADVANCED_FACE('',(#3921),#2541,.T.);
#26735=ADVANCED_FACE('',(#3922),#811,.T.);
#26736=ADVANCED_FACE('',(#3923),#2542,.T.);
#26737=ADVANCED_FACE('',(#3924),#2543,.T.);
#26738=ADVANCED_FACE('',(#3925),#25377,.T.);
#26739=ADVANCED_FACE('',(#3926),#25378,.T.);
#26740=ADVANCED_FACE('',(#3927),#2544,.T.);
#26741=ADVANCED_FACE('',(#3928),#25379,.T.);
#26742=ADVANCED_FACE('',(#3929),#2545,.T.);
#26743=ADVANCED_FACE('',(#3930),#25380,.T.);
#26744=ADVANCED_FACE('',(#3931),#2546,.T.);
#26745=ADVANCED_FACE('',(#3932),#812,.T.);
#26746=ADVANCED_FACE('',(#3933),#813,.T.);
#26747=ADVANCED_FACE('',(#3934),#2547,.T.);
#26748=ADVANCED_FACE('',(#3935),#814,.T.);
#26749=ADVANCED_FACE('',(#3936),#815,.T.);
#26750=ADVANCED_FACE('',(#3937),#816,.T.);
#26751=ADVANCED_FACE('',(#3938),#817,.T.);
#26752=ADVANCED_FACE('',(#3939),#818,.T.);
#26753=ADVANCED_FACE('',(#3940),#819,.T.);
#26754=ADVANCED_FACE('',(#3941),#820,.T.);
#26755=ADVANCED_FACE('',(#3942),#821,.T.);
#26756=ADVANCED_FACE('',(#3943),#822,.T.);
#26757=ADVANCED_FACE('',(#3944),#823,.T.);
#26758=ADVANCED_FACE('',(#3945),#824,.T.);
#26759=ADVANCED_FACE('',(#3946),#825,.T.);
#26760=ADVANCED_FACE('',(#3947),#826,.T.);
#26761=ADVANCED_FACE('',(#3948),#827,.T.);
#26762=ADVANCED_FACE('',(#3949),#828,.T.);
#26763=ADVANCED_FACE('',(#3950),#829,.T.);
#26764=ADVANCED_FACE('',(#3951),#830,.T.);
#26765=ADVANCED_FACE('',(#3952),#831,.T.);
#26766=ADVANCED_FACE('',(#3953),#832,.T.);
#26767=ADVANCED_FACE('',(#3954),#833,.T.);
#26768=ADVANCED_FACE('',(#3955),#834,.T.);
#26769=ADVANCED_FACE('',(#3956),#835,.T.);
#26770=ADVANCED_FACE('',(#3957),#836,.T.);
#26771=ADVANCED_FACE('',(#3958),#837,.T.);
#26772=ADVANCED_FACE('',(#3959),#838,.T.);
#26773=ADVANCED_FACE('',(#3960),#839,.T.);
#26774=ADVANCED_FACE('',(#3961),#840,.T.);
#26775=ADVANCED_FACE('',(#3962),#841,.T.);
#26776=ADVANCED_FACE('',(#3963),#842,.T.);
#26777=ADVANCED_FACE('',(#3964),#309,.F.);
#26778=ADVANCED_FACE('',(#3965),#310,.F.);
#26779=ADVANCED_FACE('',(#3966),#311,.F.);
#26780=ADVANCED_FACE('',(#3967),#312,.F.);
#26781=ADVANCED_FACE('',(#3968),#313,.F.);
#26782=ADVANCED_FACE('',(#3969),#314,.F.);
#26783=ADVANCED_FACE('',(#3970),#315,.F.);
#26784=ADVANCED_FACE('',(#3971),#316,.F.);
#26785=ADVANCED_FACE('',(#3972),#317,.F.);
#26786=ADVANCED_FACE('',(#3973),#318,.F.);
#26787=ADVANCED_FACE('',(#3974),#319,.F.);
#26788=ADVANCED_FACE('',(#3975),#320,.F.);
#26789=ADVANCED_FACE('',(#3976),#321,.F.);
#26790=ADVANCED_FACE('',(#3977),#322,.F.);
#26791=ADVANCED_FACE('',(#3978),#323,.F.);
#26792=ADVANCED_FACE('',(#3979),#324,.F.);
#26793=ADVANCED_FACE('',(#3980),#325,.F.);
#26794=ADVANCED_FACE('',(#3981),#326,.F.);
#26795=ADVANCED_FACE('',(#3982),#327,.F.);
#26796=ADVANCED_FACE('',(#3983),#328,.F.);
#26797=ADVANCED_FACE('',(#3984),#329,.F.);
#26798=ADVANCED_FACE('',(#3985),#330,.F.);
#26799=ADVANCED_FACE('',(#3986),#331,.F.);
#26800=ADVANCED_FACE('',(#3987),#332,.F.);
#26801=ADVANCED_FACE('',(#3988),#333,.F.);
#26802=ADVANCED_FACE('',(#3989),#334,.F.);
#26803=ADVANCED_FACE('',(#3990),#335,.F.);
#26804=ADVANCED_FACE('',(#3991),#336,.F.);
#26805=ADVANCED_FACE('',(#3992),#337,.F.);
#26806=ADVANCED_FACE('',(#3993),#338,.F.);
#26807=ADVANCED_FACE('',(#3994),#339,.F.);
#26808=ADVANCED_FACE('',(#3995),#340,.F.);
#26809=ADVANCED_FACE('',(#3996),#341,.F.);
#26810=ADVANCED_FACE('',(#3997,#919,#920),#2548,.T.);
#26811=ADVANCED_FACE('',(#3998),#2549,.F.);
#26812=ADVANCED_FACE('',(#3999),#2550,.F.);
#26813=ADVANCED_FACE('',(#4000),#2551,.F.);
#26814=ADVANCED_FACE('',(#4001),#2552,.F.);
#26815=ADVANCED_FACE('',(#4002),#2553,.F.);
#26816=ADVANCED_FACE('',(#4003),#342,.F.);
#26817=ADVANCED_FACE('',(#4004),#343,.F.);
#26818=ADVANCED_FACE('',(#4005),#344,.F.);
#26819=ADVANCED_FACE('',(#4006),#345,.F.);
#26820=ADVANCED_FACE('',(#4007),#346,.F.);
#26821=ADVANCED_FACE('',(#4008),#347,.F.);
#26822=ADVANCED_FACE('',(#4009),#348,.F.);
#26823=ADVANCED_FACE('',(#4010),#349,.F.);
#26824=ADVANCED_FACE('',(#4011),#350,.F.);
#26825=ADVANCED_FACE('',(#4012),#351,.F.);
#26826=ADVANCED_FACE('',(#4013),#352,.F.);
#26827=ADVANCED_FACE('',(#4014),#353,.F.);
#26828=ADVANCED_FACE('',(#4015),#354,.F.);
#26829=ADVANCED_FACE('',(#4016),#355,.F.);
#26830=ADVANCED_FACE('',(#4017),#356,.F.);
#26831=ADVANCED_FACE('',(#4018),#357,.F.);
#26832=ADVANCED_FACE('',(#4019),#358,.F.);
#26833=ADVANCED_FACE('',(#4020),#359,.F.);
#26834=ADVANCED_FACE('',(#4021),#360,.F.);
#26835=ADVANCED_FACE('',(#4022),#361,.F.);
#26836=ADVANCED_FACE('',(#4023),#362,.F.);
#26837=ADVANCED_FACE('',(#4024),#363,.F.);
#26838=ADVANCED_FACE('',(#4025),#364,.F.);
#26839=ADVANCED_FACE('',(#4026),#365,.F.);
#26840=ADVANCED_FACE('',(#4027),#366,.F.);
#26841=ADVANCED_FACE('',(#4028),#367,.F.);
#26842=ADVANCED_FACE('',(#4029),#368,.F.);
#26843=ADVANCED_FACE('',(#4030),#369,.F.);
#26844=ADVANCED_FACE('',(#4031),#370,.F.);
#26845=ADVANCED_FACE('',(#4032),#371,.F.);
#26846=ADVANCED_FACE('',(#4033),#372,.F.);
#26847=ADVANCED_FACE('',(#4034),#373,.F.);
#26848=ADVANCED_FACE('',(#4035),#374,.F.);
#26849=ADVANCED_FACE('',(#4036,#921,#922),#2554,.T.);
#26850=ADVANCED_FACE('',(#4037),#2555,.T.);
#26851=ADVANCED_FACE('',(#4038),#2556,.T.);
#26852=ADVANCED_FACE('',(#4039),#2557,.T.);
#26853=ADVANCED_FACE('',(#4040),#2558,.T.);
#26854=ADVANCED_FACE('',(#4041),#2559,.F.);
#26855=ADVANCED_FACE('',(#4042),#375,.F.);
#26856=ADVANCED_FACE('',(#4043),#2560,.T.);
#26857=ADVANCED_FACE('',(#4044),#843,.T.);
#26858=ADVANCED_FACE('',(#4045),#376,.F.);
#26859=ADVANCED_FACE('',(#4046),#170,.F.);
#26860=ADVANCED_FACE('',(#4047,#923),#2561,.F.);
#26861=ADVANCED_FACE('',(#4048),#844,.T.);
#26862=ADVANCED_FACE('',(#4049),#25381,.T.);
#26863=ADVANCED_FACE('',(#4050),#2562,.T.);
#26864=ADVANCED_FACE('',(#4051),#2563,.T.);
#26865=ADVANCED_FACE('',(#4052),#2564,.T.);
#26866=ADVANCED_FACE('',(#4053),#2565,.T.);
#26867=ADVANCED_FACE('',(#4054),#2566,.T.);
#26868=ADVANCED_FACE('',(#4055),#2567,.T.);
#26869=ADVANCED_FACE('',(#4056,#924,#925,#926),#2568,.T.);
#26870=ADVANCED_FACE('',(#4057),#2569,.T.);
#26871=ADVANCED_FACE('',(#4058),#25382,.T.);
#26872=CLOSED_SHELL('',(#25383,#25384,#25385,#25386,#25387,#25388,#25389,
#25390,#25391,#25392,#25393,#25394,#25395,#25396,#25397,#25398,#25399,#25400,
#25401,#25402,#25403,#25404,#25405,#25406,#25407,#25408,#25409,#25410,#25411,
#25412,#25413,#25414,#25415,#25416,#25417,#25418,#25419,#25420,#25421,#25422,
#25423,#25424,#25425,#25426,#25427,#25428,#25429,#25430,#25431,#25432,#25433,
#25434,#25435,#25436,#25437,#25438,#25439,#25440,#25441,#25442,#25443,#25444,
#25445,#25446,#25447,#25448,#25449,#25450,#25451,#25452,#25453,#25454,#25455,
#25456,#25457,#25458,#25459,#25460,#25461,#25462,#25463,#25464,#25465,#25466,
#25467,#25468,#25469,#25470,#25471,#25472,#25473,#25474,#25475,#25476,#25477,
#25478,#25479,#25480,#25481,#25482,#25483,#25484,#25485,#25486,#25487,#25488,
#25489,#25490,#25491,#25492,#25493,#25494,#25495,#25496,#25497,#25498,#25499,
#25500,#25501,#25502,#25503,#25504,#25505,#25506));
#26873=CLOSED_SHELL('',(#25507,#25508,#25509,#25510,#25511,#25512,#25513,
#25514,#25515,#25516,#25517,#25518,#25519,#25520,#25521,#25522,#25523,#25524,
#25525,#25526,#25527,#25528,#25529,#25530,#25531,#25532,#25533,#25534,#25535,
#25536,#25537,#25538,#25539,#25540,#25541,#25542,#25543,#25544,#25545));
#26874=CLOSED_SHELL('',(#25546,#25547,#25548,#25549,#25550,#25551,#25552,
#25553,#25554,#25555,#25556,#25557,#25558,#25559,#25560,#25561,#25562,#25563,
#25564,#25565,#25566,#25567,#25568,#25569,#25570,#25571,#25572,#25573,#25574,
#25575,#25576,#25577,#25578,#25579,#25580,#25581,#25582,#25583,#25584,#25585,
#25586,#25587,#25588,#25589,#25590,#25591,#25592,#25593,#25594,#25595,#25596,
#25597,#25598,#25599,#25600,#25601,#25602,#25603,#25604,#25605,#25606,#25607,
#25608,#25609,#25610));
#26875=CLOSED_SHELL('',(#25611,#25612,#25613,#25614,#25615));
#26876=CLOSED_SHELL('',(#25616,#25617,#25618,#25619,#25620,#25621,#25622,
#25623,#25624,#25625,#25626,#25627,#25628,#25629,#25630,#25631,#25632,#25633));
#26877=CLOSED_SHELL('',(#25634,#25635,#25636,#25637,#25638,#25639,#25640,
#25641,#25642,#25643,#25644,#25645,#25646,#25647,#25648,#25649,#25650,#25651,
#25652,#25653,#25654,#25655,#25656,#25657,#25658,#25659,#25660,#25661,#25662,
#25663,#25664,#25665,#25666,#25667,#25668,#25669,#25670,#25671,#25672,#25673,
#25674,#25675,#25676,#25677,#25678,#25679,#25680,#25681,#25682,#25683,#25684,
#25685,#25686,#25687,#25688));
#26878=CLOSED_SHELL('',(#25689,#25690,#25691,#25692,#25693,#25694,#25695,
#25696,#25697,#25698,#25699,#25700,#25701,#25702,#25703,#25704,#25705,#25706,
#25707,#25708,#25709,#25710,#25711,#25712,#25713,#25714,#25715,#25716,#25717,
#25718,#25719,#25720,#25721,#25722,#25723,#25724));
#26879=CLOSED_SHELL('',(#25725,#25726,#25727,#25728,#25729,#25730,#25731,
#25732,#25733,#25734,#25735,#25736,#25737,#25738,#25739,#25740,#25741,#25742,
#25743,#25744,#25745,#25746,#25747,#25748,#25749,#25750,#25751,#25752,#25753,
#25754,#25755,#25756,#25757,#25758,#25759,#25760,#25761,#25762,#25763,#25764,
#25765,#25766,#25767,#25768,#25769,#25770,#25771,#25772,#25773,#25774,#25775,
#25776,#25777,#25778,#25779,#25780,#25781,#25782,#25783,#25784,#25785,#25786,
#25787,#25788,#25789,#25790,#25791,#25792,#25793,#25794,#25795,#25796,#25797,
#25798,#25799,#25800,#25801,#25802,#25803,#25804,#25805,#25806,#25807,#25808,
#25809,#25810,#25811,#25812,#25813,#25814,#25815,#25816,#25817,#25818,#25819,
#25820,#25821,#25822,#25823));
#26880=CLOSED_SHELL('',(#25824,#25825,#25826,#25827,#25828,#25829,#25830,
#25831,#25832,#25833,#25834,#25835,#25836));
#26881=CLOSED_SHELL('',(#25837,#25838,#25839,#25840,#25841,#25842,#25843,
#25844,#25845,#25846,#25847,#25848,#25849,#25850,#25851,#25852,#25853,#25854,
#25855,#25856,#25857,#25858,#25859,#25860,#25861,#25862,#25863,#25864,#25865,
#25866,#25867,#25868,#25869,#25870,#25871,#25872,#25873,#25874,#25875,#25876,
#25877,#25878,#25879,#25880,#25881,#25882,#25883,#25884,#25885,#25886,#25887,
#25888,#25889,#25890,#25891,#25892,#25893,#25894,#25895,#25896,#25897,#25898,
#25899,#25900,#25901,#25902,#25903,#25904,#25905,#25906,#25907,#25908,#25909,
#25910,#25911,#25912,#25913,#25914,#25915));
#26882=CLOSED_SHELL('',(#25916,#25917,#25918,#25919,#25920,#25921,#25922,
#25923,#25924,#25925,#25926,#25927,#25928,#25929,#25930,#25931,#25932,#25933,
#25934,#25935));
#26883=CLOSED_SHELL('',(#25936,#25937,#25938,#25939,#25940,#25941,#25942,
#25943,#25944,#25945,#25946,#25947,#25948,#25949,#25950,#25951,#25952,#25953,
#25954,#25955,#25956,#25957,#25958,#25959,#25960,#25961,#25962,#25963,#25964,
#25965,#25966,#25967,#25968,#25969,#25970,#25971,#25972,#25973,#25974,#25975,
#25976,#25977,#25978,#25979,#25980,#25981,#25982,#25983,#25984,#25985,#25986,
#25987,#25988,#25989,#25990,#25991,#25992,#25993,#25994,#25995,#25996,#25997,
#25998,#25999,#26000,#26001,#26002,#26003,#26004,#26005,#26006,#26007,#26008,
#26009,#26010,#26011,#26012,#26013,#26014,#26015,#26016,#26017,#26018,#26019,
#26020,#26021,#26022,#26023,#26024,#26025,#26026,#26027,#26028,#26029,#26030,
#26031,#26032,#26033,#26034,#26035,#26036,#26037,#26038,#26039,#26040,#26041,
#26042,#26043,#26044,#26045,#26046,#26047,#26048,#26049,#26050,#26051,#26052,
#26053,#26054,#26055,#26056,#26057,#26058,#26059,#26060,#26061,#26062,#26063,
#26064,#26065,#26066,#26067,#26068,#26069,#26070,#26071,#26072,#26073,#26074,
#26075,#26076,#26077,#26078,#26079,#26080,#26081,#26082,#26083,#26084,#26085,
#26086,#26087,#26088,#26089,#26090,#26091,#26092,#26093,#26094,#26095,#26096,
#26097,#26098,#26099,#26100,#26101,#26102,#26103,#26104,#26105,#26106,#26107,
#26108,#26109,#26110,#26111,#26112,#26113,#26114,#26115,#26116,#26117,#26118,
#26119,#26120,#26121,#26122,#26123,#26124,#26125,#26126,#26127,#26128,#26129,
#26130,#26131,#26132,#26133,#26134,#26135,#26136,#26137,#26138,#26139,#26140,
#26141,#26142,#26143,#26144,#26145,#26146,#26147,#26148,#26149,#26150,#26151,
#26152,#26153,#26154,#26155,#26156,#26157,#26158,#26159,#26160,#26161,#26162,
#26163,#26164,#26165,#26166,#26167,#26168,#26169,#26170,#26171,#26172,#26173,
#26174,#26175,#26176,#26177,#26178,#26179,#26180,#26181,#26182,#26183,#26184,
#26185,#26186,#26187,#26188,#26189,#26190,#26191,#26192,#26193,#26194,#26195,
#26196,#26197,#26198,#26199,#26200,#26201,#26202,#26203,#26204,#26205,#26206,
#26207,#26208,#26209,#26210,#26211,#26212,#26213,#26214,#26215,#26216,#26217,
#26218,#26219,#26220,#26221,#26222,#26223,#26224,#26225,#26226,#26227,#26228,
#26229,#26230,#26231,#26232,#26233,#26234,#26235,#26236,#26237,#26238,#26239,
#26240,#26241,#26242,#26243,#26244,#26245,#26246,#26247,#26248,#26249,#26250,
#26251,#26252,#26253,#26254,#26255,#26256,#26257,#26258,#26259,#26260,#26261,
#26262,#26263,#26264,#26265,#26266,#26267,#26268,#26269,#26270,#26271,#26272,
#26273,#26274,#26275,#26276,#26277,#26278,#26279,#26280,#26281,#26282,#26283,
#26284,#26285,#26286,#26287,#26288,#26289,#26290,#26291,#26292,#26293,#26294,
#26295,#26296,#26297,#26298,#26299,#26300,#26301,#26302,#26303,#26304,#26305,
#26306,#26307,#26308,#26309,#26310,#26311,#26312,#26313,#26314,#26315,#26316,
#26317,#26318,#26319,#26320,#26321,#26322,#26323,#26324,#26325,#26326,#26327,
#26328,#26329,#26330,#26331,#26332,#26333,#26334,#26335,#26336,#26337,#26338,
#26339,#26340,#26341,#26342,#26343,#26344,#26345,#26346,#26347,#26348,#26349,
#26350,#26351,#26352,#26353,#26354,#26355,#26356,#26357,#26358,#26359,#26360,
#26361,#26362,#26363,#26364,#26365,#26366,#26367,#26368,#26369,#26370,#26371,
#26372,#26373,#26374,#26375,#26376,#26377,#26378,#26379,#26380,#26381,#26382,
#26383,#26384,#26385,#26386,#26387,#26388,#26389,#26390,#26391,#26392,#26393,
#26394,#26395,#26396,#26397,#26398,#26399,#26400,#26401,#26402,#26403,#26404,
#26405,#26406,#26407,#26408,#26409,#26410,#26411,#26412,#26413,#26414,#26415,
#26416,#26417));
#26884=CLOSED_SHELL('',(#26418,#26419,#26420,#26421,#26422,#26423,#26424,
#26425,#26426,#26427,#26428,#26429,#26430,#26431,#26432,#26433,#26434,#26435,
#26436,#26437,#26438,#26439,#26440,#26441,#26442,#26443,#26444,#26445,#26446,
#26447,#26448,#26449,#26450,#26451,#26452,#26453,#26454,#26455,#26456,#26457,
#26458,#26459,#26460,#26461,#26462,#26463,#26464,#26465));
#26885=CLOSED_SHELL('',(#26466,#26467,#26468,#26469,#26470,#26471,#26472,
#26473,#26474,#26475,#26476,#26477,#26478,#26479,#26480,#26481,#26482,#26483,
#26484,#26485,#26486,#26487,#26488,#26489,#26490,#26491,#26492,#26493,#26494,
#26495,#26496,#26497,#26498,#26499,#26500,#26501,#26502,#26503,#26504,#26505,
#26506,#26507,#26508,#26509,#26510,#26511,#26512,#26513,#26514,#26515,#26516,
#26517,#26518,#26519,#26520,#26521,#26522,#26523,#26524,#26525,#26526,#26527,
#26528,#26529,#26530,#26531,#26532,#26533,#26534,#26535,#26536,#26537,#26538,
#26539,#26540,#26541,#26542,#26543,#26544,#26545,#26546,#26547,#26548,#26549,
#26550,#26551,#26552,#26553,#26554,#26555,#26556,#26557,#26558,#26559,#26560,
#26561,#26562,#26563,#26564,#26565,#26566,#26567,#26568,#26569,#26570,#26571,
#26572,#26573,#26574,#26575,#26576,#26577,#26578,#26579,#26580,#26581,#26582,
#26583,#26584,#26585,#26586,#26587,#26588,#26589,#26590,#26591,#26592,#26593,
#26594,#26595,#26596,#26597,#26598,#26599,#26600,#26601,#26602,#26603,#26604,
#26605,#26606,#26607,#26608,#26609,#26610,#26611,#26612,#26613,#26614,#26615,
#26616,#26617,#26618,#26619,#26620,#26621,#26622,#26623,#26624,#26625,#26626,
#26627,#26628,#26629,#26630,#26631,#26632,#26633,#26634,#26635,#26636,#26637,
#26638,#26639,#26640,#26641,#26642,#26643,#26644,#26645,#26646,#26647,#26648,
#26649,#26650,#26651,#26652,#26653,#26654,#26655,#26656,#26657,#26658,#26659,
#26660,#26661,#26662,#26663,#26664,#26665,#26666,#26667,#26668,#26669,#26670,
#26671,#26672,#26673,#26674,#26675,#26676,#26677,#26678,#26679,#26680,#26681,
#26682,#26683,#26684,#26685,#26686,#26687,#26688,#26689,#26690,#26691,#26692,
#26693,#26694,#26695,#26696,#26697,#26698,#26699,#26700,#26701,#26702,#26703,
#26704,#26705,#26706,#26707,#26708,#26709,#26710,#26711,#26712,#26713,#26714,
#26715,#26716,#26717,#26718,#26719,#26720,#26721,#26722,#26723,#26724,#26725,
#26726,#26727,#26728,#26729,#26730,#26731,#26732,#26733,#26734,#26735,#26736,
#26737,#26738,#26739,#26740,#26741,#26742,#26743,#26744,#26745,#26746,#26747));
#26886=CLOSED_SHELL('',(#26748,#26749,#26750,#26751,#26752,#26753,#26754,
#26755,#26756,#26757,#26758,#26759,#26760,#26761,#26762,#26763,#26764,#26765,
#26766,#26767,#26768,#26769,#26770,#26771,#26772,#26773,#26774,#26775,#26776,
#26777,#26778,#26779,#26780,#26781,#26782,#26783,#26784,#26785,#26786,#26787,
#26788,#26789,#26790,#26791,#26792,#26793,#26794,#26795,#26796,#26797,#26798,
#26799,#26800,#26801,#26802,#26803,#26804,#26805,#26806,#26807,#26808,#26809,
#26810,#26811,#26812,#26813,#26814,#26815,#26816,#26817,#26818,#26819,#26820,
#26821,#26822,#26823,#26824,#26825,#26826,#26827,#26828,#26829,#26830,#26831,
#26832,#26833,#26834,#26835,#26836,#26837,#26838,#26839,#26840,#26841,#26842,
#26843,#26844,#26845,#26846,#26847,#26848,#26849,#26850,#26851,#26852,#26853,
#26854,#26855,#26856,#26857,#26858,#26859,#26860,#26861,#26862,#26863,#26864,
#26865,#26866,#26867,#26868,#26869,#26870,#26871));
#26887=DERIVED_UNIT_ELEMENT(#26917,1.);
#26888=DERIVED_UNIT_ELEMENT(#70759,-3.);
#26889=DERIVED_UNIT_ELEMENT(#26917,1.);
#26890=DERIVED_UNIT_ELEMENT(#70759,-3.);
#26891=DERIVED_UNIT_ELEMENT(#26917,1.);
#26892=DERIVED_UNIT_ELEMENT(#70759,-3.);
#26893=DERIVED_UNIT_ELEMENT(#26917,1.);
#26894=DERIVED_UNIT_ELEMENT(#70759,-3.);
#26895=DERIVED_UNIT_ELEMENT(#26917,1.);
#26896=DERIVED_UNIT_ELEMENT(#70759,-3.);
#26897=DERIVED_UNIT_ELEMENT(#26917,1.);
#26898=DERIVED_UNIT_ELEMENT(#70759,-3.);
#26899=DERIVED_UNIT_ELEMENT(#26917,1.);
#26900=DERIVED_UNIT_ELEMENT(#70759,-3.);
#26901=DERIVED_UNIT_ELEMENT(#26917,1.);
#26902=DERIVED_UNIT_ELEMENT(#70759,-3.);
#26903=DERIVED_UNIT_ELEMENT(#26917,1.);
#26904=DERIVED_UNIT_ELEMENT(#70759,-3.);
#26905=DERIVED_UNIT_ELEMENT(#26917,1.);
#26906=DERIVED_UNIT_ELEMENT(#70759,-3.);
#26907=DERIVED_UNIT_ELEMENT(#26917,1.);
#26908=DERIVED_UNIT_ELEMENT(#70759,-3.);
#26909=DERIVED_UNIT_ELEMENT(#26917,1.);
#26910=DERIVED_UNIT_ELEMENT(#70759,-3.);
#26911=DERIVED_UNIT_ELEMENT(#26917,1.);
#26912=DERIVED_UNIT_ELEMENT(#70759,-3.);
#26913=DERIVED_UNIT_ELEMENT(#26917,1.);
#26914=DERIVED_UNIT_ELEMENT(#70759,-3.);
#26915=DERIVED_UNIT_ELEMENT(#26917,1.);
#26916=DERIVED_UNIT_ELEMENT(#70759,-3.);
#26917=(
MASS_UNIT()
NAMED_UNIT(*)
SI_UNIT(.KILO.,.GRAM.)
);
#26918=DERIVED_UNIT((#26887,#26888));
#26919=DERIVED_UNIT((#26889,#26890));
#26920=DERIVED_UNIT((#26891,#26892));
#26921=DERIVED_UNIT((#26893,#26894));
#26922=DERIVED_UNIT((#26895,#26896));
#26923=DERIVED_UNIT((#26897,#26898));
#26924=DERIVED_UNIT((#26899,#26900));
#26925=DERIVED_UNIT((#26901,#26902));
#26926=DERIVED_UNIT((#26903,#26904));
#26927=DERIVED_UNIT((#26905,#26906));
#26928=DERIVED_UNIT((#26907,#26908));
#26929=DERIVED_UNIT((#26909,#26910));
#26930=DERIVED_UNIT((#26911,#26912));
#26931=DERIVED_UNIT((#26913,#26914));
#26932=DERIVED_UNIT((#26915,#26916));
#26933=MEASURE_REPRESENTATION_ITEM('density measure',
POSITIVE_RATIO_MEASURE(7850.),#26918);
#26934=MEASURE_REPRESENTATION_ITEM('density measure',
POSITIVE_RATIO_MEASURE(7850.),#26919);
#26935=MEASURE_REPRESENTATION_ITEM('density measure',
POSITIVE_RATIO_MEASURE(7850.),#26920);
#26936=MEASURE_REPRESENTATION_ITEM('density measure',
POSITIVE_RATIO_MEASURE(7850.),#26921);
#26937=MEASURE_REPRESENTATION_ITEM('density measure',
POSITIVE_RATIO_MEASURE(7850.),#26922);
#26938=MEASURE_REPRESENTATION_ITEM('density measure',
POSITIVE_RATIO_MEASURE(7850.),#26923);
#26939=MEASURE_REPRESENTATION_ITEM('density measure',
POSITIVE_RATIO_MEASURE(8470.),#26924);
#26940=MEASURE_REPRESENTATION_ITEM('density measure',
POSITIVE_RATIO_MEASURE(7850.),#26925);
#26941=MEASURE_REPRESENTATION_ITEM('density measure',
POSITIVE_RATIO_MEASURE(7850.),#26926);
#26942=MEASURE_REPRESENTATION_ITEM('density measure',
POSITIVE_RATIO_MEASURE(7850.),#26927);
#26943=MEASURE_REPRESENTATION_ITEM('density measure',
POSITIVE_RATIO_MEASURE(7150.),#26928);
#26944=MEASURE_REPRESENTATION_ITEM('density measure',
POSITIVE_RATIO_MEASURE(7850.),#26929);
#26945=MEASURE_REPRESENTATION_ITEM('density measure',
POSITIVE_RATIO_MEASURE(1060.),#26930);
#26946=MEASURE_REPRESENTATION_ITEM('density measure',
POSITIVE_RATIO_MEASURE(7150.),#26931);
#26947=MEASURE_REPRESENTATION_ITEM('density measure',
POSITIVE_RATIO_MEASURE(7850.),#26932);
#26948=PROPERTY_DEFINITION_REPRESENTATION(#27023,#26978);
#26949=PROPERTY_DEFINITION_REPRESENTATION(#27024,#26979);
#26950=PROPERTY_DEFINITION_REPRESENTATION(#27025,#26980);
#26951=PROPERTY_DEFINITION_REPRESENTATION(#27026,#26981);
#26952=PROPERTY_DEFINITION_REPRESENTATION(#27027,#26982);
#26953=PROPERTY_DEFINITION_REPRESENTATION(#27028,#26983);
#26954=PROPERTY_DEFINITION_REPRESENTATION(#27029,#26984);
#26955=PROPERTY_DEFINITION_REPRESENTATION(#27030,#26985);
#26956=PROPERTY_DEFINITION_REPRESENTATION(#27031,#26986);
#26957=PROPERTY_DEFINITION_REPRESENTATION(#27032,#26987);
#26958=PROPERTY_DEFINITION_REPRESENTATION(#27033,#26988);
#26959=PROPERTY_DEFINITION_REPRESENTATION(#27034,#26989);
#26960=PROPERTY_DEFINITION_REPRESENTATION(#27035,#26990);
#26961=PROPERTY_DEFINITION_REPRESENTATION(#27036,#26991);
#26962=PROPERTY_DEFINITION_REPRESENTATION(#27037,#26992);
#26963=PROPERTY_DEFINITION_REPRESENTATION(#27038,#26993);
#26964=PROPERTY_DEFINITION_REPRESENTATION(#27039,#26994);
#26965=PROPERTY_DEFINITION_REPRESENTATION(#27040,#26995);
#26966=PROPERTY_DEFINITION_REPRESENTATION(#27041,#26996);
#26967=PROPERTY_DEFINITION_REPRESENTATION(#27042,#26997);
#26968=PROPERTY_DEFINITION_REPRESENTATION(#27043,#26998);
#26969=PROPERTY_DEFINITION_REPRESENTATION(#27044,#26999);
#26970=PROPERTY_DEFINITION_REPRESENTATION(#27045,#27000);
#26971=PROPERTY_DEFINITION_REPRESENTATION(#27046,#27001);
#26972=PROPERTY_DEFINITION_REPRESENTATION(#27047,#27002);
#26973=PROPERTY_DEFINITION_REPRESENTATION(#27048,#27003);
#26974=PROPERTY_DEFINITION_REPRESENTATION(#27049,#27004);
#26975=PROPERTY_DEFINITION_REPRESENTATION(#27050,#27005);
#26976=PROPERTY_DEFINITION_REPRESENTATION(#27051,#27006);
#26977=PROPERTY_DEFINITION_REPRESENTATION(#27052,#27007);
#26978=REPRESENTATION('material name',(#27008),#70742);
#26979=REPRESENTATION('density',(#26933),#70742);
#26980=REPRESENTATION('material name',(#27009),#70743);
#26981=REPRESENTATION('density',(#26934),#70743);
#26982=REPRESENTATION('material name',(#27010),#70744);
#26983=REPRESENTATION('density',(#26935),#70744);
#26984=REPRESENTATION('material name',(#27011),#70745);
#26985=REPRESENTATION('density',(#26936),#70745);
#26986=REPRESENTATION('material name',(#27012),#70746);
#26987=REPRESENTATION('density',(#26937),#70746);
#26988=REPRESENTATION('material name',(#27013),#70747);
#26989=REPRESENTATION('density',(#26938),#70747);
#26990=REPRESENTATION('material name',(#27014),#70748);
#26991=REPRESENTATION('density',(#26939),#70748);
#26992=REPRESENTATION('material name',(#27015),#70749);
#26993=REPRESENTATION('density',(#26940),#70749);
#26994=REPRESENTATION('material name',(#27016),#70750);
#26995=REPRESENTATION('density',(#26941),#70750);
#26996=REPRESENTATION('material name',(#27017),#70751);
#26997=REPRESENTATION('density',(#26942),#70751);
#26998=REPRESENTATION('material name',(#27018),#70752);
#26999=REPRESENTATION('density',(#26943),#70752);
#27000=REPRESENTATION('material name',(#27019),#70753);
#27001=REPRESENTATION('density',(#26944),#70753);
#27002=REPRESENTATION('material name',(#27020),#70754);
#27003=REPRESENTATION('density',(#26945),#70754);
#27004=REPRESENTATION('material name',(#27021),#70755);
#27005=REPRESENTATION('density',(#26946),#70755);
#27006=REPRESENTATION('material name',(#27022),#70756);
#27007=REPRESENTATION('density',(#26947),#70756);
#27008=DESCRIPTIVE_REPRESENTATION_ITEM('Steel','Steel');
#27009=DESCRIPTIVE_REPRESENTATION_ITEM('Steel','Steel');
#27010=DESCRIPTIVE_REPRESENTATION_ITEM('Steel','Steel');
#27011=DESCRIPTIVE_REPRESENTATION_ITEM('Steel','Steel');
#27012=DESCRIPTIVE_REPRESENTATION_ITEM('Steel','Steel');
#27013=DESCRIPTIVE_REPRESENTATION_ITEM('Steel','Steel');
#27014=DESCRIPTIVE_REPRESENTATION_ITEM('Bronze','Bronze');
#27015=DESCRIPTIVE_REPRESENTATION_ITEM('Steel','Steel');
#27016=DESCRIPTIVE_REPRESENTATION_ITEM('Steel','Steel');
#27017=DESCRIPTIVE_REPRESENTATION_ITEM('Steel','Steel');
#27018=DESCRIPTIVE_REPRESENTATION_ITEM('Iron, Cast','Iron, Cast');
#27019=DESCRIPTIVE_REPRESENTATION_ITEM('Steel','Steel');
#27020=DESCRIPTIVE_REPRESENTATION_ITEM('ABS Plastic','ABS Plastic');
#27021=DESCRIPTIVE_REPRESENTATION_ITEM('Iron, Cast','Iron, Cast');
#27022=DESCRIPTIVE_REPRESENTATION_ITEM('Steel','Steel');
#27023=PROPERTY_DEFINITION('material property','material name',#70835);
#27024=PROPERTY_DEFINITION('material property','density of part',#70835);
#27025=PROPERTY_DEFINITION('material property','material name',#70836);
#27026=PROPERTY_DEFINITION('material property','density of part',#70836);
#27027=PROPERTY_DEFINITION('material property','material name',#70837);
#27028=PROPERTY_DEFINITION('material property','density of part',#70837);
#27029=PROPERTY_DEFINITION('material property','material name',#70838);
#27030=PROPERTY_DEFINITION('material property','density of part',#70838);
#27031=PROPERTY_DEFINITION('material property','material name',#70839);
#27032=PROPERTY_DEFINITION('material property','density of part',#70839);
#27033=PROPERTY_DEFINITION('material property','material name',#70840);
#27034=PROPERTY_DEFINITION('material property','density of part',#70840);
#27035=PROPERTY_DEFINITION('material property','material name',#70841);
#27036=PROPERTY_DEFINITION('material property','density of part',#70841);
#27037=PROPERTY_DEFINITION('material property','material name',#70842);
#27038=PROPERTY_DEFINITION('material property','density of part',#70842);
#27039=PROPERTY_DEFINITION('material property','material name',#70843);
#27040=PROPERTY_DEFINITION('material property','density of part',#70843);
#27041=PROPERTY_DEFINITION('material property','material name',#70844);
#27042=PROPERTY_DEFINITION('material property','density of part',#70844);
#27043=PROPERTY_DEFINITION('material property','material name',#70845);
#27044=PROPERTY_DEFINITION('material property','density of part',#70845);
#27045=PROPERTY_DEFINITION('material property','material name',#70846);
#27046=PROPERTY_DEFINITION('material property','density of part',#70846);
#27047=PROPERTY_DEFINITION('material property','material name',#70847);
#27048=PROPERTY_DEFINITION('material property','density of part',#70847);
#27049=PROPERTY_DEFINITION('material property','material name',#70848);
#27050=PROPERTY_DEFINITION('material property','density of part',#70848);
#27051=PROPERTY_DEFINITION('material property','material name',#70849);
#27052=PROPERTY_DEFINITION('material property','density of part',#70849);
#27053=AXIS2_PLACEMENT_3D('',#35346,#28985,#28986);
#27054=AXIS2_PLACEMENT_3D('',#35347,#28987,#28988);
#27055=AXIS2_PLACEMENT_3D('',#35348,#28989,#28990);
#27056=AXIS2_PLACEMENT_3D('',#35351,#28991,#28992);
#27057=AXIS2_PLACEMENT_3D('',#35352,#28993,#28994);
#27058=AXIS2_PLACEMENT_3D('',#35355,#28996,#28997);
#27059=AXIS2_PLACEMENT_3D('',#35356,#28998,#28999);
#27060=AXIS2_PLACEMENT_3D('',#35368,#29000,#29001);
#27061=AXIS2_PLACEMENT_3D('',#35419,#29003,#29004);
#27062=AXIS2_PLACEMENT_3D('',#35432,#29006,#29007);
#27063=AXIS2_PLACEMENT_3D('',#35483,#29009,#29010);
#27064=AXIS2_PLACEMENT_3D('',#35496,#29012,#29013);
#27065=AXIS2_PLACEMENT_3D('',#35509,#29015,#29016);
#27066=AXIS2_PLACEMENT_3D('',#35522,#29018,#29019);
#27067=AXIS2_PLACEMENT_3D('',#35535,#29021,#29022);
#27068=AXIS2_PLACEMENT_3D('',#35548,#29024,#29025);
#27069=AXIS2_PLACEMENT_3D('',#35599,#29027,#29028);
#27070=AXIS2_PLACEMENT_3D('',#35612,#29030,#29031);
#27071=AXIS2_PLACEMENT_3D('',#35663,#29033,#29034);
#27072=AXIS2_PLACEMENT_3D('',#35676,#29036,#29037);
#27073=AXIS2_PLACEMENT_3D('',#35727,#29039,#29040);
#27074=AXIS2_PLACEMENT_3D('',#35740,#29042,#29043);
#27075=AXIS2_PLACEMENT_3D('',#35791,#29045,#29046);
#27076=AXIS2_PLACEMENT_3D('',#35804,#29048,#29049);
#27077=AXIS2_PLACEMENT_3D('',#35855,#29051,#29052);
#27078=AXIS2_PLACEMENT_3D('',#35868,#29054,#29055);
#27079=AXIS2_PLACEMENT_3D('',#35879,#29057,#29058);
#27080=AXIS2_PLACEMENT_3D('',#35892,#29060,#29061);
#27081=AXIS2_PLACEMENT_3D('',#35905,#29063,#29064);
#27082=AXIS2_PLACEMENT_3D('',#35918,#29066,#29067);
#27083=AXIS2_PLACEMENT_3D('',#35969,#29069,#29070);
#27084=AXIS2_PLACEMENT_3D('',#35982,#29072,#29073);
#27085=AXIS2_PLACEMENT_3D('',#36033,#29075,#29076);
#27086=AXIS2_PLACEMENT_3D('',#36046,#29078,#29079);
#27087=AXIS2_PLACEMENT_3D('',#36097,#29081,#29082);
#27088=AXIS2_PLACEMENT_3D('',#36110,#29084,#29085);
#27089=AXIS2_PLACEMENT_3D('',#36161,#29087,#29088);
#27090=AXIS2_PLACEMENT_3D('',#36174,#29090,#29091);
#27091=AXIS2_PLACEMENT_3D('',#36225,#29093,#29094);
#27092=AXIS2_PLACEMENT_3D('',#36238,#29096,#29097);
#27093=AXIS2_PLACEMENT_3D('',#36289,#29099,#29100);
#27094=AXIS2_PLACEMENT_3D('',#36302,#29102,#29103);
#27095=AXIS2_PLACEMENT_3D('',#36353,#29105,#29106);
#27096=AXIS2_PLACEMENT_3D('',#36355,#29108,#29109);
#27097=AXIS2_PLACEMENT_3D('',#36357,#29110,#29111);
#27098=AXIS2_PLACEMENT_3D('',#36359,#29113,#29114);
#27099=AXIS2_PLACEMENT_3D('',#36361,#29115,#29116);
#27100=AXIS2_PLACEMENT_3D('',#36365,#29118,#29119);
#27101=AXIS2_PLACEMENT_3D('',#36366,#29120,#29121);
#27102=AXIS2_PLACEMENT_3D('',#36367,#29122,#29123);
#27103=AXIS2_PLACEMENT_3D('',#36419,#29125,#29126);
#27104=AXIS2_PLACEMENT_3D('',#36432,#29128,#29129);
#27105=AXIS2_PLACEMENT_3D('',#36483,#29131,#29132);
#27106=AXIS2_PLACEMENT_3D('',#36496,#29134,#29135);
#27107=AXIS2_PLACEMENT_3D('',#36547,#29137,#29138);
#27108=AXIS2_PLACEMENT_3D('',#36560,#29140,#29141);
#27109=AXIS2_PLACEMENT_3D('',#36611,#29143,#29144);
#27110=AXIS2_PLACEMENT_3D('',#36624,#29146,#29147);
#27111=AXIS2_PLACEMENT_3D('',#36637,#29149,#29150);
#27112=AXIS2_PLACEMENT_3D('',#36650,#29152,#29153);
#27113=AXIS2_PLACEMENT_3D('',#36701,#29155,#29156);
#27114=AXIS2_PLACEMENT_3D('',#36714,#29158,#29159);
#27115=AXIS2_PLACEMENT_3D('',#36765,#29161,#29162);
#27116=AXIS2_PLACEMENT_3D('',#36778,#29164,#29165);
#27117=AXIS2_PLACEMENT_3D('',#36829,#29167,#29168);
#27118=AXIS2_PLACEMENT_3D('',#36842,#29170,#29171);
#27119=AXIS2_PLACEMENT_3D('',#36893,#29173,#29174);
#27120=AXIS2_PLACEMENT_3D('',#36906,#29176,#29177);
#27121=AXIS2_PLACEMENT_3D('',#36957,#29179,#29180);
#27122=AXIS2_PLACEMENT_3D('',#36970,#29182,#29183);
#27123=AXIS2_PLACEMENT_3D('',#36983,#29185,#29186);
#27124=AXIS2_PLACEMENT_3D('',#36996,#29188,#29189);
#27125=AXIS2_PLACEMENT_3D('',#37047,#29191,#29192);
#27126=AXIS2_PLACEMENT_3D('',#37060,#29194,#29195);
#27127=AXIS2_PLACEMENT_3D('',#37111,#29197,#29198);
#27128=AXIS2_PLACEMENT_3D('',#37124,#29200,#29201);
#27129=AXIS2_PLACEMENT_3D('',#37175,#29203,#29204);
#27130=AXIS2_PLACEMENT_3D('',#37188,#29206,#29207);
#27131=AXIS2_PLACEMENT_3D('',#37201,#29209,#29210);
#27132=AXIS2_PLACEMENT_3D('',#37214,#29212,#29213);
#27133=AXIS2_PLACEMENT_3D('',#37265,#29215,#29216);
#27134=AXIS2_PLACEMENT_3D('',#37278,#29218,#29219);
#27135=AXIS2_PLACEMENT_3D('',#37329,#29221,#29222);
#27136=AXIS2_PLACEMENT_3D('',#37342,#29224,#29225);
#27137=AXIS2_PLACEMENT_3D('',#37393,#29227,#29228);
#27138=AXIS2_PLACEMENT_3D('',#37405,#29230,#29231);
#27139=AXIS2_PLACEMENT_3D('',#37406,#29232,#29233);
#27140=AXIS2_PLACEMENT_3D('',#37409,#29235,#29236);
#27141=AXIS2_PLACEMENT_3D('',#37410,#29237,#29238);
#27142=AXIS2_PLACEMENT_3D('',#37412,#29239,#29240);
#27143=AXIS2_PLACEMENT_3D('',#37413,#29241,#29242);
#27144=AXIS2_PLACEMENT_3D('',#37415,#29243,#29244);
#27145=AXIS2_PLACEMENT_3D('',#37417,#29246,#29247);
#27146=AXIS2_PLACEMENT_3D('',#37419,#29248,#29249);
#27147=AXIS2_PLACEMENT_3D('',#37421,#29251,#29252);
#27148=AXIS2_PLACEMENT_3D('',#37423,#29253,#29254);
#27149=AXIS2_PLACEMENT_3D('',#37424,#29255,#29256);
#27150=AXIS2_PLACEMENT_3D('',#37426,#29258,#29259);
#27151=AXIS2_PLACEMENT_3D('',#37428,#29260,#29261);
#27152=AXIS2_PLACEMENT_3D('',#37430,#29263,#29264);
#27153=AXIS2_PLACEMENT_3D('',#37432,#29265,#29266);
#27154=AXIS2_PLACEMENT_3D('',#37433,#29267,#29268);
#27155=AXIS2_PLACEMENT_3D('',#37435,#29269,#29270);
#27156=AXIS2_PLACEMENT_3D('',#37437,#29272,#29273);
#27157=AXIS2_PLACEMENT_3D('',#37439,#29274,#29275);
#27158=AXIS2_PLACEMENT_3D('',#37441,#29277,#29278);
#27159=AXIS2_PLACEMENT_3D('',#37519,#29280,#29281);
#27160=AXIS2_PLACEMENT_3D('',#37522,#29284,#29285);
#27161=AXIS2_PLACEMENT_3D('',#37600,#29287,#29288);
#27162=AXIS2_PLACEMENT_3D('',#37678,#29290,#29291);
#27163=AXIS2_PLACEMENT_3D('',#37681,#29294,#29295);
#27164=AXIS2_PLACEMENT_3D('',#37759,#29297,#29298);
#27165=AXIS2_PLACEMENT_3D('',#37837,#29300,#29301);
#27166=AXIS2_PLACEMENT_3D('',#37840,#29304,#29305);
#27167=AXIS2_PLACEMENT_3D('',#37918,#29307,#29308);
#27168=AXIS2_PLACEMENT_3D('',#37996,#29310,#29311);
#27169=AXIS2_PLACEMENT_3D('',#37999,#29314,#29315);
#27170=AXIS2_PLACEMENT_3D('',#38077,#29317,#29318);
#27171=AXIS2_PLACEMENT_3D('',#38155,#29320,#29321);
#27172=AXIS2_PLACEMENT_3D('',#38158,#29324,#29325);
#27173=AXIS2_PLACEMENT_3D('',#38236,#29327,#29328);
#27174=AXIS2_PLACEMENT_3D('',#38314,#29330,#29331);
#27175=AXIS2_PLACEMENT_3D('',#38317,#29334,#29335);
#27176=AXIS2_PLACEMENT_3D('',#38395,#29337,#29338);
#27177=AXIS2_PLACEMENT_3D('',#38473,#29340,#29341);
#27178=AXIS2_PLACEMENT_3D('',#38476,#29344,#29345);
#27179=AXIS2_PLACEMENT_3D('',#38554,#29347,#29348);
#27180=AXIS2_PLACEMENT_3D('',#38632,#29350,#29351);
#27181=AXIS2_PLACEMENT_3D('',#38635,#29354,#29355);
#27182=AXIS2_PLACEMENT_3D('',#38713,#29357,#29358);
#27183=AXIS2_PLACEMENT_3D('',#38791,#29360,#29361);
#27184=AXIS2_PLACEMENT_3D('',#38794,#29364,#29365);
#27185=AXIS2_PLACEMENT_3D('',#38872,#29367,#29368);
#27186=AXIS2_PLACEMENT_3D('',#38950,#29370,#29371);
#27187=AXIS2_PLACEMENT_3D('',#38953,#29374,#29375);
#27188=AXIS2_PLACEMENT_3D('',#39031,#29377,#29378);
#27189=AXIS2_PLACEMENT_3D('',#39109,#29380,#29381);
#27190=AXIS2_PLACEMENT_3D('',#39112,#29384,#29385);
#27191=AXIS2_PLACEMENT_3D('',#39190,#29387,#29388);
#27192=AXIS2_PLACEMENT_3D('',#39268,#29390,#29391);
#27193=AXIS2_PLACEMENT_3D('',#39271,#29394,#29395);
#27194=AXIS2_PLACEMENT_3D('',#39349,#29397,#29398);
#27195=AXIS2_PLACEMENT_3D('',#39427,#29400,#29401);
#27196=AXIS2_PLACEMENT_3D('',#39430,#29404,#29405);
#27197=AXIS2_PLACEMENT_3D('',#39508,#29407,#29408);
#27198=AXIS2_PLACEMENT_3D('',#39586,#29410,#29411);
#27199=AXIS2_PLACEMENT_3D('',#39589,#29414,#29415);
#27200=AXIS2_PLACEMENT_3D('',#39667,#29417,#29418);
#27201=AXIS2_PLACEMENT_3D('',#39745,#29420,#29421);
#27202=AXIS2_PLACEMENT_3D('',#39748,#29424,#29425);
#27203=AXIS2_PLACEMENT_3D('',#39826,#29427,#29428);
#27204=AXIS2_PLACEMENT_3D('',#39904,#29430,#29431);
#27205=AXIS2_PLACEMENT_3D('',#39907,#29434,#29435);
#27206=AXIS2_PLACEMENT_3D('',#39985,#29437,#29438);
#27207=AXIS2_PLACEMENT_3D('',#40063,#29440,#29441);
#27208=AXIS2_PLACEMENT_3D('',#40066,#29444,#29445);
#27209=AXIS2_PLACEMENT_3D('',#40144,#29447,#29448);
#27210=AXIS2_PLACEMENT_3D('',#40222,#29450,#29451);
#27211=AXIS2_PLACEMENT_3D('',#40225,#29454,#29455);
#27212=AXIS2_PLACEMENT_3D('',#40303,#29457,#29458);
#27213=AXIS2_PLACEMENT_3D('',#40304,#29459,#29460);
#27214=AXIS2_PLACEMENT_3D('',#40305,#29461,#29462);
#27215=AXIS2_PLACEMENT_3D('',#40306,#29463,#29464);
#27216=AXIS2_PLACEMENT_3D('',#40307,#29465,#29466);
#27217=AXIS2_PLACEMENT_3D('',#40308,#29467,#29468);
#27218=AXIS2_PLACEMENT_3D('',#40309,#29469,#29470);
#27219=AXIS2_PLACEMENT_3D('',#40310,#29471,#29472);
#27220=AXIS2_PLACEMENT_3D('',#40311,#29473,#29474);
#27221=AXIS2_PLACEMENT_3D('',#40312,#29475,#29476);
#27222=AXIS2_PLACEMENT_3D('',#40313,#29477,#29478);
#27223=AXIS2_PLACEMENT_3D('',#40314,#29479,#29480);
#27224=AXIS2_PLACEMENT_3D('',#40315,#29481,#29482);
#27225=AXIS2_PLACEMENT_3D('',#40316,#29483,#29484);
#27226=AXIS2_PLACEMENT_3D('',#40317,#29485,#29486);
#27227=AXIS2_PLACEMENT_3D('',#40318,#29487,#29488);
#27228=AXIS2_PLACEMENT_3D('',#40319,#29489,#29490);
#27229=AXIS2_PLACEMENT_3D('',#40320,#29491,#29492);
#27230=AXIS2_PLACEMENT_3D('',#40321,#29493,#29494);
#27231=AXIS2_PLACEMENT_3D('',#40322,#29495,#29496);
#27232=AXIS2_PLACEMENT_3D('',#40323,#29497,#29498);
#27233=AXIS2_PLACEMENT_3D('',#40345,#29500,#29501);
#27234=AXIS2_PLACEMENT_3D('',#40356,#29502,#29503);
#27235=AXIS2_PLACEMENT_3D('',#40440,#29505,#29506);
#27236=AXIS2_PLACEMENT_3D('',#40530,#29508,#29509);
#27237=AXIS2_PLACEMENT_3D('',#40620,#29511,#29512);
#27238=AXIS2_PLACEMENT_3D('',#40704,#29514,#29515);
#27239=AXIS2_PLACEMENT_3D('',#40794,#29517,#29518);
#27240=AXIS2_PLACEMENT_3D('',#40878,#29520,#29521);
#27241=AXIS2_PLACEMENT_3D('',#40968,#29523,#29524);
#27242=AXIS2_PLACEMENT_3D('',#41058,#29526,#29527);
#27243=AXIS2_PLACEMENT_3D('',#41142,#29529,#29530);
#27244=AXIS2_PLACEMENT_3D('',#41232,#29532,#29533);
#27245=AXIS2_PLACEMENT_3D('',#41322,#29535,#29536);
#27246=AXIS2_PLACEMENT_3D('',#41406,#29538,#29539);
#27247=AXIS2_PLACEMENT_3D('',#41415,#29541,#29542);
#27248=AXIS2_PLACEMENT_3D('',#41416,#29543,#29544);
#27249=AXIS2_PLACEMENT_3D('',#41437,#29546,#29547);
#27250=AXIS2_PLACEMENT_3D('',#41452,#29548,#29549);
#27251=AXIS2_PLACEMENT_3D('',#41489,#29551,#29552);
#27252=AXIS2_PLACEMENT_3D('',#41527,#29554,#29555);
#27253=AXIS2_PLACEMENT_3D('',#41564,#29557,#29558);
#27254=AXIS2_PLACEMENT_3D('',#41601,#29560,#29561);
#27255=AXIS2_PLACEMENT_3D('',#41639,#29563,#29564);
#27256=AXIS2_PLACEMENT_3D('',#41676,#29566,#29567);
#27257=AXIS2_PLACEMENT_3D('',#41713,#29569,#29570);
#27258=AXIS2_PLACEMENT_3D('',#41750,#29572,#29573);
#27259=AXIS2_PLACEMENT_3D('',#41787,#29575,#29576);
#27260=AXIS2_PLACEMENT_3D('',#41825,#29578,#29579);
#27261=AXIS2_PLACEMENT_3D('',#41862,#29581,#29582);
#27262=AXIS2_PLACEMENT_3D('',#41944,#29583,#29584);
#27263=AXIS2_PLACEMENT_3D('',#41946,#29585,#29586);
#27264=AXIS2_PLACEMENT_3D('',#42813,#29587,#29588);
#27265=AXIS2_PLACEMENT_3D('',#42815,#29589,#29590);
#27266=AXIS2_PLACEMENT_3D('',#42816,#29591,#29592);
#27267=AXIS2_PLACEMENT_3D('',#42900,#29593,#29594);
#27268=AXIS2_PLACEMENT_3D('',#42901,#29595,#29596);
#27269=AXIS2_PLACEMENT_3D('',#43598,#29597,#29598);
#27270=AXIS2_PLACEMENT_3D('',#43599,#29599,#29600);
#27271=AXIS2_PLACEMENT_3D('',#43600,#29601,#29602);
#27272=AXIS2_PLACEMENT_3D('',#43602,#29603,#29604);
#27273=AXIS2_PLACEMENT_3D('',#43603,#29605,#29606);
#27274=AXIS2_PLACEMENT_3D('',#43605,#29607,#29608);
#27275=AXIS2_PLACEMENT_3D('',#43607,#29610,#29611);
#27276=AXIS2_PLACEMENT_3D('',#43609,#29612,#29613);
#27277=AXIS2_PLACEMENT_3D('',#43611,#29615,#29616);
#27278=AXIS2_PLACEMENT_3D('',#43613,#29617,#29618);
#27279=AXIS2_PLACEMENT_3D('',#43614,#29619,#29620);
#27280=AXIS2_PLACEMENT_3D('',#43616,#29622,#29623);
#27281=AXIS2_PLACEMENT_3D('',#43618,#29624,#29625);
#27282=AXIS2_PLACEMENT_3D('',#43620,#29627,#29628);
#27283=AXIS2_PLACEMENT_3D('',#43621,#29629,#29630);
#27284=AXIS2_PLACEMENT_3D('',#43622,#29631,#29632);
#27285=AXIS2_PLACEMENT_3D('',#43639,#29637,#29638);
#27286=AXIS2_PLACEMENT_3D('',#43641,#29639,#29640);
#27287=AXIS2_PLACEMENT_3D('',#43644,#29642,#29643);
#27288=AXIS2_PLACEMENT_3D('',#43645,#29644,#29645);
#27289=AXIS2_PLACEMENT_3D('',#43651,#29646,#29647);
#27290=AXIS2_PLACEMENT_3D('',#43659,#29648,#29649);
#27291=AXIS2_PLACEMENT_3D('',#43670,#29653,#29654);
#27292=AXIS2_PLACEMENT_3D('',#43687,#29659,#29660);
#27293=AXIS2_PLACEMENT_3D('',#43697,#29664,#29665);
#27294=AXIS2_PLACEMENT_3D('',#43701,#29668,#29669);
#27295=AXIS2_PLACEMENT_3D('',#43714,#29672,#29673);
#27296=AXIS2_PLACEMENT_3D('',#43718,#29675,#29676);
#27297=AXIS2_PLACEMENT_3D('',#43719,#29677,#29678);
#27298=AXIS2_PLACEMENT_3D('',#43720,#29679,#29680);
#27299=AXIS2_PLACEMENT_3D('',#43727,#29683,#29684);
#27300=AXIS2_PLACEMENT_3D('',#43729,#29685,#29686);
#27301=AXIS2_PLACEMENT_3D('',#43733,#29688,#29689);
#27302=AXIS2_PLACEMENT_3D('',#43737,#29691,#29692);
#27303=AXIS2_PLACEMENT_3D('',#43741,#29694,#29695);
#27304=AXIS2_PLACEMENT_3D('',#43745,#29697,#29698);
#27305=AXIS2_PLACEMENT_3D('',#43749,#29700,#29701);
#27306=AXIS2_PLACEMENT_3D('',#43752,#29703,#29704);
#27307=AXIS2_PLACEMENT_3D('',#43754,#29705,#29706);
#27308=AXIS2_PLACEMENT_3D('',#43755,#29707,#29708);
#27309=AXIS2_PLACEMENT_3D('',#43763,#29709,#29710);
#27310=AXIS2_PLACEMENT_3D('',#43780,#29715,#29716);
#27311=AXIS2_PLACEMENT_3D('',#43795,#29720,#29721);
#27312=AXIS2_PLACEMENT_3D('',#43799,#29724,#29725);
#27313=AXIS2_PLACEMENT_3D('',#43804,#29727,#29728);
#27314=AXIS2_PLACEMENT_3D('',#43810,#29732,#29733);
#27315=AXIS2_PLACEMENT_3D('',#43814,#29736,#29737);
#27316=AXIS2_PLACEMENT_3D('',#43815,#29738,#29739);
#27317=AXIS2_PLACEMENT_3D('',#43816,#29740,#29741);
#27318=AXIS2_PLACEMENT_3D('',#43818,#29742,#29743);
#27319=AXIS2_PLACEMENT_3D('',#43826,#29744,#29745);
#27320=AXIS2_PLACEMENT_3D('',#43829,#29747,#29748);
#27321=AXIS2_PLACEMENT_3D('',#43830,#29749,#29750);
#27322=AXIS2_PLACEMENT_3D('',#43832,#29752,#29753);
#27323=AXIS2_PLACEMENT_3D('',#43835,#29755,#29756);
#27324=AXIS2_PLACEMENT_3D('',#43836,#29757,#29758);
#27325=AXIS2_PLACEMENT_3D('',#43838,#29759,#29760);
#27326=AXIS2_PLACEMENT_3D('',#43840,#29762,#29763);
#27327=AXIS2_PLACEMENT_3D('',#43857,#29768,#29769);
#27328=AXIS2_PLACEMENT_3D('',#43872,#29773,#29774);
#27329=AXIS2_PLACEMENT_3D('',#43876,#29777,#29778);
#27330=AXIS2_PLACEMENT_3D('',#43881,#29780,#29781);
#27331=AXIS2_PLACEMENT_3D('',#43898,#29786,#29787);
#27332=AXIS2_PLACEMENT_3D('',#43900,#29788,#29789);
#27333=AXIS2_PLACEMENT_3D('',#43903,#29791,#29792);
#27334=AXIS2_PLACEMENT_3D('',#43904,#29793,#29794);
#27335=AXIS2_PLACEMENT_3D('',#43915,#29795,#29796);
#27336=AXIS2_PLACEMENT_3D('',#43919,#29799,#29800);
#27337=AXIS2_PLACEMENT_3D('',#43920,#29801,#29802);
#27338=AXIS2_PLACEMENT_3D('',#43921,#29803,#29804);
#27339=AXIS2_PLACEMENT_3D('',#43924,#29806,#29807);
#27340=AXIS2_PLACEMENT_3D('',#43925,#29808,#29809);
#27341=AXIS2_PLACEMENT_3D('',#43927,#29811,#29812);
#27342=AXIS2_PLACEMENT_3D('',#43937,#29816,#29817);
#27343=AXIS2_PLACEMENT_3D('',#43952,#29821,#29822);
#27344=AXIS2_PLACEMENT_3D('',#43956,#29825,#29826);
#27345=AXIS2_PLACEMENT_3D('',#43958,#29828,#29829);
#27346=AXIS2_PLACEMENT_3D('',#43970,#29834,#29835);
#27347=AXIS2_PLACEMENT_3D('',#43971,#29836,#29837);
#27348=AXIS2_PLACEMENT_3D('',#43972,#29838,#29839);
#27349=AXIS2_PLACEMENT_3D('',#43976,#29842,#29843);
#27350=AXIS2_PLACEMENT_3D('',#43977,#29844,#29845);
#27351=AXIS2_PLACEMENT_3D('',#43978,#29846,#29847);
#27352=AXIS2_PLACEMENT_3D('',#43981,#29849,#29850);
#27353=AXIS2_PLACEMENT_3D('',#43982,#29851,#29852);
#27354=AXIS2_PLACEMENT_3D('',#43984,#29854,#29855);
#27355=AXIS2_PLACEMENT_3D('',#43985,#29856,#29857);
#27356=AXIS2_PLACEMENT_3D('',#43986,#29858,#29859);
#27357=AXIS2_PLACEMENT_3D('',#43987,#29860,#29861);
#27358=AXIS2_PLACEMENT_3D('',#43989,#29862,#29863);
#27359=AXIS2_PLACEMENT_3D('',#43991,#29864,#29865);
#27360=AXIS2_PLACEMENT_3D('',#43996,#29866,#29867);
#27361=AXIS2_PLACEMENT_3D('',#43998,#29868,#29869);
#27362=AXIS2_PLACEMENT_3D('',#44003,#29870,#29871);
#27363=AXIS2_PLACEMENT_3D('',#44005,#29872,#29873);
#27364=AXIS2_PLACEMENT_3D('',#44007,#29874,#29875);
#27365=AXIS2_PLACEMENT_3D('',#44012,#29876,#29877);
#27366=AXIS2_PLACEMENT_3D('',#44015,#29879,#29880);
#27367=AXIS2_PLACEMENT_3D('',#44016,#29881,#29882);
#27368=AXIS2_PLACEMENT_3D('',#44018,#29884,#29885);
#27369=AXIS2_PLACEMENT_3D('',#44021,#29887,#29888);
#27370=AXIS2_PLACEMENT_3D('',#44022,#29889,#29890);
#27371=AXIS2_PLACEMENT_3D('',#44027,#29892,#29893);
#27372=AXIS2_PLACEMENT_3D('',#44028,#29894,#29895);
#27373=AXIS2_PLACEMENT_3D('',#44029,#29896,#29897);
#27374=AXIS2_PLACEMENT_3D('',#44030,#29898,#29899);
#27375=AXIS2_PLACEMENT_3D('',#44033,#29901,#29902);
#27376=AXIS2_PLACEMENT_3D('',#44034,#29903,#29904);
#27377=AXIS2_PLACEMENT_3D('',#44039,#29906,#29907);
#27378=AXIS2_PLACEMENT_3D('',#44040,#29908,#29909);
#27379=AXIS2_PLACEMENT_3D('',#44041,#29910,#29911);
#27380=AXIS2_PLACEMENT_3D('',#44043,#29912,#29913);
#27381=AXIS2_PLACEMENT_3D('',#44044,#29914,#29915);
#27382=AXIS2_PLACEMENT_3D('',#44046,#29917,#29918);
#27383=AXIS2_PLACEMENT_3D('',#44048,#29920,#29921);
#27384=AXIS2_PLACEMENT_3D('',#44049,#29922,#29923);
#27385=AXIS2_PLACEMENT_3D('',#44050,#29924,#29925);
#27386=AXIS2_PLACEMENT_3D('',#44051,#29926,#29927);
#27387=AXIS2_PLACEMENT_3D('',#44052,#29928,#29929);
#27388=AXIS2_PLACEMENT_3D('',#44053,#29930,#29931);
#27389=AXIS2_PLACEMENT_3D('',#44054,#29932,#29933);
#27390=AXIS2_PLACEMENT_3D('',#44055,#29934,#29935);
#27391=AXIS2_PLACEMENT_3D('',#44057,#29936,#29937);
#27392=AXIS2_PLACEMENT_3D('',#44058,#29938,#29939);
#27393=AXIS2_PLACEMENT_3D('',#44060,#29940,#29941);
#27394=AXIS2_PLACEMENT_3D('',#44062,#29943,#29944);
#27395=AXIS2_PLACEMENT_3D('',#44064,#29945,#29946);
#27396=AXIS2_PLACEMENT_3D('',#44066,#29948,#29949);
#27397=AXIS2_PLACEMENT_3D('',#44068,#29950,#29951);
#27398=AXIS2_PLACEMENT_3D('',#44070,#29953,#29954);
#27399=AXIS2_PLACEMENT_3D('',#44071,#29955,#29956);
#27400=AXIS2_PLACEMENT_3D('',#44465,#29958,#29959);
#27401=AXIS2_PLACEMENT_3D('',#44496,#29961,#29962);
#27402=AXIS2_PLACEMENT_3D('',#44498,#29963,#29964);
#27403=AXIS2_PLACEMENT_3D('',#44530,#29967,#29968);
#27404=AXIS2_PLACEMENT_3D('',#44942,#29970,#29971);
#27405=AXIS2_PLACEMENT_3D('',#44944,#29972,#29973);
#27406=AXIS2_PLACEMENT_3D('',#44947,#29975,#29976);
#27407=AXIS2_PLACEMENT_3D('',#44948,#29977,#29978);
#27408=AXIS2_PLACEMENT_3D('',#44950,#29979,#29980);
#27409=AXIS2_PLACEMENT_3D('',#44952,#29981,#29982);
#27410=AXIS2_PLACEMENT_3D('',#44981,#29983,#29984);
#27411=AXIS2_PLACEMENT_3D('',#45008,#29985,#29986);
#27412=AXIS2_PLACEMENT_3D('',#45037,#29987,#29988);
#27413=AXIS2_PLACEMENT_3D('',#45066,#29989,#29990);
#27414=AXIS2_PLACEMENT_3D('',#45093,#29991,#29992);
#27415=AXIS2_PLACEMENT_3D('',#45121,#29993,#29994);
#27416=AXIS2_PLACEMENT_3D('',#45312,#29995,#29996);
#27417=AXIS2_PLACEMENT_3D('',#45314,#29998,#29999);
#27418=AXIS2_PLACEMENT_3D('',#45316,#30001,#30002);
#27419=AXIS2_PLACEMENT_3D('',#45318,#30004,#30005);
#27420=AXIS2_PLACEMENT_3D('',#45320,#30007,#30008);
#27421=AXIS2_PLACEMENT_3D('',#45322,#30010,#30011);
#27422=AXIS2_PLACEMENT_3D('',#45324,#30013,#30014);
#27423=AXIS2_PLACEMENT_3D('',#45327,#30016,#30017);
#27424=AXIS2_PLACEMENT_3D('',#45328,#30018,#30019);
#27425=AXIS2_PLACEMENT_3D('',#45330,#30020,#30021);
#27426=AXIS2_PLACEMENT_3D('',#45331,#30022,#30023);
#27427=AXIS2_PLACEMENT_3D('',#45333,#30025,#30026);
#27428=AXIS2_PLACEMENT_3D('',#45335,#30027,#30028);
#27429=AXIS2_PLACEMENT_3D('',#45337,#30030,#30031);
#27430=AXIS2_PLACEMENT_3D('',#45339,#30032,#30033);
#27431=AXIS2_PLACEMENT_3D('',#45340,#30034,#30035);
#27432=AXIS2_PLACEMENT_3D('',#45342,#30037,#30038);
#27433=AXIS2_PLACEMENT_3D('',#45343,#30039,#30040);
#27434=AXIS2_PLACEMENT_3D('',#45365,#30042,#30043);
#27435=AXIS2_PLACEMENT_3D('',#45376,#30044,#30045);
#27436=AXIS2_PLACEMENT_3D('',#45460,#30047,#30048);
#27437=AXIS2_PLACEMENT_3D('',#45550,#30050,#30051);
#27438=AXIS2_PLACEMENT_3D('',#45640,#30053,#30054);
#27439=AXIS2_PLACEMENT_3D('',#45730,#30056,#30057);
#27440=AXIS2_PLACEMENT_3D('',#45814,#30059,#30060);
#27441=AXIS2_PLACEMENT_3D('',#45904,#30062,#30063);
#27442=AXIS2_PLACEMENT_3D('',#45914,#30065,#30066);
#27443=AXIS2_PLACEMENT_3D('',#45915,#30067,#30068);
#27444=AXIS2_PLACEMENT_3D('',#45937,#30070,#30071);
#27445=AXIS2_PLACEMENT_3D('',#45953,#30072,#30073);
#27446=AXIS2_PLACEMENT_3D('',#45990,#30075,#30076);
#27447=AXIS2_PLACEMENT_3D('',#46027,#30078,#30079);
#27448=AXIS2_PLACEMENT_3D('',#46065,#30081,#30082);
#27449=AXIS2_PLACEMENT_3D('',#46103,#30084,#30085);
#27450=AXIS2_PLACEMENT_3D('',#46140,#30087,#30088);
#27451=AXIS2_PLACEMENT_3D('',#46219,#30089,#30090);
#27452=AXIS2_PLACEMENT_3D('',#46221,#30091,#30092);
#27453=AXIS2_PLACEMENT_3D('',#46789,#30093,#30094);
#27454=AXIS2_PLACEMENT_3D('',#46791,#30095,#30096);
#27455=AXIS2_PLACEMENT_3D('',#46792,#30097,#30098);
#27456=AXIS2_PLACEMENT_3D('',#46873,#30099,#30100);
#27457=AXIS2_PLACEMENT_3D('',#46874,#30101,#30102);
#27458=AXIS2_PLACEMENT_3D('',#47278,#30103,#30104);
#27459=AXIS2_PLACEMENT_3D('',#47282,#30106,#30107);
#27460=AXIS2_PLACEMENT_3D('',#47283,#30108,#30109);
#27461=AXIS2_PLACEMENT_3D('',#47286,#30111,#30112);
#27462=AXIS2_PLACEMENT_3D('',#47287,#30113,#30114);
#27463=AXIS2_PLACEMENT_3D('',#47290,#30116,#30117);
#27464=AXIS2_PLACEMENT_3D('',#47291,#30118,#30119);
#27465=AXIS2_PLACEMENT_3D('',#47294,#30121,#30122);
#27466=AXIS2_PLACEMENT_3D('',#47295,#30123,#30124);
#27467=AXIS2_PLACEMENT_3D('',#47298,#30126,#30127);
#27468=AXIS2_PLACEMENT_3D('',#47299,#30128,#30129);
#27469=AXIS2_PLACEMENT_3D('',#47301,#30131,#30132);
#27470=AXIS2_PLACEMENT_3D('',#47302,#30133,#30134);
#27471=AXIS2_PLACEMENT_3D('',#47307,#30136,#30137);
#27472=AXIS2_PLACEMENT_3D('',#47316,#30138,#30139);
#27473=AXIS2_PLACEMENT_3D('',#47325,#30140,#30141);
#27474=AXIS2_PLACEMENT_3D('',#47334,#30142,#30143);
#27475=AXIS2_PLACEMENT_3D('',#47343,#30144,#30145);
#27476=AXIS2_PLACEMENT_3D('',#47352,#30146,#30147);
#27477=AXIS2_PLACEMENT_3D('',#47360,#30148,#30149);
#27478=AXIS2_PLACEMENT_3D('',#47361,#30150,#30151);
#27479=AXIS2_PLACEMENT_3D('',#47367,#30155,#30156);
#27480=AXIS2_PLACEMENT_3D('',#47371,#30159,#30160);
#27481=AXIS2_PLACEMENT_3D('',#47375,#30163,#30164);
#27482=AXIS2_PLACEMENT_3D('',#47379,#30167,#30168);
#27483=AXIS2_PLACEMENT_3D('',#47383,#30171,#30172);
#27484=AXIS2_PLACEMENT_3D('',#47387,#30175,#30176);
#27485=AXIS2_PLACEMENT_3D('',#47391,#30179,#30180);
#27486=AXIS2_PLACEMENT_3D('',#47395,#30183,#30184);
#27487=AXIS2_PLACEMENT_3D('',#47399,#30187,#30188);
#27488=AXIS2_PLACEMENT_3D('',#47401,#30190,#30191);
#27489=AXIS2_PLACEMENT_3D('',#47403,#30193,#30194);
#27490=AXIS2_PLACEMENT_3D('',#47404,#30195,#30196);
#27491=AXIS2_PLACEMENT_3D('',#47406,#30198,#30199);
#27492=AXIS2_PLACEMENT_3D('',#47410,#30202,#30203);
#27493=AXIS2_PLACEMENT_3D('',#47412,#30205,#30206);
#27494=AXIS2_PLACEMENT_3D('',#47414,#30208,#30209);
#27495=AXIS2_PLACEMENT_3D('',#47418,#30212,#30213);
#27496=AXIS2_PLACEMENT_3D('',#47420,#30215,#30216);
#27497=AXIS2_PLACEMENT_3D('',#47421,#30217,#30218);
#27498=AXIS2_PLACEMENT_3D('',#47422,#30219,#30220);
#27499=AXIS2_PLACEMENT_3D('',#47424,#30222,#30223);
#27500=AXIS2_PLACEMENT_3D('',#47425,#30224,#30225);
#27501=AXIS2_PLACEMENT_3D('',#47426,#30226,#30227);
#27502=AXIS2_PLACEMENT_3D('',#47427,#30228,#30229);
#27503=AXIS2_PLACEMENT_3D('',#47429,#30230,#30231);
#27504=AXIS2_PLACEMENT_3D('',#47430,#30232,#30233);
#27505=AXIS2_PLACEMENT_3D('',#47432,#30235,#30236);
#27506=AXIS2_PLACEMENT_3D('',#47433,#30237,#30238);
#27507=AXIS2_PLACEMENT_3D('',#47434,#30239,#30240);
#27508=AXIS2_PLACEMENT_3D('',#47436,#30241,#30242);
#27509=AXIS2_PLACEMENT_3D('',#47438,#30244,#30245);
#27510=AXIS2_PLACEMENT_3D('',#47439,#30246,#30247);
#27511=AXIS2_PLACEMENT_3D('',#47440,#30248,#30249);
#27512=AXIS2_PLACEMENT_3D('',#47449,#30254,#30255);
#27513=AXIS2_PLACEMENT_3D('',#47455,#30259,#30260);
#27514=AXIS2_PLACEMENT_3D('',#47461,#30264,#30265);
#27515=AXIS2_PLACEMENT_3D('',#47464,#30268,#30269);
#27516=AXIS2_PLACEMENT_3D('',#47465,#30270,#30271);
#27517=AXIS2_PLACEMENT_3D('',#47474,#30276,#30277);
#27518=AXIS2_PLACEMENT_3D('',#47480,#30281,#30282);
#27519=AXIS2_PLACEMENT_3D('',#47486,#30286,#30287);
#27520=AXIS2_PLACEMENT_3D('',#47489,#30290,#30291);
#27521=AXIS2_PLACEMENT_3D('',#47490,#30292,#30293);
#27522=AXIS2_PLACEMENT_3D('',#47497,#30297,#30298);
#27523=AXIS2_PLACEMENT_3D('',#47504,#30302,#30303);
#27524=AXIS2_PLACEMENT_3D('',#47511,#30307,#30308);
#27525=AXIS2_PLACEMENT_3D('',#47518,#30312,#30313);
#27526=AXIS2_PLACEMENT_3D('',#47525,#30317,#30318);
#27527=AXIS2_PLACEMENT_3D('',#47528,#30321,#30322);
#27528=AXIS2_PLACEMENT_3D('',#47535,#30326,#30327);
#27529=AXIS2_PLACEMENT_3D('',#47542,#30331,#30332);
#27530=AXIS2_PLACEMENT_3D('',#47545,#30335,#30336);
#27531=AXIS2_PLACEMENT_3D('',#47548,#30339,#30340);
#27532=AXIS2_PLACEMENT_3D('',#47555,#30344,#30345);
#27533=AXIS2_PLACEMENT_3D('',#47558,#30348,#30349);
#27534=AXIS2_PLACEMENT_3D('',#47561,#30352,#30353);
#27535=AXIS2_PLACEMENT_3D('',#47564,#30356,#30357);
#27536=AXIS2_PLACEMENT_3D('',#47567,#30360,#30361);
#27537=AXIS2_PLACEMENT_3D('',#47570,#30364,#30365);
#27538=AXIS2_PLACEMENT_3D('',#47573,#30368,#30369);
#27539=AXIS2_PLACEMENT_3D('',#47576,#30372,#30373);
#27540=AXIS2_PLACEMENT_3D('',#47579,#30376,#30377);
#27541=AXIS2_PLACEMENT_3D('',#47582,#30380,#30381);
#27542=AXIS2_PLACEMENT_3D('',#47583,#30382,#30383);
#27543=AXIS2_PLACEMENT_3D('',#47584,#30384,#30385);
#27544=AXIS2_PLACEMENT_3D('',#47585,#30386,#30387);
#27545=AXIS2_PLACEMENT_3D('',#47586,#30388,#30389);
#27546=AXIS2_PLACEMENT_3D('',#47587,#30390,#30391);
#27547=AXIS2_PLACEMENT_3D('',#47588,#30392,#30393);
#27548=AXIS2_PLACEMENT_3D('',#47589,#30394,#30395);
#27549=AXIS2_PLACEMENT_3D('',#47611,#30397,#30398);
#27550=AXIS2_PLACEMENT_3D('',#47622,#30399,#30400);
#27551=AXIS2_PLACEMENT_3D('',#47706,#30402,#30403);
#27552=AXIS2_PLACEMENT_3D('',#47796,#30405,#30406);
#27553=AXIS2_PLACEMENT_3D('',#47886,#30408,#30409);
#27554=AXIS2_PLACEMENT_3D('',#47970,#30411,#30412);
#27555=AXIS2_PLACEMENT_3D('',#48060,#30414,#30415);
#27556=AXIS2_PLACEMENT_3D('',#48144,#30417,#30418);
#27557=AXIS2_PLACEMENT_3D('',#48234,#30420,#30421);
#27558=AXIS2_PLACEMENT_3D('',#48324,#30423,#30424);
#27559=AXIS2_PLACEMENT_3D('',#48408,#30426,#30427);
#27560=AXIS2_PLACEMENT_3D('',#48498,#30429,#30430);
#27561=AXIS2_PLACEMENT_3D('',#48582,#30432,#30433);
#27562=AXIS2_PLACEMENT_3D('',#48672,#30435,#30436);
#27563=AXIS2_PLACEMENT_3D('',#48762,#30438,#30439);
#27564=AXIS2_PLACEMENT_3D('',#48846,#30441,#30442);
#27565=AXIS2_PLACEMENT_3D('',#48936,#30444,#30445);
#27566=AXIS2_PLACEMENT_3D('',#49026,#30447,#30448);
#27567=AXIS2_PLACEMENT_3D('',#49110,#30450,#30451);
#27568=AXIS2_PLACEMENT_3D('',#49200,#30453,#30454);
#27569=AXIS2_PLACEMENT_3D('',#49284,#30456,#30457);
#27570=AXIS2_PLACEMENT_3D('',#49374,#30459,#30460);
#27571=AXIS2_PLACEMENT_3D('',#49464,#30462,#30463);
#27572=AXIS2_PLACEMENT_3D('',#49548,#30465,#30466);
#27573=AXIS2_PLACEMENT_3D('',#49638,#30468,#30469);
#27574=AXIS2_PLACEMENT_3D('',#49722,#30471,#30472);
#27575=AXIS2_PLACEMENT_3D('',#49812,#30474,#30475);
#27576=AXIS2_PLACEMENT_3D('',#49902,#30477,#30478);
#27577=AXIS2_PLACEMENT_3D('',#49986,#30480,#30481);
#27578=AXIS2_PLACEMENT_3D('',#50076,#30483,#30484);
#27579=AXIS2_PLACEMENT_3D('',#50085,#30486,#30487);
#27580=AXIS2_PLACEMENT_3D('',#50086,#30488,#30489);
#27581=AXIS2_PLACEMENT_3D('',#50108,#30491,#30492);
#27582=AXIS2_PLACEMENT_3D('',#50123,#30493,#30494);
#27583=AXIS2_PLACEMENT_3D('',#50160,#30496,#30497);
#27584=AXIS2_PLACEMENT_3D('',#50197,#30499,#30500);
#27585=AXIS2_PLACEMENT_3D('',#50235,#30502,#30503);
#27586=AXIS2_PLACEMENT_3D('',#50272,#30505,#30506);
#27587=AXIS2_PLACEMENT_3D('',#50309,#30508,#30509);
#27588=AXIS2_PLACEMENT_3D('',#50346,#30511,#30512);
#27589=AXIS2_PLACEMENT_3D('',#50383,#30514,#30515);
#27590=AXIS2_PLACEMENT_3D('',#50421,#30517,#30518);
#27591=AXIS2_PLACEMENT_3D('',#50458,#30520,#30521);
#27592=AXIS2_PLACEMENT_3D('',#50495,#30523,#30524);
#27593=AXIS2_PLACEMENT_3D('',#50532,#30526,#30527);
#27594=AXIS2_PLACEMENT_3D('',#50569,#30529,#30530);
#27595=AXIS2_PLACEMENT_3D('',#50607,#30532,#30533);
#27596=AXIS2_PLACEMENT_3D('',#50644,#30535,#30536);
#27597=AXIS2_PLACEMENT_3D('',#50681,#30538,#30539);
#27598=AXIS2_PLACEMENT_3D('',#50719,#30541,#30542);
#27599=AXIS2_PLACEMENT_3D('',#50756,#30544,#30545);
#27600=AXIS2_PLACEMENT_3D('',#50793,#30547,#30548);
#27601=AXIS2_PLACEMENT_3D('',#50830,#30550,#30551);
#27602=AXIS2_PLACEMENT_3D('',#50867,#30553,#30554);
#27603=AXIS2_PLACEMENT_3D('',#50905,#30556,#30557);
#27604=AXIS2_PLACEMENT_3D('',#50942,#30559,#30560);
#27605=AXIS2_PLACEMENT_3D('',#50979,#30562,#30563);
#27606=AXIS2_PLACEMENT_3D('',#51016,#30565,#30566);
#27607=AXIS2_PLACEMENT_3D('',#51053,#30568,#30569);
#27608=AXIS2_PLACEMENT_3D('',#51091,#30571,#30572);
#27609=AXIS2_PLACEMENT_3D('',#51128,#30574,#30575);
#27610=AXIS2_PLACEMENT_3D('',#51204,#30576,#30577);
#27611=AXIS2_PLACEMENT_3D('',#51206,#30578,#30579);
#27612=AXIS2_PLACEMENT_3D('',#52869,#30580,#30581);
#27613=AXIS2_PLACEMENT_3D('',#52871,#30582,#30583);
#27614=AXIS2_PLACEMENT_3D('',#52872,#30584,#30585);
#27615=AXIS2_PLACEMENT_3D('',#52950,#30586,#30587);
#27616=AXIS2_PLACEMENT_3D('',#52951,#30588,#30589);
#27617=AXIS2_PLACEMENT_3D('',#54456,#30590,#30591);
#27618=AXIS2_PLACEMENT_3D('',#54460,#30593,#30594);
#27619=AXIS2_PLACEMENT_3D('',#54461,#30595,#30596);
#27620=AXIS2_PLACEMENT_3D('',#54464,#30598,#30599);
#27621=AXIS2_PLACEMENT_3D('',#54465,#30600,#30601);
#27622=AXIS2_PLACEMENT_3D('',#54468,#30603,#30604);
#27623=AXIS2_PLACEMENT_3D('',#54469,#30605,#30606);
#27624=AXIS2_PLACEMENT_3D('',#54472,#30608,#30609);
#27625=AXIS2_PLACEMENT_3D('',#54473,#30610,#30611);
#27626=AXIS2_PLACEMENT_3D('',#54476,#30613,#30614);
#27627=AXIS2_PLACEMENT_3D('',#54477,#30615,#30616);
#27628=AXIS2_PLACEMENT_3D('',#54479,#30618,#30619);
#27629=AXIS2_PLACEMENT_3D('',#54480,#30620,#30621);
#27630=AXIS2_PLACEMENT_3D('',#54485,#30623,#30624);
#27631=AXIS2_PLACEMENT_3D('',#54494,#30625,#30626);
#27632=AXIS2_PLACEMENT_3D('',#54503,#30627,#30628);
#27633=AXIS2_PLACEMENT_3D('',#54512,#30629,#30630);
#27634=AXIS2_PLACEMENT_3D('',#54521,#30631,#30632);
#27635=AXIS2_PLACEMENT_3D('',#54530,#30633,#30634);
#27636=AXIS2_PLACEMENT_3D('',#54538,#30635,#30636);
#27637=AXIS2_PLACEMENT_3D('',#54539,#30637,#30638);
#27638=AXIS2_PLACEMENT_3D('',#54545,#30642,#30643);
#27639=AXIS2_PLACEMENT_3D('',#54549,#30646,#30647);
#27640=AXIS2_PLACEMENT_3D('',#54553,#30650,#30651);
#27641=AXIS2_PLACEMENT_3D('',#54557,#30654,#30655);
#27642=AXIS2_PLACEMENT_3D('',#54561,#30658,#30659);
#27643=AXIS2_PLACEMENT_3D('',#54565,#30662,#30663);
#27644=AXIS2_PLACEMENT_3D('',#54569,#30666,#30667);
#27645=AXIS2_PLACEMENT_3D('',#54573,#30670,#30671);
#27646=AXIS2_PLACEMENT_3D('',#54577,#30674,#30675);
#27647=AXIS2_PLACEMENT_3D('',#54579,#30677,#30678);
#27648=AXIS2_PLACEMENT_3D('',#54581,#30680,#30681);
#27649=AXIS2_PLACEMENT_3D('',#54582,#30682,#30683);
#27650=AXIS2_PLACEMENT_3D('',#54584,#30685,#30686);
#27651=AXIS2_PLACEMENT_3D('',#54588,#30689,#30690);
#27652=AXIS2_PLACEMENT_3D('',#54590,#30692,#30693);
#27653=AXIS2_PLACEMENT_3D('',#54592,#30695,#30696);
#27654=AXIS2_PLACEMENT_3D('',#54596,#30699,#30700);
#27655=AXIS2_PLACEMENT_3D('',#54598,#30702,#30703);
#27656=AXIS2_PLACEMENT_3D('',#54599,#30704,#30705);
#27657=AXIS2_PLACEMENT_3D('',#54600,#30706,#30707);
#27658=AXIS2_PLACEMENT_3D('',#54602,#30709,#30710);
#27659=AXIS2_PLACEMENT_3D('',#54603,#30711,#30712);
#27660=AXIS2_PLACEMENT_3D('',#54604,#30713,#30714);
#27661=AXIS2_PLACEMENT_3D('',#54605,#30715,#30716);
#27662=AXIS2_PLACEMENT_3D('',#54607,#30717,#30718);
#27663=AXIS2_PLACEMENT_3D('',#54608,#30719,#30720);
#27664=AXIS2_PLACEMENT_3D('',#54610,#30722,#30723);
#27665=AXIS2_PLACEMENT_3D('',#54611,#30724,#30725);
#27666=AXIS2_PLACEMENT_3D('',#54612,#30726,#30727);
#27667=AXIS2_PLACEMENT_3D('',#54614,#30728,#30729);
#27668=AXIS2_PLACEMENT_3D('',#54616,#30731,#30732);
#27669=AXIS2_PLACEMENT_3D('',#54617,#30733,#30734);
#27670=AXIS2_PLACEMENT_3D('',#54618,#30735,#30736);
#27671=AXIS2_PLACEMENT_3D('',#54620,#30737,#30738);
#27672=AXIS2_PLACEMENT_3D('',#54623,#30740,#30741);
#27673=AXIS2_PLACEMENT_3D('',#54624,#30742,#30743);
#27674=AXIS2_PLACEMENT_3D('',#54626,#30744,#30745);
#27675=AXIS2_PLACEMENT_3D('',#54628,#30747,#30748);
#27676=AXIS2_PLACEMENT_3D('',#54630,#30749,#30750);
#27677=AXIS2_PLACEMENT_3D('',#54631,#30751,#30752);
#27678=AXIS2_PLACEMENT_3D('',#54633,#30753,#30754);
#27679=AXIS2_PLACEMENT_3D('',#54635,#30756,#30757);
#27680=AXIS2_PLACEMENT_3D('',#54637,#30758,#30759);
#27681=AXIS2_PLACEMENT_3D('',#54638,#30760,#30761);
#27682=AXIS2_PLACEMENT_3D('',#54668,#30763,#30764);
#27683=AXIS2_PLACEMENT_3D('',#54676,#30767,#30768);
#27684=AXIS2_PLACEMENT_3D('',#54682,#30770,#30771);
#27685=AXIS2_PLACEMENT_3D('',#54688,#30773,#30774);
#27686=AXIS2_PLACEMENT_3D('',#54705,#30776,#30777);
#27687=AXIS2_PLACEMENT_3D('',#54707,#30779,#30780);
#27688=AXIS2_PLACEMENT_3D('',#54709,#30782,#30783);
#27689=AXIS2_PLACEMENT_3D('',#54710,#30784,#30785);
#27690=AXIS2_PLACEMENT_3D('',#54711,#30786,#30787);
#27691=AXIS2_PLACEMENT_3D('',#54733,#30789,#30790);
#27692=AXIS2_PLACEMENT_3D('',#54744,#30791,#30792);
#27693=AXIS2_PLACEMENT_3D('',#54828,#30794,#30795);
#27694=AXIS2_PLACEMENT_3D('',#54918,#30797,#30798);
#27695=AXIS2_PLACEMENT_3D('',#55008,#30800,#30801);
#27696=AXIS2_PLACEMENT_3D('',#55092,#30803,#30804);
#27697=AXIS2_PLACEMENT_3D('',#55182,#30806,#30807);
#27698=AXIS2_PLACEMENT_3D('',#55266,#30809,#30810);
#27699=AXIS2_PLACEMENT_3D('',#55356,#30812,#30813);
#27700=AXIS2_PLACEMENT_3D('',#55446,#30815,#30816);
#27701=AXIS2_PLACEMENT_3D('',#55530,#30818,#30819);
#27702=AXIS2_PLACEMENT_3D('',#55620,#30821,#30822);
#27703=AXIS2_PLACEMENT_3D('',#55710,#30824,#30825);
#27704=AXIS2_PLACEMENT_3D('',#55794,#30827,#30828);
#27705=AXIS2_PLACEMENT_3D('',#55884,#30830,#30831);
#27706=AXIS2_PLACEMENT_3D('',#55968,#30833,#30834);
#27707=AXIS2_PLACEMENT_3D('',#56058,#30836,#30837);
#27708=AXIS2_PLACEMENT_3D('',#56148,#30839,#30840);
#27709=AXIS2_PLACEMENT_3D('',#56232,#30842,#30843);
#27710=AXIS2_PLACEMENT_3D('',#56322,#30845,#30846);
#27711=AXIS2_PLACEMENT_3D('',#56331,#30848,#30849);
#27712=AXIS2_PLACEMENT_3D('',#56332,#30850,#30851);
#27713=AXIS2_PLACEMENT_3D('',#56354,#30853,#30854);
#27714=AXIS2_PLACEMENT_3D('',#56369,#30855,#30856);
#27715=AXIS2_PLACEMENT_3D('',#56406,#30858,#30859);
#27716=AXIS2_PLACEMENT_3D('',#56443,#30861,#30862);
#27717=AXIS2_PLACEMENT_3D('',#56481,#30864,#30865);
#27718=AXIS2_PLACEMENT_3D('',#56518,#30867,#30868);
#27719=AXIS2_PLACEMENT_3D('',#56555,#30870,#30871);
#27720=AXIS2_PLACEMENT_3D('',#56592,#30873,#30874);
#27721=AXIS2_PLACEMENT_3D('',#56629,#30876,#30877);
#27722=AXIS2_PLACEMENT_3D('',#56667,#30879,#30880);
#27723=AXIS2_PLACEMENT_3D('',#56704,#30882,#30883);
#27724=AXIS2_PLACEMENT_3D('',#56741,#30885,#30886);
#27725=AXIS2_PLACEMENT_3D('',#56779,#30888,#30889);
#27726=AXIS2_PLACEMENT_3D('',#56816,#30891,#30892);
#27727=AXIS2_PLACEMENT_3D('',#56853,#30894,#30895);
#27728=AXIS2_PLACEMENT_3D('',#56890,#30897,#30898);
#27729=AXIS2_PLACEMENT_3D('',#56927,#30900,#30901);
#27730=AXIS2_PLACEMENT_3D('',#56965,#30903,#30904);
#27731=AXIS2_PLACEMENT_3D('',#57002,#30906,#30907);
#27732=AXIS2_PLACEMENT_3D('',#57078,#30908,#30909);
#27733=AXIS2_PLACEMENT_3D('',#57080,#30910,#30911);
#27734=AXIS2_PLACEMENT_3D('',#58239,#30912,#30913);
#27735=AXIS2_PLACEMENT_3D('',#58241,#30914,#30915);
#27736=AXIS2_PLACEMENT_3D('',#58242,#30916,#30917);
#27737=AXIS2_PLACEMENT_3D('',#58320,#30918,#30919);
#27738=AXIS2_PLACEMENT_3D('',#58321,#30920,#30921);
#27739=AXIS2_PLACEMENT_3D('',#59322,#30922,#30923);
#27740=AXIS2_PLACEMENT_3D('',#59326,#30925,#30926);
#27741=AXIS2_PLACEMENT_3D('',#59327,#30927,#30928);
#27742=AXIS2_PLACEMENT_3D('',#59330,#30930,#30931);
#27743=AXIS2_PLACEMENT_3D('',#59331,#30932,#30933);
#27744=AXIS2_PLACEMENT_3D('',#59334,#30935,#30936);
#27745=AXIS2_PLACEMENT_3D('',#59335,#30937,#30938);
#27746=AXIS2_PLACEMENT_3D('',#59338,#30940,#30941);
#27747=AXIS2_PLACEMENT_3D('',#59339,#30942,#30943);
#27748=AXIS2_PLACEMENT_3D('',#59342,#30945,#30946);
#27749=AXIS2_PLACEMENT_3D('',#59343,#30947,#30948);
#27750=AXIS2_PLACEMENT_3D('',#59345,#30950,#30951);
#27751=AXIS2_PLACEMENT_3D('',#59346,#30952,#30953);
#27752=AXIS2_PLACEMENT_3D('',#59351,#30955,#30956);
#27753=AXIS2_PLACEMENT_3D('',#59360,#30957,#30958);
#27754=AXIS2_PLACEMENT_3D('',#59369,#30959,#30960);
#27755=AXIS2_PLACEMENT_3D('',#59378,#30961,#30962);
#27756=AXIS2_PLACEMENT_3D('',#59387,#30963,#30964);
#27757=AXIS2_PLACEMENT_3D('',#59396,#30965,#30966);
#27758=AXIS2_PLACEMENT_3D('',#59404,#30967,#30968);
#27759=AXIS2_PLACEMENT_3D('',#59405,#30969,#30970);
#27760=AXIS2_PLACEMENT_3D('',#59411,#30974,#30975);
#27761=AXIS2_PLACEMENT_3D('',#59415,#30978,#30979);
#27762=AXIS2_PLACEMENT_3D('',#59419,#30982,#30983);
#27763=AXIS2_PLACEMENT_3D('',#59423,#30986,#30987);
#27764=AXIS2_PLACEMENT_3D('',#59427,#30990,#30991);
#27765=AXIS2_PLACEMENT_3D('',#59431,#30994,#30995);
#27766=AXIS2_PLACEMENT_3D('',#59435,#30998,#30999);
#27767=AXIS2_PLACEMENT_3D('',#59439,#31002,#31003);
#27768=AXIS2_PLACEMENT_3D('',#59443,#31006,#31007);
#27769=AXIS2_PLACEMENT_3D('',#59445,#31009,#31010);
#27770=AXIS2_PLACEMENT_3D('',#59447,#31012,#31013);
#27771=AXIS2_PLACEMENT_3D('',#59448,#31014,#31015);
#27772=AXIS2_PLACEMENT_3D('',#59450,#31017,#31018);
#27773=AXIS2_PLACEMENT_3D('',#59454,#31021,#31022);
#27774=AXIS2_PLACEMENT_3D('',#59456,#31024,#31025);
#27775=AXIS2_PLACEMENT_3D('',#59458,#31027,#31028);
#27776=AXIS2_PLACEMENT_3D('',#59462,#31031,#31032);
#27777=AXIS2_PLACEMENT_3D('',#59464,#31034,#31035);
#27778=AXIS2_PLACEMENT_3D('',#59465,#31036,#31037);
#27779=AXIS2_PLACEMENT_3D('',#59466,#31038,#31039);
#27780=AXIS2_PLACEMENT_3D('',#59468,#31041,#31042);
#27781=AXIS2_PLACEMENT_3D('',#59469,#31043,#31044);
#27782=AXIS2_PLACEMENT_3D('',#59470,#31045,#31046);
#27783=AXIS2_PLACEMENT_3D('',#59471,#31047,#31048);
#27784=AXIS2_PLACEMENT_3D('',#59473,#31049,#31050);
#27785=AXIS2_PLACEMENT_3D('',#59474,#31051,#31052);
#27786=AXIS2_PLACEMENT_3D('',#59476,#31054,#31055);
#27787=AXIS2_PLACEMENT_3D('',#59477,#31056,#31057);
#27788=AXIS2_PLACEMENT_3D('',#59478,#31058,#31059);
#27789=AXIS2_PLACEMENT_3D('',#59480,#31060,#31061);
#27790=AXIS2_PLACEMENT_3D('',#59482,#31063,#31064);
#27791=AXIS2_PLACEMENT_3D('',#59483,#31065,#31066);
#27792=AXIS2_PLACEMENT_3D('',#59763,#31068,#31069);
#27793=AXIS2_PLACEMENT_3D('',#59765,#31070,#31071);
#27794=AXIS2_PLACEMENT_3D('',#59768,#31073,#31074);
#27795=AXIS2_PLACEMENT_3D('',#59883,#31075,#31076);
#27796=AXIS2_PLACEMENT_3D('',#60182,#31081,#31082);
#27797=AXIS2_PLACEMENT_3D('',#60184,#31083,#31084);
#27798=AXIS2_PLACEMENT_3D('',#60187,#31086,#31087);
#27799=AXIS2_PLACEMENT_3D('',#60188,#31088,#31089);
#27800=AXIS2_PLACEMENT_3D('',#60207,#31090,#31091);
#27801=AXIS2_PLACEMENT_3D('',#60224,#31092,#31093);
#27802=AXIS2_PLACEMENT_3D('',#60226,#31095,#31096);
#27803=AXIS2_PLACEMENT_3D('',#60227,#31097,#31098);
#27804=AXIS2_PLACEMENT_3D('',#60229,#31099,#31100);
#27805=AXIS2_PLACEMENT_3D('',#60532,#31102,#31103);
#27806=AXIS2_PLACEMENT_3D('',#60593,#31105,#31106);
#27807=AXIS2_PLACEMENT_3D('',#60595,#31107,#31108);
#27808=AXIS2_PLACEMENT_3D('',#60598,#31110,#31111);
#27809=AXIS2_PLACEMENT_3D('',#60832,#31113,#31114);
#27810=AXIS2_PLACEMENT_3D('',#60833,#31115,#31116);
#27811=AXIS2_PLACEMENT_3D('',#60834,#31117,#31118);
#27812=AXIS2_PLACEMENT_3D('',#60835,#31119,#31120);
#27813=AXIS2_PLACEMENT_3D('',#60838,#31122,#31123);
#27814=AXIS2_PLACEMENT_3D('',#60839,#31124,#31125);
#27815=AXIS2_PLACEMENT_3D('',#60841,#31126,#31127);
#27816=AXIS2_PLACEMENT_3D('',#60842,#31128,#31129);
#27817=AXIS2_PLACEMENT_3D('',#60844,#31131,#31132);
#27818=AXIS2_PLACEMENT_3D('',#60846,#31134,#31135);
#27819=AXIS2_PLACEMENT_3D('',#60847,#31136,#31137);
#27820=AXIS2_PLACEMENT_3D('',#60860,#31144,#31145);
#27821=AXIS2_PLACEMENT_3D('',#60868,#31150,#31151);
#27822=AXIS2_PLACEMENT_3D('',#60872,#31154,#31155);
#27823=AXIS2_PLACEMENT_3D('',#60878,#31159,#31160);
#27824=AXIS2_PLACEMENT_3D('',#60891,#31167,#31168);
#27825=AXIS2_PLACEMENT_3D('',#60899,#31173,#31174);
#27826=AXIS2_PLACEMENT_3D('',#60903,#31177,#31178);
#27827=AXIS2_PLACEMENT_3D('',#60909,#31182,#31183);
#27828=AXIS2_PLACEMENT_3D('',#60922,#31190,#31191);
#27829=AXIS2_PLACEMENT_3D('',#60928,#31195,#31196);
#27830=AXIS2_PLACEMENT_3D('',#60934,#31200,#31201);
#27831=AXIS2_PLACEMENT_3D('',#60942,#31206,#31207);
#27832=AXIS2_PLACEMENT_3D('',#60955,#31214,#31215);
#27833=AXIS2_PLACEMENT_3D('',#60963,#31220,#31221);
#27834=AXIS2_PLACEMENT_3D('',#60967,#31224,#31225);
#27835=AXIS2_PLACEMENT_3D('',#60973,#31229,#31230);
#27836=AXIS2_PLACEMENT_3D('',#60986,#31237,#31238);
#27837=AXIS2_PLACEMENT_3D('',#60992,#31242,#31243);
#27838=AXIS2_PLACEMENT_3D('',#61000,#31248,#31249);
#27839=AXIS2_PLACEMENT_3D('',#61006,#31253,#31254);
#27840=AXIS2_PLACEMENT_3D('',#61019,#31261,#31262);
#27841=AXIS2_PLACEMENT_3D('',#61027,#31267,#31268);
#27842=AXIS2_PLACEMENT_3D('',#61035,#31273,#31274);
#27843=AXIS2_PLACEMENT_3D('',#61039,#31277,#31278);
#27844=AXIS2_PLACEMENT_3D('',#61047,#31283,#31284);
#27845=AXIS2_PLACEMENT_3D('',#61053,#31288,#31289);
#27846=AXIS2_PLACEMENT_3D('',#61066,#31296,#31297);
#27847=AXIS2_PLACEMENT_3D('',#61072,#31301,#31302);
#27848=AXIS2_PLACEMENT_3D('',#61078,#31306,#31307);
#27849=AXIS2_PLACEMENT_3D('',#61081,#31310,#31311);
#27850=AXIS2_PLACEMENT_3D('',#61094,#31318,#31319);
#27851=AXIS2_PLACEMENT_3D('',#61100,#31323,#31324);
#27852=AXIS2_PLACEMENT_3D('',#61108,#31329,#31330);
#27853=AXIS2_PLACEMENT_3D('',#61114,#31334,#31335);
#27854=AXIS2_PLACEMENT_3D('',#61127,#31342,#31343);
#27855=AXIS2_PLACEMENT_3D('',#61135,#31348,#31349);
#27856=AXIS2_PLACEMENT_3D('',#61143,#31354,#31355);
#27857=AXIS2_PLACEMENT_3D('',#61147,#31358,#31359);
#27858=AXIS2_PLACEMENT_3D('',#61155,#31364,#31365);
#27859=AXIS2_PLACEMENT_3D('',#61161,#31369,#31370);
#27860=AXIS2_PLACEMENT_3D('',#61174,#31377,#31378);
#27861=AXIS2_PLACEMENT_3D('',#61180,#31382,#31383);
#27862=AXIS2_PLACEMENT_3D('',#61186,#31387,#31388);
#27863=AXIS2_PLACEMENT_3D('',#61189,#31391,#31392);
#27864=AXIS2_PLACEMENT_3D('',#61202,#31399,#31400);
#27865=AXIS2_PLACEMENT_3D('',#61210,#31405,#31406);
#27866=AXIS2_PLACEMENT_3D('',#61218,#31411,#31412);
#27867=AXIS2_PLACEMENT_3D('',#61222,#31415,#31416);
#27868=AXIS2_PLACEMENT_3D('',#61230,#31421,#31422);
#27869=AXIS2_PLACEMENT_3D('',#61236,#31426,#31427);
#27870=AXIS2_PLACEMENT_3D('',#61249,#31434,#31435);
#27871=AXIS2_PLACEMENT_3D('',#61255,#31439,#31440);
#27872=AXIS2_PLACEMENT_3D('',#61261,#31444,#31445);
#27873=AXIS2_PLACEMENT_3D('',#61269,#31450,#31451);
#27874=AXIS2_PLACEMENT_3D('',#61279,#31457,#31458);
#27875=AXIS2_PLACEMENT_3D('',#61285,#31462,#31463);
#27876=AXIS2_PLACEMENT_3D('',#61291,#31467,#31468);
#27877=AXIS2_PLACEMENT_3D('',#61296,#31472,#31473);
#27878=AXIS2_PLACEMENT_3D('',#61309,#31480,#31481);
#27879=AXIS2_PLACEMENT_3D('',#61317,#31486,#31487);
#27880=AXIS2_PLACEMENT_3D('',#61325,#31492,#31493);
#27881=AXIS2_PLACEMENT_3D('',#61329,#31496,#31497);
#27882=AXIS2_PLACEMENT_3D('',#61337,#31502,#31503);
#27883=AXIS2_PLACEMENT_3D('',#61343,#31507,#31508);
#27884=AXIS2_PLACEMENT_3D('',#61356,#31515,#31516);
#27885=AXIS2_PLACEMENT_3D('',#61364,#31521,#31522);
#27886=AXIS2_PLACEMENT_3D('',#61372,#31527,#31528);
#27887=AXIS2_PLACEMENT_3D('',#61376,#31531,#31532);
#27888=AXIS2_PLACEMENT_3D('',#61384,#31537,#31538);
#27889=AXIS2_PLACEMENT_3D('',#61390,#31542,#31543);
#27890=AXIS2_PLACEMENT_3D('',#61403,#31550,#31551);
#27891=AXIS2_PLACEMENT_3D('',#61411,#31556,#31557);
#27892=AXIS2_PLACEMENT_3D('',#61415,#31560,#31561);
#27893=AXIS2_PLACEMENT_3D('',#61421,#31565,#31566);
#27894=AXIS2_PLACEMENT_3D('',#61434,#31573,#31574);
#27895=AXIS2_PLACEMENT_3D('',#61442,#31579,#31580);
#27896=AXIS2_PLACEMENT_3D('',#61450,#31585,#31586);
#27897=AXIS2_PLACEMENT_3D('',#61454,#31589,#31590);
#27898=AXIS2_PLACEMENT_3D('',#61462,#31595,#31596);
#27899=AXIS2_PLACEMENT_3D('',#61468,#31600,#31601);
#27900=AXIS2_PLACEMENT_3D('',#61481,#31608,#31609);
#27901=AXIS2_PLACEMENT_3D('',#61489,#31614,#31615);
#27902=AXIS2_PLACEMENT_3D('',#61497,#31620,#31621);
#27903=AXIS2_PLACEMENT_3D('',#61501,#31624,#31625);
#27904=AXIS2_PLACEMENT_3D('',#61509,#31630,#31631);
#27905=AXIS2_PLACEMENT_3D('',#61515,#31635,#31636);
#27906=AXIS2_PLACEMENT_3D('',#61525,#31642,#31643);
#27907=AXIS2_PLACEMENT_3D('',#61531,#31647,#31648);
#27908=AXIS2_PLACEMENT_3D('',#61535,#31651,#31652);
#27909=AXIS2_PLACEMENT_3D('',#61541,#31656,#31657);
#27910=AXIS2_PLACEMENT_3D('',#61550,#31662,#31663);
#27911=AXIS2_PLACEMENT_3D('',#61557,#31667,#31668);
#27912=AXIS2_PLACEMENT_3D('',#61558,#31669,#31670);
#27913=AXIS2_PLACEMENT_3D('',#61566,#31675,#31676);
#27914=AXIS2_PLACEMENT_3D('',#61578,#31683,#31684);
#27915=AXIS2_PLACEMENT_3D('',#61582,#31687,#31688);
#27916=AXIS2_PLACEMENT_3D('',#61592,#31694,#31695);
#27917=AXIS2_PLACEMENT_3D('',#61600,#31700,#31701);
#27918=AXIS2_PLACEMENT_3D('',#61602,#31703,#31704);
#27919=AXIS2_PLACEMENT_3D('',#61615,#31711,#31712);
#27920=AXIS2_PLACEMENT_3D('',#61622,#31717,#31718);
#27921=AXIS2_PLACEMENT_3D('',#61630,#31723,#31724);
#27922=AXIS2_PLACEMENT_3D('',#61634,#31727,#31728);
#27923=AXIS2_PLACEMENT_3D('',#61647,#31735,#31736);
#27924=AXIS2_PLACEMENT_3D('',#61655,#31741,#31742);
#27925=AXIS2_PLACEMENT_3D('',#61663,#31747,#31748);
#27926=AXIS2_PLACEMENT_3D('',#61667,#31751,#31752);
#27927=AXIS2_PLACEMENT_3D('',#61675,#31757,#31758);
#27928=AXIS2_PLACEMENT_3D('',#61681,#31762,#31763);
#27929=AXIS2_PLACEMENT_3D('',#61694,#31770,#31771);
#27930=AXIS2_PLACEMENT_3D('',#61702,#31776,#31777);
#27931=AXIS2_PLACEMENT_3D('',#61710,#31782,#31783);
#27932=AXIS2_PLACEMENT_3D('',#61714,#31786,#31787);
#27933=AXIS2_PLACEMENT_3D('',#61722,#31792,#31793);
#27934=AXIS2_PLACEMENT_3D('',#61728,#31797,#31798);
#27935=AXIS2_PLACEMENT_3D('',#61741,#31805,#31806);
#27936=AXIS2_PLACEMENT_3D('',#61749,#31811,#31812);
#27937=AXIS2_PLACEMENT_3D('',#61757,#31817,#31818);
#27938=AXIS2_PLACEMENT_3D('',#61761,#31821,#31822);
#27939=AXIS2_PLACEMENT_3D('',#61769,#31827,#31828);
#27940=AXIS2_PLACEMENT_3D('',#61775,#31832,#31833);
#27941=AXIS2_PLACEMENT_3D('',#61788,#31840,#31841);
#27942=AXIS2_PLACEMENT_3D('',#61796,#31846,#31847);
#27943=AXIS2_PLACEMENT_3D('',#61804,#31852,#31853);
#27944=AXIS2_PLACEMENT_3D('',#61808,#31856,#31857);
#27945=AXIS2_PLACEMENT_3D('',#61816,#31862,#31863);
#27946=AXIS2_PLACEMENT_3D('',#61822,#31867,#31868);
#27947=AXIS2_PLACEMENT_3D('',#61835,#31875,#31876);
#27948=AXIS2_PLACEMENT_3D('',#61841,#31880,#31881);
#27949=AXIS2_PLACEMENT_3D('',#61847,#31885,#31886);
#27950=AXIS2_PLACEMENT_3D('',#61850,#31889,#31890);
#27951=AXIS2_PLACEMENT_3D('',#61853,#31893,#31894);
#27952=AXIS2_PLACEMENT_3D('',#61857,#31897,#31898);
#27953=AXIS2_PLACEMENT_3D('',#61859,#31900,#31901);
#27954=AXIS2_PLACEMENT_3D('',#61862,#31904,#31905);
#27955=AXIS2_PLACEMENT_3D('',#61866,#31908,#31909);
#27956=AXIS2_PLACEMENT_3D('',#61870,#31912,#31913);
#27957=AXIS2_PLACEMENT_3D('',#61872,#31915,#31916);
#27958=AXIS2_PLACEMENT_3D('',#61875,#31919,#31920);
#27959=AXIS2_PLACEMENT_3D('',#61879,#31923,#31924);
#27960=AXIS2_PLACEMENT_3D('',#61881,#31926,#31927);
#27961=AXIS2_PLACEMENT_3D('',#62015,#32003,#32004);
#27962=AXIS2_PLACEMENT_3D('',#62017,#32006,#32007);
#27963=AXIS2_PLACEMENT_3D('',#62021,#32010,#32011);
#27964=AXIS2_PLACEMENT_3D('',#62023,#32013,#32014);
#27965=AXIS2_PLACEMENT_3D('',#62025,#32016,#32017);
#27966=AXIS2_PLACEMENT_3D('',#62029,#32020,#32021);
#27967=AXIS2_PLACEMENT_3D('',#62033,#32024,#32025);
#27968=AXIS2_PLACEMENT_3D('',#62035,#32027,#32028);
#27969=AXIS2_PLACEMENT_3D('',#62037,#32030,#32031);
#27970=AXIS2_PLACEMENT_3D('',#62041,#32034,#32035);
#27971=AXIS2_PLACEMENT_3D('',#62045,#32038,#32039);
#27972=AXIS2_PLACEMENT_3D('',#62047,#32041,#32042);
#27973=AXIS2_PLACEMENT_3D('',#62049,#32044,#32045);
#27974=AXIS2_PLACEMENT_3D('',#62053,#32048,#32049);
#27975=AXIS2_PLACEMENT_3D('',#62057,#32052,#32053);
#27976=AXIS2_PLACEMENT_3D('',#62059,#32055,#32056);
#27977=AXIS2_PLACEMENT_3D('',#62063,#32059,#32060);
#27978=AXIS2_PLACEMENT_3D('',#62067,#32063,#32064);
#27979=AXIS2_PLACEMENT_3D('',#62071,#32067,#32068);
#27980=AXIS2_PLACEMENT_3D('',#62080,#32073,#32074);
#27981=AXIS2_PLACEMENT_3D('',#62087,#32079,#32080);
#27982=AXIS2_PLACEMENT_3D('',#62090,#32083,#32084);
#27983=AXIS2_PLACEMENT_3D('',#62096,#32088,#32089);
#27984=AXIS2_PLACEMENT_3D('',#62102,#32093,#32094);
#27985=AXIS2_PLACEMENT_3D('',#62107,#32098,#32099);
#27986=AXIS2_PLACEMENT_3D('',#62115,#32104,#32105);
#27987=AXIS2_PLACEMENT_3D('',#62119,#32108,#32109);
#27988=AXIS2_PLACEMENT_3D('',#62132,#32116,#32117);
#27989=AXIS2_PLACEMENT_3D('',#62137,#32121,#32122);
#27990=AXIS2_PLACEMENT_3D('',#62143,#32126,#32127);
#27991=AXIS2_PLACEMENT_3D('',#62147,#32130,#32131);
#27992=AXIS2_PLACEMENT_3D('',#62155,#32136,#32137);
#27993=AXIS2_PLACEMENT_3D('',#62157,#32139,#32140);
#27994=AXIS2_PLACEMENT_3D('',#62159,#32142,#32143);
#27995=AXIS2_PLACEMENT_3D('',#62161,#32145,#32146);
#27996=AXIS2_PLACEMENT_3D('',#62165,#32149,#32150);
#27997=AXIS2_PLACEMENT_3D('',#62169,#32153,#32154);
#27998=AXIS2_PLACEMENT_3D('',#62171,#32156,#32157);
#27999=AXIS2_PLACEMENT_3D('',#62173,#32159,#32160);
#28000=AXIS2_PLACEMENT_3D('',#62177,#32163,#32164);
#28001=AXIS2_PLACEMENT_3D('',#62179,#32166,#32167);
#28002=AXIS2_PLACEMENT_3D('',#62181,#32169,#32170);
#28003=AXIS2_PLACEMENT_3D('',#62185,#32173,#32174);
#28004=AXIS2_PLACEMENT_3D('',#62189,#32177,#32178);
#28005=AXIS2_PLACEMENT_3D('',#62191,#32180,#32181);
#28006=AXIS2_PLACEMENT_3D('',#62193,#32183,#32184);
#28007=AXIS2_PLACEMENT_3D('',#62195,#32186,#32187);
#28008=AXIS2_PLACEMENT_3D('',#62199,#32190,#32191);
#28009=AXIS2_PLACEMENT_3D('',#62201,#32193,#32194);
#28010=AXIS2_PLACEMENT_3D('',#62203,#32196,#32197);
#28011=AXIS2_PLACEMENT_3D('',#62207,#32200,#32201);
#28012=AXIS2_PLACEMENT_3D('',#62209,#32203,#32204);
#28013=AXIS2_PLACEMENT_3D('',#62211,#32206,#32207);
#28014=AXIS2_PLACEMENT_3D('',#62215,#32210,#32211);
#28015=AXIS2_PLACEMENT_3D('',#62217,#32213,#32214);
#28016=AXIS2_PLACEMENT_3D('',#62219,#32216,#32217);
#28017=AXIS2_PLACEMENT_3D('',#62223,#32220,#32221);
#28018=AXIS2_PLACEMENT_3D('',#62225,#32223,#32224);
#28019=AXIS2_PLACEMENT_3D('',#62227,#32226,#32227);
#28020=AXIS2_PLACEMENT_3D('',#62231,#32230,#32231);
#28021=AXIS2_PLACEMENT_3D('',#62235,#32234,#32235);
#28022=AXIS2_PLACEMENT_3D('',#62237,#32237,#32238);
#28023=AXIS2_PLACEMENT_3D('',#62250,#32245,#32246);
#28024=AXIS2_PLACEMENT_3D('',#62255,#32250,#32251);
#28025=AXIS2_PLACEMENT_3D('',#62261,#32255,#32256);
#28026=AXIS2_PLACEMENT_3D('',#62265,#32259,#32260);
#28027=AXIS2_PLACEMENT_3D('',#62273,#32265,#32266);
#28028=AXIS2_PLACEMENT_3D('',#62277,#32269,#32270);
#28029=AXIS2_PLACEMENT_3D('',#62290,#32277,#32278);
#28030=AXIS2_PLACEMENT_3D('',#62295,#32282,#32283);
#28031=AXIS2_PLACEMENT_3D('',#62301,#32287,#32288);
#28032=AXIS2_PLACEMENT_3D('',#62305,#32291,#32292);
#28033=AXIS2_PLACEMENT_3D('',#62313,#32297,#32298);
#28034=AXIS2_PLACEMENT_3D('',#62317,#32301,#32302);
#28035=AXIS2_PLACEMENT_3D('',#62330,#32309,#32310);
#28036=AXIS2_PLACEMENT_3D('',#62335,#32314,#32315);
#28037=AXIS2_PLACEMENT_3D('',#62341,#32319,#32320);
#28038=AXIS2_PLACEMENT_3D('',#62345,#32323,#32324);
#28039=AXIS2_PLACEMENT_3D('',#62353,#32329,#32330);
#28040=AXIS2_PLACEMENT_3D('',#62357,#32333,#32334);
#28041=AXIS2_PLACEMENT_3D('',#62370,#32341,#32342);
#28042=AXIS2_PLACEMENT_3D('',#62376,#32346,#32347);
#28043=AXIS2_PLACEMENT_3D('',#62379,#32350,#32351);
#28044=AXIS2_PLACEMENT_3D('',#62385,#32355,#32356);
#28045=AXIS2_PLACEMENT_3D('',#62395,#32362,#32363);
#28046=AXIS2_PLACEMENT_3D('',#62401,#32367,#32368);
#28047=AXIS2_PLACEMENT_3D('',#62407,#32372,#32373);
#28048=AXIS2_PLACEMENT_3D('',#62412,#32377,#32378);
#28049=AXIS2_PLACEMENT_3D('',#62425,#32385,#32386);
#28050=AXIS2_PLACEMENT_3D('',#62430,#32390,#32391);
#28051=AXIS2_PLACEMENT_3D('',#62436,#32395,#32396);
#28052=AXIS2_PLACEMENT_3D('',#62440,#32399,#32400);
#28053=AXIS2_PLACEMENT_3D('',#62448,#32405,#32406);
#28054=AXIS2_PLACEMENT_3D('',#62452,#32409,#32410);
#28055=AXIS2_PLACEMENT_3D('',#62465,#32417,#32418);
#28056=AXIS2_PLACEMENT_3D('',#62470,#32422,#32423);
#28057=AXIS2_PLACEMENT_3D('',#62476,#32427,#32428);
#28058=AXIS2_PLACEMENT_3D('',#62480,#32431,#32432);
#28059=AXIS2_PLACEMENT_3D('',#62488,#32437,#32438);
#28060=AXIS2_PLACEMENT_3D('',#62492,#32441,#32442);
#28061=AXIS2_PLACEMENT_3D('',#62500,#32447,#32448);
#28062=AXIS2_PLACEMENT_3D('',#62508,#32453,#32454);
#28063=AXIS2_PLACEMENT_3D('',#62512,#32457,#32458);
#28064=AXIS2_PLACEMENT_3D('',#62514,#32460,#32461);
#28065=AXIS2_PLACEMENT_3D('',#62516,#32463,#32464);
#28066=AXIS2_PLACEMENT_3D('',#62520,#32467,#32468);
#28067=AXIS2_PLACEMENT_3D('',#62522,#32470,#32471);
#28068=AXIS2_PLACEMENT_3D('',#62524,#32473,#32474);
#28069=AXIS2_PLACEMENT_3D('',#62528,#32477,#32478);
#28070=AXIS2_PLACEMENT_3D('',#62532,#32481,#32482);
#28071=AXIS2_PLACEMENT_3D('',#62534,#32484,#32485);
#28072=AXIS2_PLACEMENT_3D('',#62536,#32487,#32488);
#28073=AXIS2_PLACEMENT_3D('',#62538,#32490,#32491);
#28074=AXIS2_PLACEMENT_3D('',#62542,#32494,#32495);
#28075=AXIS2_PLACEMENT_3D('',#62544,#32497,#32498);
#28076=AXIS2_PLACEMENT_3D('',#62546,#32500,#32501);
#28077=AXIS2_PLACEMENT_3D('',#62550,#32504,#32505);
#28078=AXIS2_PLACEMENT_3D('',#62552,#32507,#32508);
#28079=AXIS2_PLACEMENT_3D('',#62554,#32510,#32511);
#28080=AXIS2_PLACEMENT_3D('',#62558,#32514,#32515);
#28081=AXIS2_PLACEMENT_3D('',#62562,#32518,#32519);
#28082=AXIS2_PLACEMENT_3D('',#62564,#32521,#32522);
#28083=AXIS2_PLACEMENT_3D('',#62566,#32524,#32525);
#28084=AXIS2_PLACEMENT_3D('',#62570,#32528,#32529);
#28085=AXIS2_PLACEMENT_3D('',#62574,#32532,#32533);
#28086=AXIS2_PLACEMENT_3D('',#62576,#32535,#32536);
#28087=AXIS2_PLACEMENT_3D('',#62578,#32538,#32539);
#28088=AXIS2_PLACEMENT_3D('',#62582,#32542,#32543);
#28089=AXIS2_PLACEMENT_3D('',#62584,#32545,#32546);
#28090=AXIS2_PLACEMENT_3D('',#62586,#32548,#32549);
#28091=AXIS2_PLACEMENT_3D('',#62590,#32552,#32553);
#28092=AXIS2_PLACEMENT_3D('',#62592,#32555,#32556);
#28093=AXIS2_PLACEMENT_3D('',#62594,#32558,#32559);
#28094=AXIS2_PLACEMENT_3D('',#62598,#32562,#32563);
#28095=AXIS2_PLACEMENT_3D('',#62602,#32566,#32567);
#28096=AXIS2_PLACEMENT_3D('',#62604,#32569,#32570);
#28097=AXIS2_PLACEMENT_3D('',#62617,#32577,#32578);
#28098=AXIS2_PLACEMENT_3D('',#62622,#32582,#32583);
#28099=AXIS2_PLACEMENT_3D('',#62628,#32587,#32588);
#28100=AXIS2_PLACEMENT_3D('',#62632,#32591,#32592);
#28101=AXIS2_PLACEMENT_3D('',#62640,#32597,#32598);
#28102=AXIS2_PLACEMENT_3D('',#62644,#32601,#32602);
#28103=AXIS2_PLACEMENT_3D('',#62657,#32609,#32610);
#28104=AXIS2_PLACEMENT_3D('',#62662,#32614,#32615);
#28105=AXIS2_PLACEMENT_3D('',#62668,#32619,#32620);
#28106=AXIS2_PLACEMENT_3D('',#62672,#32623,#32624);
#28107=AXIS2_PLACEMENT_3D('',#62680,#32629,#32630);
#28108=AXIS2_PLACEMENT_3D('',#62684,#32633,#32634);
#28109=AXIS2_PLACEMENT_3D('',#62697,#32641,#32642);
#28110=AXIS2_PLACEMENT_3D('',#62702,#32646,#32647);
#28111=AXIS2_PLACEMENT_3D('',#62708,#32651,#32652);
#28112=AXIS2_PLACEMENT_3D('',#62712,#32655,#32656);
#28113=AXIS2_PLACEMENT_3D('',#62720,#32661,#32662);
#28114=AXIS2_PLACEMENT_3D('',#62724,#32665,#32666);
#28115=AXIS2_PLACEMENT_3D('',#62737,#32673,#32674);
#28116=AXIS2_PLACEMENT_3D('',#62742,#32678,#32679);
#28117=AXIS2_PLACEMENT_3D('',#62748,#32683,#32684);
#28118=AXIS2_PLACEMENT_3D('',#62752,#32687,#32688);
#28119=AXIS2_PLACEMENT_3D('',#62760,#32693,#32694);
#28120=AXIS2_PLACEMENT_3D('',#62764,#32697,#32698);
#28121=AXIS2_PLACEMENT_3D('',#62777,#32705,#32706);
#28122=AXIS2_PLACEMENT_3D('',#62782,#32710,#32711);
#28123=AXIS2_PLACEMENT_3D('',#62788,#32715,#32716);
#28124=AXIS2_PLACEMENT_3D('',#62792,#32719,#32720);
#28125=AXIS2_PLACEMENT_3D('',#62800,#32725,#32726);
#28126=AXIS2_PLACEMENT_3D('',#62804,#32729,#32730);
#28127=AXIS2_PLACEMENT_3D('',#62817,#32737,#32738);
#28128=AXIS2_PLACEMENT_3D('',#62822,#32742,#32743);
#28129=AXIS2_PLACEMENT_3D('',#62828,#32747,#32748);
#28130=AXIS2_PLACEMENT_3D('',#62832,#32751,#32752);
#28131=AXIS2_PLACEMENT_3D('',#62840,#32757,#32758);
#28132=AXIS2_PLACEMENT_3D('',#62844,#32761,#32762);
#28133=AXIS2_PLACEMENT_3D('',#62852,#32767,#32768);
#28134=AXIS2_PLACEMENT_3D('',#62860,#32773,#32774);
#28135=AXIS2_PLACEMENT_3D('',#62864,#32777,#32778);
#28136=AXIS2_PLACEMENT_3D('',#62866,#32780,#32781);
#28137=AXIS2_PLACEMENT_3D('',#62868,#32783,#32784);
#28138=AXIS2_PLACEMENT_3D('',#62872,#32787,#32788);
#28139=AXIS2_PLACEMENT_3D('',#62874,#32790,#32791);
#28140=AXIS2_PLACEMENT_3D('',#62876,#32793,#32794);
#28141=AXIS2_PLACEMENT_3D('',#62880,#32797,#32798);
#28142=AXIS2_PLACEMENT_3D('',#62884,#32801,#32802);
#28143=AXIS2_PLACEMENT_3D('',#62886,#32804,#32805);
#28144=AXIS2_PLACEMENT_3D('',#62888,#32807,#32808);
#28145=AXIS2_PLACEMENT_3D('',#62892,#32811,#32812);
#28146=AXIS2_PLACEMENT_3D('',#62896,#32815,#32816);
#28147=AXIS2_PLACEMENT_3D('',#62898,#32818,#32819);
#28148=AXIS2_PLACEMENT_3D('',#62900,#32821,#32822);
#28149=AXIS2_PLACEMENT_3D('',#62904,#32825,#32826);
#28150=AXIS2_PLACEMENT_3D('',#62908,#32829,#32830);
#28151=AXIS2_PLACEMENT_3D('',#62910,#32832,#32833);
#28152=AXIS2_PLACEMENT_3D('',#62912,#32835,#32836);
#28153=AXIS2_PLACEMENT_3D('',#62916,#32839,#32840);
#28154=AXIS2_PLACEMENT_3D('',#62920,#32843,#32844);
#28155=AXIS2_PLACEMENT_3D('',#62922,#32846,#32847);
#28156=AXIS2_PLACEMENT_3D('',#62924,#32849,#32850);
#28157=AXIS2_PLACEMENT_3D('',#62928,#32853,#32854);
#28158=AXIS2_PLACEMENT_3D('',#62932,#32857,#32858);
#28159=AXIS2_PLACEMENT_3D('',#62934,#32860,#32861);
#28160=AXIS2_PLACEMENT_3D('',#62937,#32864,#32865);
#28161=AXIS2_PLACEMENT_3D('',#62941,#32868,#32869);
#28162=AXIS2_PLACEMENT_3D('',#62943,#32871,#32872);
#28163=AXIS2_PLACEMENT_3D('',#62945,#32874,#32875);
#28164=AXIS2_PLACEMENT_3D('',#62951,#32879,#32880);
#28165=AXIS2_PLACEMENT_3D('',#62955,#32883,#32884);
#28166=AXIS2_PLACEMENT_3D('',#62959,#32887,#32888);
#28167=AXIS2_PLACEMENT_3D('',#63178,#33003,#33004);
#28168=AXIS2_PLACEMENT_3D('',#63179,#33005,#33006);
#28169=AXIS2_PLACEMENT_3D('',#63181,#33008,#33009);
#28170=AXIS2_PLACEMENT_3D('',#63184,#33012,#33013);
#28171=AXIS2_PLACEMENT_3D('',#63186,#33015,#33016);
#28172=AXIS2_PLACEMENT_3D('',#63188,#33018,#33019);
#28173=AXIS2_PLACEMENT_3D('',#63189,#33020,#33021);
#28174=AXIS2_PLACEMENT_3D('',#63192,#33024,#33025);
#28175=AXIS2_PLACEMENT_3D('',#63194,#33027,#33028);
#28176=AXIS2_PLACEMENT_3D('',#63196,#33030,#33031);
#28177=AXIS2_PLACEMENT_3D('',#63197,#33032,#33033);
#28178=AXIS2_PLACEMENT_3D('',#63200,#33036,#33037);
#28179=AXIS2_PLACEMENT_3D('',#63202,#33039,#33040);
#28180=AXIS2_PLACEMENT_3D('',#63204,#33042,#33043);
#28181=AXIS2_PLACEMENT_3D('',#63205,#33044,#33045);
#28182=AXIS2_PLACEMENT_3D('',#63207,#33047,#33048);
#28183=AXIS2_PLACEMENT_3D('',#63209,#33050,#33051);
#28184=AXIS2_PLACEMENT_3D('',#63211,#33053,#33054);
#28185=AXIS2_PLACEMENT_3D('',#63214,#33057,#33058);
#28186=AXIS2_PLACEMENT_3D('',#63216,#33060,#33061);
#28187=AXIS2_PLACEMENT_3D('',#63218,#33063,#33064);
#28188=AXIS2_PLACEMENT_3D('',#63219,#33065,#33066);
#28189=AXIS2_PLACEMENT_3D('',#63222,#33069,#33070);
#28190=AXIS2_PLACEMENT_3D('',#63223,#33071,#33072);
#28191=AXIS2_PLACEMENT_3D('',#63225,#33074,#33075);
#28192=AXIS2_PLACEMENT_3D('',#63227,#33077,#33078);
#28193=AXIS2_PLACEMENT_3D('',#63230,#33081,#33082);
#28194=AXIS2_PLACEMENT_3D('',#63232,#33084,#33085);
#28195=AXIS2_PLACEMENT_3D('',#63234,#33087,#33088);
#28196=AXIS2_PLACEMENT_3D('',#63235,#33089,#33090);
#28197=AXIS2_PLACEMENT_3D('',#63238,#33093,#33094);
#28198=AXIS2_PLACEMENT_3D('',#63240,#33096,#33097);
#28199=AXIS2_PLACEMENT_3D('',#63242,#33099,#33100);
#28200=AXIS2_PLACEMENT_3D('',#63243,#33101,#33102);
#28201=AXIS2_PLACEMENT_3D('',#63246,#33105,#33106);
#28202=AXIS2_PLACEMENT_3D('',#63248,#33108,#33109);
#28203=AXIS2_PLACEMENT_3D('',#63250,#33111,#33112);
#28204=AXIS2_PLACEMENT_3D('',#63251,#33113,#33114);
#28205=AXIS2_PLACEMENT_3D('',#63254,#33117,#33118);
#28206=AXIS2_PLACEMENT_3D('',#63256,#33120,#33121);
#28207=AXIS2_PLACEMENT_3D('',#63258,#33123,#33124);
#28208=AXIS2_PLACEMENT_3D('',#63259,#33125,#33126);
#28209=AXIS2_PLACEMENT_3D('',#63262,#33129,#33130);
#28210=AXIS2_PLACEMENT_3D('',#63264,#33132,#33133);
#28211=AXIS2_PLACEMENT_3D('',#63266,#33135,#33136);
#28212=AXIS2_PLACEMENT_3D('',#63267,#33137,#33138);
#28213=AXIS2_PLACEMENT_3D('',#63270,#33141,#33142);
#28214=AXIS2_PLACEMENT_3D('',#63271,#33143,#33144);
#28215=AXIS2_PLACEMENT_3D('',#63272,#33145,#33146);
#28216=AXIS2_PLACEMENT_3D('',#63275,#33149,#33150);
#28217=AXIS2_PLACEMENT_3D('',#63277,#33152,#33153);
#28218=AXIS2_PLACEMENT_3D('',#63279,#33155,#33156);
#28219=AXIS2_PLACEMENT_3D('',#63280,#33157,#33158);
#28220=AXIS2_PLACEMENT_3D('',#63283,#33161,#33162);
#28221=AXIS2_PLACEMENT_3D('',#63285,#33164,#33165);
#28222=AXIS2_PLACEMENT_3D('',#63287,#33167,#33168);
#28223=AXIS2_PLACEMENT_3D('',#63288,#33169,#33170);
#28224=AXIS2_PLACEMENT_3D('',#63290,#33172,#33173);
#28225=AXIS2_PLACEMENT_3D('',#63292,#33175,#33176);
#28226=AXIS2_PLACEMENT_3D('',#63294,#33178,#33179);
#28227=AXIS2_PLACEMENT_3D('',#63297,#33182,#33183);
#28228=AXIS2_PLACEMENT_3D('',#63299,#33185,#33186);
#28229=AXIS2_PLACEMENT_3D('',#63301,#33188,#33189);
#28230=AXIS2_PLACEMENT_3D('',#63302,#33190,#33191);
#28231=AXIS2_PLACEMENT_3D('',#63305,#33194,#33195);
#28232=AXIS2_PLACEMENT_3D('',#63307,#33197,#33198);
#28233=AXIS2_PLACEMENT_3D('',#63309,#33200,#33201);
#28234=AXIS2_PLACEMENT_3D('',#63310,#33202,#33203);
#28235=AXIS2_PLACEMENT_3D('',#63313,#33206,#33207);
#28236=AXIS2_PLACEMENT_3D('',#63315,#33209,#33210);
#28237=AXIS2_PLACEMENT_3D('',#63316,#33211,#33212);
#28238=AXIS2_PLACEMENT_3D('',#63318,#33214,#33215);
#28239=AXIS2_PLACEMENT_3D('',#63320,#33217,#33218);
#28240=AXIS2_PLACEMENT_3D('',#63323,#33221,#33222);
#28241=AXIS2_PLACEMENT_3D('',#63325,#33224,#33225);
#28242=AXIS2_PLACEMENT_3D('',#63327,#33227,#33228);
#28243=AXIS2_PLACEMENT_3D('',#63328,#33229,#33230);
#28244=AXIS2_PLACEMENT_3D('',#63331,#33233,#33234);
#28245=AXIS2_PLACEMENT_3D('',#63332,#33235,#33236);
#28246=AXIS2_PLACEMENT_3D('',#63333,#33237,#33238);
#28247=AXIS2_PLACEMENT_3D('',#63336,#33241,#33242);
#28248=AXIS2_PLACEMENT_3D('',#63338,#33244,#33245);
#28249=AXIS2_PLACEMENT_3D('',#63340,#33247,#33248);
#28250=AXIS2_PLACEMENT_3D('',#63341,#33249,#33250);
#28251=AXIS2_PLACEMENT_3D('',#63344,#33253,#33254);
#28252=AXIS2_PLACEMENT_3D('',#63346,#33256,#33257);
#28253=AXIS2_PLACEMENT_3D('',#63348,#33259,#33260);
#28254=AXIS2_PLACEMENT_3D('',#63349,#33261,#33262);
#28255=AXIS2_PLACEMENT_3D('',#63351,#33264,#33265);
#28256=AXIS2_PLACEMENT_3D('',#63353,#33267,#33268);
#28257=AXIS2_PLACEMENT_3D('',#63355,#33270,#33271);
#28258=AXIS2_PLACEMENT_3D('',#63358,#33274,#33275);
#28259=AXIS2_PLACEMENT_3D('',#63360,#33277,#33278);
#28260=AXIS2_PLACEMENT_3D('',#63361,#33279,#33280);
#28261=AXIS2_PLACEMENT_3D('',#63363,#33282,#33283);
#28262=AXIS2_PLACEMENT_3D('',#63365,#33285,#33286);
#28263=AXIS2_PLACEMENT_3D('',#63368,#33289,#33290);
#28264=AXIS2_PLACEMENT_3D('',#63370,#33292,#33293);
#28265=AXIS2_PLACEMENT_3D('',#63372,#33295,#33296);
#28266=AXIS2_PLACEMENT_3D('',#63373,#33297,#33298);
#28267=AXIS2_PLACEMENT_3D('',#63376,#33301,#33302);
#28268=AXIS2_PLACEMENT_3D('',#63377,#33303,#33304);
#28269=AXIS2_PLACEMENT_3D('',#63378,#33305,#33306);
#28270=AXIS2_PLACEMENT_3D('',#63382,#33309,#33310);
#28271=AXIS2_PLACEMENT_3D('',#63385,#33313,#33314);
#28272=AXIS2_PLACEMENT_3D('',#63387,#33316,#33317);
#28273=AXIS2_PLACEMENT_3D('',#63389,#33319,#33320);
#28274=AXIS2_PLACEMENT_3D('',#63390,#33321,#33322);
#28275=AXIS2_PLACEMENT_3D('',#63393,#33325,#33326);
#28276=AXIS2_PLACEMENT_3D('',#63395,#33328,#33329);
#28277=AXIS2_PLACEMENT_3D('',#63396,#33330,#33331);
#28278=AXIS2_PLACEMENT_3D('',#63645,#33333,#33334);
#28279=AXIS2_PLACEMENT_3D('',#63647,#33335,#33336);
#28280=AXIS2_PLACEMENT_3D('',#63649,#33338,#33339);
#28281=AXIS2_PLACEMENT_3D('',#63651,#33340,#33341);
#28282=AXIS2_PLACEMENT_3D('',#63654,#33343,#33344);
#28283=AXIS2_PLACEMENT_3D('',#63655,#33345,#33346);
#28284=AXIS2_PLACEMENT_3D('',#63657,#33348,#33349);
#28285=AXIS2_PLACEMENT_3D('',#63659,#33351,#33352);
#28286=AXIS2_PLACEMENT_3D('',#63662,#33354,#33355);
#28287=AXIS2_PLACEMENT_3D('',#63666,#33358,#33359);
#28288=AXIS2_PLACEMENT_3D('',#63668,#33361,#33362);
#28289=AXIS2_PLACEMENT_3D('',#63672,#33365,#33366);
#28290=AXIS2_PLACEMENT_3D('',#63673,#33367,#33368);
#28291=AXIS2_PLACEMENT_3D('',#63674,#33369,#33370);
#28292=AXIS2_PLACEMENT_3D('',#63675,#33371,#33372);
#28293=AXIS2_PLACEMENT_3D('',#63676,#33373,#33374);
#28294=AXIS2_PLACEMENT_3D('',#63677,#33375,#33376);
#28295=AXIS2_PLACEMENT_3D('',#63678,#33377,#33378);
#28296=AXIS2_PLACEMENT_3D('',#63680,#33380,#33381);
#28297=AXIS2_PLACEMENT_3D('',#63681,#33382,#33383);
#28298=AXIS2_PLACEMENT_3D('',#63682,#33384,#33385);
#28299=AXIS2_PLACEMENT_3D('',#63683,#33386,#33387);
#28300=AXIS2_PLACEMENT_3D('',#63687,#33390,#33391);
#28301=AXIS2_PLACEMENT_3D('',#63689,#33393,#33394);
#28302=AXIS2_PLACEMENT_3D('',#63691,#33396,#33397);
#28303=AXIS2_PLACEMENT_3D('',#63692,#33398,#33399);
#28304=AXIS2_PLACEMENT_3D('',#63693,#33400,#33401);
#28305=AXIS2_PLACEMENT_3D('',#63694,#33402,#33403);
#28306=AXIS2_PLACEMENT_3D('',#63695,#33404,#33405);
#28307=AXIS2_PLACEMENT_3D('',#63704,#33410,#33411);
#28308=AXIS2_PLACEMENT_3D('',#63706,#33412,#33413);
#28309=AXIS2_PLACEMENT_3D('',#63709,#33415,#33416);
#28310=AXIS2_PLACEMENT_3D('',#63710,#33417,#33418);
#28311=AXIS2_PLACEMENT_3D('',#63716,#33422,#33423);
#28312=AXIS2_PLACEMENT_3D('',#63725,#33428,#33429);
#28313=AXIS2_PLACEMENT_3D('',#63727,#33430,#33431);
#28314=AXIS2_PLACEMENT_3D('',#63730,#33433,#33434);
#28315=AXIS2_PLACEMENT_3D('',#63731,#33435,#33436);
#28316=AXIS2_PLACEMENT_3D('',#63737,#33440,#33441);
#28317=AXIS2_PLACEMENT_3D('',#63746,#33446,#33447);
#28318=AXIS2_PLACEMENT_3D('',#63748,#33448,#33449);
#28319=AXIS2_PLACEMENT_3D('',#63751,#33451,#33452);
#28320=AXIS2_PLACEMENT_3D('',#63752,#33453,#33454);
#28321=AXIS2_PLACEMENT_3D('',#63758,#33458,#33459);
#28322=AXIS2_PLACEMENT_3D('',#63767,#33464,#33465);
#28323=AXIS2_PLACEMENT_3D('',#63769,#33466,#33467);
#28324=AXIS2_PLACEMENT_3D('',#63772,#33469,#33470);
#28325=AXIS2_PLACEMENT_3D('',#63773,#33471,#33472);
#28326=AXIS2_PLACEMENT_3D('',#63779,#33476,#33477);
#28327=AXIS2_PLACEMENT_3D('',#63788,#33482,#33483);
#28328=AXIS2_PLACEMENT_3D('',#63790,#33484,#33485);
#28329=AXIS2_PLACEMENT_3D('',#63793,#33487,#33488);
#28330=AXIS2_PLACEMENT_3D('',#63794,#33489,#33490);
#28331=AXIS2_PLACEMENT_3D('',#63800,#33494,#33495);
#28332=AXIS2_PLACEMENT_3D('',#63809,#33500,#33501);
#28333=AXIS2_PLACEMENT_3D('',#63811,#33502,#33503);
#28334=AXIS2_PLACEMENT_3D('',#63814,#33505,#33506);
#28335=AXIS2_PLACEMENT_3D('',#63815,#33507,#33508);
#28336=AXIS2_PLACEMENT_3D('',#63821,#33512,#33513);
#28337=AXIS2_PLACEMENT_3D('',#63830,#33518,#33519);
#28338=AXIS2_PLACEMENT_3D('',#63832,#33520,#33521);
#28339=AXIS2_PLACEMENT_3D('',#63835,#33523,#33524);
#28340=AXIS2_PLACEMENT_3D('',#63836,#33525,#33526);
#28341=AXIS2_PLACEMENT_3D('',#63842,#33530,#33531);
#28342=AXIS2_PLACEMENT_3D('',#63851,#33536,#33537);
#28343=AXIS2_PLACEMENT_3D('',#63853,#33538,#33539);
#28344=AXIS2_PLACEMENT_3D('',#63856,#33541,#33542);
#28345=AXIS2_PLACEMENT_3D('',#63857,#33543,#33544);
#28346=AXIS2_PLACEMENT_3D('',#63863,#33548,#33549);
#28347=AXIS2_PLACEMENT_3D('',#63864,#33550,#33551);
#28348=AXIS2_PLACEMENT_3D('',#63865,#33552,#33553);
#28349=AXIS2_PLACEMENT_3D('',#63866,#33554,#33555);
#28350=AXIS2_PLACEMENT_3D('',#63867,#33556,#33557);
#28351=AXIS2_PLACEMENT_3D('',#63869,#33558,#33559);
#28352=AXIS2_PLACEMENT_3D('',#63870,#33560,#33561);
#28353=AXIS2_PLACEMENT_3D('',#63871,#33562,#33563);
#28354=AXIS2_PLACEMENT_3D('',#63873,#33564,#33565);
#28355=AXIS2_PLACEMENT_3D('',#63874,#33566,#33567);
#28356=AXIS2_PLACEMENT_3D('',#63875,#33568,#33569);
#28357=AXIS2_PLACEMENT_3D('',#63876,#33570,#33571);
#28358=AXIS2_PLACEMENT_3D('',#63877,#33572,#33573);
#28359=AXIS2_PLACEMENT_3D('',#63878,#33574,#33575);
#28360=AXIS2_PLACEMENT_3D('',#63879,#33576,#33577);
#28361=AXIS2_PLACEMENT_3D('',#63880,#33578,#33579);
#28362=AXIS2_PLACEMENT_3D('',#63881,#33580,#33581);
#28363=AXIS2_PLACEMENT_3D('',#63882,#33582,#33583);
#28364=AXIS2_PLACEMENT_3D('',#63883,#33584,#33585);
#28365=AXIS2_PLACEMENT_3D('',#63884,#33586,#33587);
#28366=AXIS2_PLACEMENT_3D('',#63885,#33588,#33589);
#28367=AXIS2_PLACEMENT_3D('',#63886,#33590,#33591);
#28368=AXIS2_PLACEMENT_3D('',#63887,#33592,#33593);
#28369=AXIS2_PLACEMENT_3D('',#63888,#33594,#33595);
#28370=AXIS2_PLACEMENT_3D('',#63889,#33596,#33597);
#28371=AXIS2_PLACEMENT_3D('',#63890,#33598,#33599);
#28372=AXIS2_PLACEMENT_3D('',#63891,#33600,#33601);
#28373=AXIS2_PLACEMENT_3D('',#63892,#33602,#33603);
#28374=AXIS2_PLACEMENT_3D('',#63893,#33604,#33605);
#28375=AXIS2_PLACEMENT_3D('',#63894,#33606,#33607);
#28376=AXIS2_PLACEMENT_3D('',#63895,#33608,#33609);
#28377=AXIS2_PLACEMENT_3D('',#63896,#33610,#33611);
#28378=AXIS2_PLACEMENT_3D('',#63897,#33612,#33613);
#28379=AXIS2_PLACEMENT_3D('',#63898,#33614,#33615);
#28380=AXIS2_PLACEMENT_3D('',#63899,#33616,#33617);
#28381=AXIS2_PLACEMENT_3D('',#63901,#33618,#33619);
#28382=AXIS2_PLACEMENT_3D('',#63904,#33621,#33622);
#28383=AXIS2_PLACEMENT_3D('',#63905,#33623,#33624);
#28384=AXIS2_PLACEMENT_3D('',#63907,#33625,#33626);
#28385=AXIS2_PLACEMENT_3D('',#63908,#33627,#33628);
#28386=AXIS2_PLACEMENT_3D('',#63911,#33630,#33631);
#28387=AXIS2_PLACEMENT_3D('',#63912,#33632,#33633);
#28388=AXIS2_PLACEMENT_3D('',#63915,#33635,#33636);
#28389=AXIS2_PLACEMENT_3D('',#63917,#33637,#33638);
#28390=AXIS2_PLACEMENT_3D('',#63918,#33639,#33640);
#28391=AXIS2_PLACEMENT_3D('',#63920,#33641,#33642);
#28392=AXIS2_PLACEMENT_3D('',#63922,#33644,#33645);
#28393=AXIS2_PLACEMENT_3D('',#63924,#33646,#33647);
#28394=AXIS2_PLACEMENT_3D('',#63927,#33650,#33651);
#28395=AXIS2_PLACEMENT_3D('',#63929,#33652,#33653);
#28396=AXIS2_PLACEMENT_3D('',#63930,#33654,#33655);
#28397=AXIS2_PLACEMENT_3D('',#63931,#33656,#33657);
#28398=AXIS2_PLACEMENT_3D('',#63934,#33658,#33659);
#28399=AXIS2_PLACEMENT_3D('',#63936,#33660,#33661);
#28400=AXIS2_PLACEMENT_3D('',#63951,#33662,#33663);
#28401=AXIS2_PLACEMENT_3D('',#63966,#33664,#33665);
#28402=AXIS2_PLACEMENT_3D('',#63970,#33667,#33668);
#28403=AXIS2_PLACEMENT_3D('',#63986,#33670,#33671);
#28404=AXIS2_PLACEMENT_3D('',#63987,#33672,#33673);
#28405=AXIS2_PLACEMENT_3D('',#63991,#33675,#33676);
#28406=AXIS2_PLACEMENT_3D('',#63995,#33678,#33679);
#28407=AXIS2_PLACEMENT_3D('',#64010,#33680,#33681);
#28408=AXIS2_PLACEMENT_3D('',#64012,#33682,#33683);
#28409=AXIS2_PLACEMENT_3D('',#64013,#33684,#33685);
#28410=AXIS2_PLACEMENT_3D('',#64014,#33686,#33687);
#28411=AXIS2_PLACEMENT_3D('',#64015,#33688,#33689);
#28412=AXIS2_PLACEMENT_3D('',#64021,#33693,#33694);
#28413=AXIS2_PLACEMENT_3D('',#64029,#33698,#33699);
#28414=AXIS2_PLACEMENT_3D('',#64031,#33701,#33702);
#28415=AXIS2_PLACEMENT_3D('',#64033,#33703,#33704);
#28416=AXIS2_PLACEMENT_3D('',#64037,#33707,#33708);
#28417=AXIS2_PLACEMENT_3D('',#64038,#33709,#33710);
#28418=AXIS2_PLACEMENT_3D('',#64041,#33711,#33712);
#28419=AXIS2_PLACEMENT_3D('',#64045,#33714,#33715);
#28420=AXIS2_PLACEMENT_3D('',#64048,#33717,#33718);
#28421=AXIS2_PLACEMENT_3D('',#64049,#33719,#33720);
#28422=AXIS2_PLACEMENT_3D('',#64059,#33726,#33727);
#28423=AXIS2_PLACEMENT_3D('',#64065,#33731,#33732);
#28424=AXIS2_PLACEMENT_3D('',#64069,#33735,#33736);
#28425=AXIS2_PLACEMENT_3D('',#64072,#33737,#33738);
#28426=AXIS2_PLACEMENT_3D('',#64076,#33740,#33741);
#28427=AXIS2_PLACEMENT_3D('',#64078,#33742,#33743);
#28428=AXIS2_PLACEMENT_3D('',#64080,#33745,#33746);
#28429=AXIS2_PLACEMENT_3D('',#64086,#33750,#33751);
#28430=AXIS2_PLACEMENT_3D('',#64096,#33757,#33758);
#28431=AXIS2_PLACEMENT_3D('',#64098,#33759,#33760);
#28432=AXIS2_PLACEMENT_3D('',#64101,#33762,#33763);
#28433=AXIS2_PLACEMENT_3D('',#64102,#33764,#33765);
#28434=AXIS2_PLACEMENT_3D('',#64104,#33766,#33767);
#28435=AXIS2_PLACEMENT_3D('',#64106,#33768,#33769);
#28436=AXIS2_PLACEMENT_3D('',#64107,#33770,#33771);
#28437=AXIS2_PLACEMENT_3D('',#64108,#33772,#33773);
#28438=AXIS2_PLACEMENT_3D('',#64111,#33775,#33776);
#28439=AXIS2_PLACEMENT_3D('',#64112,#33777,#33778);
#28440=AXIS2_PLACEMENT_3D('',#64114,#33779,#33780);
#28441=AXIS2_PLACEMENT_3D('',#64115,#33781,#33782);
#28442=AXIS2_PLACEMENT_3D('',#64116,#33783,#33784);
#28443=AXIS2_PLACEMENT_3D('',#64121,#33786,#33787);
#28444=AXIS2_PLACEMENT_3D('',#64124,#33789,#33790);
#28445=AXIS2_PLACEMENT_3D('',#64125,#33791,#33792);
#28446=AXIS2_PLACEMENT_3D('',#64128,#33795,#33796);
#28447=AXIS2_PLACEMENT_3D('',#64131,#33798,#33799);
#28448=AXIS2_PLACEMENT_3D('',#64132,#33800,#33801);
#28449=AXIS2_PLACEMENT_3D('',#64137,#33804,#33805);
#28450=AXIS2_PLACEMENT_3D('',#64138,#33806,#33807);
#28451=AXIS2_PLACEMENT_3D('',#64141,#33809,#33810);
#28452=AXIS2_PLACEMENT_3D('',#64142,#33811,#33812);
#28453=AXIS2_PLACEMENT_3D('',#64144,#33813,#33814);
#28454=AXIS2_PLACEMENT_3D('',#64145,#33815,#33816);
#28455=AXIS2_PLACEMENT_3D('',#64146,#33817,#33818);
#28456=AXIS2_PLACEMENT_3D('',#64147,#33819,#33820);
#28457=AXIS2_PLACEMENT_3D('',#64149,#33822,#33823);
#28458=AXIS2_PLACEMENT_3D('',#64154,#33826,#33827);
#28459=AXIS2_PLACEMENT_3D('',#64155,#33828,#33829);
#28460=AXIS2_PLACEMENT_3D('',#64158,#33832,#33833);
#28461=AXIS2_PLACEMENT_3D('',#64161,#33835,#33836);
#28462=AXIS2_PLACEMENT_3D('',#64162,#33837,#33838);
#28463=AXIS2_PLACEMENT_3D('',#64166,#33841,#33842);
#28464=AXIS2_PLACEMENT_3D('',#64170,#33844,#33845);
#28465=AXIS2_PLACEMENT_3D('',#64174,#33847,#33848);
#28466=AXIS2_PLACEMENT_3D('',#64178,#33850,#33851);
#28467=AXIS2_PLACEMENT_3D('',#64181,#33853,#33854);
#28468=AXIS2_PLACEMENT_3D('',#64183,#33855,#33856);
#28469=AXIS2_PLACEMENT_3D('',#64185,#33857,#33858);
#28470=AXIS2_PLACEMENT_3D('',#64187,#33859,#33860);
#28471=AXIS2_PLACEMENT_3D('',#64189,#33861,#33862);
#28472=AXIS2_PLACEMENT_3D('',#64190,#33863,#33864);
#28473=AXIS2_PLACEMENT_3D('',#64201,#33870,#33871);
#28474=AXIS2_PLACEMENT_3D('',#64202,#33872,#33873);
#28475=AXIS2_PLACEMENT_3D('',#64204,#33875,#33876);
#28476=AXIS2_PLACEMENT_3D('',#64206,#33878,#33879);
#28477=AXIS2_PLACEMENT_3D('',#64208,#33880,#33881);
#28478=AXIS2_PLACEMENT_3D('',#64210,#33882,#33883);
#28479=AXIS2_PLACEMENT_3D('',#64211,#33884,#33885);
#28480=AXIS2_PLACEMENT_3D('',#64212,#33886,#33887);
#28481=AXIS2_PLACEMENT_3D('',#64214,#33888,#33889);
#28482=AXIS2_PLACEMENT_3D('',#64216,#33891,#33892);
#28483=AXIS2_PLACEMENT_3D('',#64218,#33893,#33894);
#28484=AXIS2_PLACEMENT_3D('',#64219,#33895,#33896);
#28485=AXIS2_PLACEMENT_3D('',#64220,#33897,#33898);
#28486=AXIS2_PLACEMENT_3D('',#64221,#33899,#33900);
#28487=AXIS2_PLACEMENT_3D('',#64223,#33901,#33902);
#28488=AXIS2_PLACEMENT_3D('',#64225,#33903,#33904);
#28489=AXIS2_PLACEMENT_3D('',#64226,#33905,#33906);
#28490=AXIS2_PLACEMENT_3D('',#64227,#33907,#33908);
#28491=AXIS2_PLACEMENT_3D('',#64229,#33909,#33910);
#28492=AXIS2_PLACEMENT_3D('',#64231,#33912,#33913);
#28493=AXIS2_PLACEMENT_3D('',#64233,#33914,#33915);
#28494=AXIS2_PLACEMENT_3D('',#64234,#33916,#33917);
#28495=AXIS2_PLACEMENT_3D('',#64235,#33918,#33919);
#28496=AXIS2_PLACEMENT_3D('',#64236,#33920,#33921);
#28497=AXIS2_PLACEMENT_3D('',#64238,#33922,#33923);
#28498=AXIS2_PLACEMENT_3D('',#64239,#33924,#33925);
#28499=AXIS2_PLACEMENT_3D('',#64240,#33926,#33927);
#28500=AXIS2_PLACEMENT_3D('',#64243,#33929,#33930);
#28501=AXIS2_PLACEMENT_3D('',#64244,#33931,#33932);
#28502=AXIS2_PLACEMENT_3D('',#64246,#33933,#33934);
#28503=AXIS2_PLACEMENT_3D('',#64247,#33935,#33936);
#28504=AXIS2_PLACEMENT_3D('',#64248,#33937,#33938);
#28505=AXIS2_PLACEMENT_3D('',#64251,#33940,#33941);
#28506=AXIS2_PLACEMENT_3D('',#64252,#33942,#33943);
#28507=AXIS2_PLACEMENT_3D('',#64255,#33944,#33945);
#28508=AXIS2_PLACEMENT_3D('',#64257,#33946,#33947);
#28509=AXIS2_PLACEMENT_3D('',#64258,#33948,#33949);
#28510=AXIS2_PLACEMENT_3D('',#64259,#33950,#33951);
#28511=AXIS2_PLACEMENT_3D('',#64262,#33952,#33953);
#28512=AXIS2_PLACEMENT_3D('',#64264,#33954,#33955);
#28513=AXIS2_PLACEMENT_3D('',#64265,#33956,#33957);
#28514=AXIS2_PLACEMENT_3D('',#64266,#33958,#33959);
#28515=AXIS2_PLACEMENT_3D('',#64269,#33962,#33963);
#28516=AXIS2_PLACEMENT_3D('',#64284,#33966,#33967);
#28517=AXIS2_PLACEMENT_3D('',#64301,#33968,#33969);
#28518=AXIS2_PLACEMENT_3D('',#64302,#33970,#33971);
#28519=AXIS2_PLACEMENT_3D('',#64303,#33972,#33973);
#28520=AXIS2_PLACEMENT_3D('',#64320,#33974,#33975);
#28521=AXIS2_PLACEMENT_3D('',#64321,#33976,#33977);
#28522=AXIS2_PLACEMENT_3D('',#64322,#33978,#33979);
#28523=AXIS2_PLACEMENT_3D('',#64337,#33982,#33983);
#28524=AXIS2_PLACEMENT_3D('',#64339,#33984,#33985);
#28525=AXIS2_PLACEMENT_3D('',#64343,#33987,#33988);
#28526=AXIS2_PLACEMENT_3D('',#64345,#33990,#33991);
#28527=AXIS2_PLACEMENT_3D('',#64355,#33997,#33998);
#28528=AXIS2_PLACEMENT_3D('',#64371,#34000,#34001);
#28529=AXIS2_PLACEMENT_3D('',#64373,#34003,#34004);
#28530=AXIS2_PLACEMENT_3D('',#64385,#34006,#34007);
#28531=AXIS2_PLACEMENT_3D('',#64388,#34009,#34010);
#28532=AXIS2_PLACEMENT_3D('',#64390,#34012,#34013);
#28533=AXIS2_PLACEMENT_3D('',#64391,#34014,#34015);
#28534=AXIS2_PLACEMENT_3D('',#64392,#34016,#34017);
#28535=AXIS2_PLACEMENT_3D('',#64394,#34018,#34019);
#28536=AXIS2_PLACEMENT_3D('',#64398,#34021,#34022);
#28537=AXIS2_PLACEMENT_3D('',#64409,#34024,#34025);
#28538=AXIS2_PLACEMENT_3D('',#64420,#34027,#34028);
#28539=AXIS2_PLACEMENT_3D('',#64422,#34030,#34031);
#28540=AXIS2_PLACEMENT_3D('',#64424,#34032,#34033);
#28541=AXIS2_PLACEMENT_3D('',#64430,#34037,#34038);
#28542=AXIS2_PLACEMENT_3D('',#64432,#34039,#34040);
#28543=AXIS2_PLACEMENT_3D('',#64433,#34041,#34042);
#28544=AXIS2_PLACEMENT_3D('',#64434,#34043,#34044);
#28545=AXIS2_PLACEMENT_3D('',#64436,#34045,#34046);
#28546=AXIS2_PLACEMENT_3D('',#64440,#34048,#34049);
#28547=AXIS2_PLACEMENT_3D('',#64444,#34051,#34052);
#28548=AXIS2_PLACEMENT_3D('',#64448,#34054,#34055);
#28549=AXIS2_PLACEMENT_3D('',#64452,#34057,#34058);
#28550=AXIS2_PLACEMENT_3D('',#64454,#34060,#34061);
#28551=AXIS2_PLACEMENT_3D('',#64465,#34063,#34064);
#28552=AXIS2_PLACEMENT_3D('',#64467,#34065,#34066);
#28553=AXIS2_PLACEMENT_3D('',#64469,#34068,#34069);
#28554=AXIS2_PLACEMENT_3D('',#64484,#34071,#34072);
#28555=AXIS2_PLACEMENT_3D('',#64486,#34074,#34075);
#28556=AXIS2_PLACEMENT_3D('',#64487,#34076,#34077);
#28557=AXIS2_PLACEMENT_3D('',#64488,#34078,#34079);
#28558=AXIS2_PLACEMENT_3D('',#64490,#34080,#34081);
#28559=AXIS2_PLACEMENT_3D('',#64491,#34082,#34083);
#28560=AXIS2_PLACEMENT_3D('',#64492,#34084,#34085);
#28561=AXIS2_PLACEMENT_3D('',#64494,#34086,#34087);
#28562=AXIS2_PLACEMENT_3D('',#64500,#34091,#34092);
#28563=AXIS2_PLACEMENT_3D('',#64504,#34094,#34095);
#28564=AXIS2_PLACEMENT_3D('',#64515,#34097,#34098);
#28565=AXIS2_PLACEMENT_3D('',#64526,#34100,#34101);
#28566=AXIS2_PLACEMENT_3D('',#64528,#34103,#34104);
#28567=AXIS2_PLACEMENT_3D('',#64552,#34106,#34107);
#28568=AXIS2_PLACEMENT_3D('',#64572,#34111,#34112);
#28569=AXIS2_PLACEMENT_3D('',#64574,#34113,#34114);
#28570=AXIS2_PLACEMENT_3D('',#64576,#34115,#34116);
#28571=AXIS2_PLACEMENT_3D('',#64578,#34117,#34118);
#28572=AXIS2_PLACEMENT_3D('',#64579,#34119,#34120);
#28573=AXIS2_PLACEMENT_3D('',#64580,#34121,#34122);
#28574=AXIS2_PLACEMENT_3D('',#64583,#34123,#34124);
#28575=AXIS2_PLACEMENT_3D('',#64599,#34133,#34134);
#28576=AXIS2_PLACEMENT_3D('',#64601,#34135,#34136);
#28577=AXIS2_PLACEMENT_3D('',#64603,#34137,#34138);
#28578=AXIS2_PLACEMENT_3D('',#64604,#34139,#34140);
#28579=AXIS2_PLACEMENT_3D('',#64606,#34141,#34142);
#28580=AXIS2_PLACEMENT_3D('',#64608,#34144,#34145);
#28581=AXIS2_PLACEMENT_3D('',#64610,#34146,#34147);
#28582=AXIS2_PLACEMENT_3D('',#64612,#34148,#34149);
#28583=AXIS2_PLACEMENT_3D('',#64613,#34150,#34151);
#28584=AXIS2_PLACEMENT_3D('',#64614,#34152,#34153);
#28585=AXIS2_PLACEMENT_3D('',#64616,#34154,#34155);
#28586=AXIS2_PLACEMENT_3D('',#64618,#34157,#34158);
#28587=AXIS2_PLACEMENT_3D('',#64620,#34159,#34160);
#28588=AXIS2_PLACEMENT_3D('',#64622,#34161,#34162);
#28589=AXIS2_PLACEMENT_3D('',#64623,#34163,#34164);
#28590=AXIS2_PLACEMENT_3D('',#64624,#34165,#34166);
#28591=AXIS2_PLACEMENT_3D('',#64626,#34167,#34168);
#28592=AXIS2_PLACEMENT_3D('',#64628,#34170,#34171);
#28593=AXIS2_PLACEMENT_3D('',#64640,#34172,#34173);
#28594=AXIS2_PLACEMENT_3D('',#64642,#34174,#34175);
#28595=AXIS2_PLACEMENT_3D('',#64643,#34176,#34177);
#28596=AXIS2_PLACEMENT_3D('',#64644,#34178,#34179);
#28597=AXIS2_PLACEMENT_3D('',#64667,#34181,#34182);
#28598=AXIS2_PLACEMENT_3D('',#64671,#34184,#34185);
#28599=AXIS2_PLACEMENT_3D('',#64692,#34187,#34188);
#28600=AXIS2_PLACEMENT_3D('',#64694,#34189,#34190);
#28601=AXIS2_PLACEMENT_3D('',#64696,#34192,#34193);
#28602=AXIS2_PLACEMENT_3D('',#64728,#34194,#34195);
#28603=AXIS2_PLACEMENT_3D('',#64731,#34197,#34198);
#28604=AXIS2_PLACEMENT_3D('',#64732,#34199,#34200);
#28605=AXIS2_PLACEMENT_3D('',#64748,#34209,#34210);
#28606=AXIS2_PLACEMENT_3D('',#64750,#34211,#34212);
#28607=AXIS2_PLACEMENT_3D('',#64752,#34213,#34214);
#28608=AXIS2_PLACEMENT_3D('',#64754,#34215,#34216);
#28609=AXIS2_PLACEMENT_3D('',#64755,#34217,#34218);
#28610=AXIS2_PLACEMENT_3D('',#64757,#34219,#34220);
#28611=AXIS2_PLACEMENT_3D('',#64758,#34221,#34222);
#28612=AXIS2_PLACEMENT_3D('',#64759,#34223,#34224);
#28613=AXIS2_PLACEMENT_3D('',#64763,#34226,#34227);
#28614=AXIS2_PLACEMENT_3D('',#64764,#34228,#34229);
#28615=AXIS2_PLACEMENT_3D('',#64765,#34230,#34231);
#28616=AXIS2_PLACEMENT_3D('',#64783,#34232,#34233);
#28617=AXIS2_PLACEMENT_3D('',#64799,#34234,#34235);
#28618=AXIS2_PLACEMENT_3D('',#64800,#34236,#34237);
#28619=AXIS2_PLACEMENT_3D('',#64804,#34239,#34240);
#28620=AXIS2_PLACEMENT_3D('',#64806,#34242,#34243);
#28621=AXIS2_PLACEMENT_3D('',#64812,#34247,#34248);
#28622=AXIS2_PLACEMENT_3D('',#64829,#34249,#34250);
#28623=AXIS2_PLACEMENT_3D('',#64844,#34251,#34252);
#28624=AXIS2_PLACEMENT_3D('',#64848,#34254,#34255);
#28625=AXIS2_PLACEMENT_3D('',#64850,#34257,#34258);
#28626=AXIS2_PLACEMENT_3D('',#64854,#34261,#34262);
#28627=AXIS2_PLACEMENT_3D('',#64856,#34263,#34264);
#28628=AXIS2_PLACEMENT_3D('',#64857,#34265,#34266);
#28629=AXIS2_PLACEMENT_3D('',#64858,#34267,#34268);
#28630=AXIS2_PLACEMENT_3D('',#64859,#34269,#34270);
#28631=AXIS2_PLACEMENT_3D('',#64861,#34271,#34272);
#28632=AXIS2_PLACEMENT_3D('',#64865,#34274,#34275);
#28633=AXIS2_PLACEMENT_3D('',#64869,#34277,#34278);
#28634=AXIS2_PLACEMENT_3D('',#64872,#34280,#34281);
#28635=AXIS2_PLACEMENT_3D('',#64874,#34282,#34283);
#28636=AXIS2_PLACEMENT_3D('',#64876,#34284,#34285);
#28637=AXIS2_PLACEMENT_3D('',#64878,#34286,#34287);
#28638=AXIS2_PLACEMENT_3D('',#64880,#34288,#34289);
#28639=AXIS2_PLACEMENT_3D('',#64900,#34301,#34302);
#28640=AXIS2_PLACEMENT_3D('',#64902,#34303,#34304);
#28641=AXIS2_PLACEMENT_3D('',#64903,#34305,#34306);
#28642=AXIS2_PLACEMENT_3D('',#64904,#34307,#34308);
#28643=AXIS2_PLACEMENT_3D('',#64905,#34309,#34310);
#28644=AXIS2_PLACEMENT_3D('',#64906,#34311,#34312);
#28645=AXIS2_PLACEMENT_3D('',#64907,#34313,#34314);
#28646=AXIS2_PLACEMENT_3D('',#64908,#34315,#34316);
#28647=AXIS2_PLACEMENT_3D('',#64909,#34317,#34318);
#28648=AXIS2_PLACEMENT_3D('',#64910,#34319,#34320);
#28649=AXIS2_PLACEMENT_3D('',#64911,#34321,#34322);
#28650=AXIS2_PLACEMENT_3D('',#64912,#34323,#34324);
#28651=AXIS2_PLACEMENT_3D('',#64913,#34325,#34326);
#28652=AXIS2_PLACEMENT_3D('',#64916,#34327,#34328);
#28653=AXIS2_PLACEMENT_3D('',#64920,#34330,#34331);
#28654=AXIS2_PLACEMENT_3D('',#64940,#34335,#34336);
#28655=AXIS2_PLACEMENT_3D('',#64941,#34337,#34338);
#28656=AXIS2_PLACEMENT_3D('',#64943,#34340,#34341);
#28657=AXIS2_PLACEMENT_3D('',#64949,#34345,#34346);
#28658=AXIS2_PLACEMENT_3D('',#64954,#34347,#34348);
#28659=AXIS2_PLACEMENT_3D('',#64955,#34349,#34350);
#28660=AXIS2_PLACEMENT_3D('',#64970,#34357,#34358);
#28661=AXIS2_PLACEMENT_3D('',#64972,#34360,#34361);
#28662=AXIS2_PLACEMENT_3D('',#64973,#34362,#34363);
#28663=AXIS2_PLACEMENT_3D('',#64974,#34364,#34365);
#28664=AXIS2_PLACEMENT_3D('',#64977,#34367,#34368);
#28665=AXIS2_PLACEMENT_3D('',#64978,#34369,#34370);
#28666=AXIS2_PLACEMENT_3D('',#64979,#34371,#34372);
#28667=AXIS2_PLACEMENT_3D('',#64980,#34373,#34374);
#28668=AXIS2_PLACEMENT_3D('',#64982,#34375,#34376);
#28669=AXIS2_PLACEMENT_3D('',#64984,#34378,#34379);
#28670=AXIS2_PLACEMENT_3D('',#64985,#34380,#34381);
#28671=AXIS2_PLACEMENT_3D('',#64986,#34382,#34383);
#28672=AXIS2_PLACEMENT_3D('',#64992,#34387,#34388);
#28673=AXIS2_PLACEMENT_3D('',#64994,#34390,#34391);
#28674=AXIS2_PLACEMENT_3D('',#65000,#34393,#34394);
#28675=AXIS2_PLACEMENT_3D('',#65014,#34396,#34397);
#28676=AXIS2_PLACEMENT_3D('',#65015,#34398,#34399);
#28677=AXIS2_PLACEMENT_3D('',#65017,#34400,#34401);
#28678=AXIS2_PLACEMENT_3D('',#65030,#34403,#34404);
#28679=AXIS2_PLACEMENT_3D('',#65034,#34406,#34407);
#28680=AXIS2_PLACEMENT_3D('',#65038,#34409,#34410);
#28681=AXIS2_PLACEMENT_3D('',#65042,#34412,#34413);
#28682=AXIS2_PLACEMENT_3D('',#65044,#34415,#34416);
#28683=AXIS2_PLACEMENT_3D('',#65046,#34417,#34418);
#28684=AXIS2_PLACEMENT_3D('',#65050,#34420,#34421);
#28685=AXIS2_PLACEMENT_3D('',#65101,#34427,#34428);
#28686=AXIS2_PLACEMENT_3D('',#65148,#34444,#34445);
#28687=AXIS2_PLACEMENT_3D('',#65149,#34446,#34447);
#28688=AXIS2_PLACEMENT_3D('',#65150,#34448,#34449);
#28689=AXIS2_PLACEMENT_3D('',#65151,#34450,#34451);
#28690=AXIS2_PLACEMENT_3D('',#65157,#34453,#34454);
#28691=AXIS2_PLACEMENT_3D('',#65159,#34456,#34457);
#28692=AXIS2_PLACEMENT_3D('',#65161,#34458,#34459);
#28693=AXIS2_PLACEMENT_3D('',#65164,#34461,#34462);
#28694=AXIS2_PLACEMENT_3D('',#65165,#34463,#34464);
#28695=AXIS2_PLACEMENT_3D('',#65167,#34465,#34466);
#28696=AXIS2_PLACEMENT_3D('',#65169,#34468,#34469);
#28697=AXIS2_PLACEMENT_3D('',#65173,#34471,#34472);
#28698=AXIS2_PLACEMENT_3D('',#65177,#34474,#34475);
#28699=AXIS2_PLACEMENT_3D('',#65181,#34477,#34478);
#28700=AXIS2_PLACEMENT_3D('',#65184,#34480,#34481);
#28701=AXIS2_PLACEMENT_3D('',#65186,#34482,#34483);
#28702=AXIS2_PLACEMENT_3D('',#65190,#34485,#34486);
#28703=AXIS2_PLACEMENT_3D('',#65193,#34488,#34489);
#28704=AXIS2_PLACEMENT_3D('',#65194,#34490,#34491);
#28705=AXIS2_PLACEMENT_3D('',#65207,#34493,#34494);
#28706=AXIS2_PLACEMENT_3D('',#65208,#34495,#34496);
#28707=AXIS2_PLACEMENT_3D('',#65209,#34497,#34498);
#28708=AXIS2_PLACEMENT_3D('',#65210,#34499,#34500);
#28709=AXIS2_PLACEMENT_3D('',#65213,#34502,#34503);
#28710=AXIS2_PLACEMENT_3D('',#65214,#34504,#34505);
#28711=AXIS2_PLACEMENT_3D('',#65216,#34506,#34507);
#28712=AXIS2_PLACEMENT_3D('',#65218,#34509,#34510);
#28713=AXIS2_PLACEMENT_3D('',#65222,#34512,#34513);
#28714=AXIS2_PLACEMENT_3D('',#65225,#34515,#34516);
#28715=AXIS2_PLACEMENT_3D('',#65226,#34517,#34518);
#28716=AXIS2_PLACEMENT_3D('',#65230,#34520,#34521);
#28717=AXIS2_PLACEMENT_3D('',#65233,#34523,#34524);
#28718=AXIS2_PLACEMENT_3D('',#65234,#34525,#34526);
#28719=AXIS2_PLACEMENT_3D('',#65235,#34527,#34528);
#28720=AXIS2_PLACEMENT_3D('',#65236,#34529,#34530);
#28721=AXIS2_PLACEMENT_3D('',#65237,#34531,#34532);
#28722=AXIS2_PLACEMENT_3D('',#65238,#34533,#34534);
#28723=AXIS2_PLACEMENT_3D('',#65239,#34535,#34536);
#28724=AXIS2_PLACEMENT_3D('',#65240,#34537,#34538);
#28725=AXIS2_PLACEMENT_3D('',#65242,#34539,#34540);
#28726=AXIS2_PLACEMENT_3D('',#65243,#34541,#34542);
#28727=AXIS2_PLACEMENT_3D('',#65244,#34543,#34544);
#28728=AXIS2_PLACEMENT_3D('',#65248,#34547,#34548);
#28729=AXIS2_PLACEMENT_3D('',#65251,#34551,#34552);
#28730=AXIS2_PLACEMENT_3D('',#65253,#34553,#34554);
#28731=AXIS2_PLACEMENT_3D('',#65257,#34555,#34556);
#28732=AXIS2_PLACEMENT_3D('',#65258,#34557,#34558);
#28733=AXIS2_PLACEMENT_3D('',#65260,#34559,#34560);
#28734=AXIS2_PLACEMENT_3D('',#65263,#34562,#34563);
#28735=AXIS2_PLACEMENT_3D('',#65264,#34564,#34565);
#28736=AXIS2_PLACEMENT_3D('',#65265,#34566,#34567);
#28737=AXIS2_PLACEMENT_3D('',#65266,#34568,#34569);
#28738=AXIS2_PLACEMENT_3D('',#65270,#34570,#34571);
#28739=AXIS2_PLACEMENT_3D('',#65274,#34574,#34575);
#28740=AXIS2_PLACEMENT_3D('',#65280,#34579,#34580);
#28741=AXIS2_PLACEMENT_3D('',#65301,#34581,#34582);
#28742=AXIS2_PLACEMENT_3D('',#65320,#34583,#34584);
#28743=AXIS2_PLACEMENT_3D('',#65321,#34585,#34586);
#28744=AXIS2_PLACEMENT_3D('',#65322,#34587,#34588);
#28745=AXIS2_PLACEMENT_3D('',#65328,#34593,#34594);
#28746=AXIS2_PLACEMENT_3D('',#65331,#34597,#34598);
#28747=AXIS2_PLACEMENT_3D('',#65333,#34599,#34600);
#28748=AXIS2_PLACEMENT_3D('',#65336,#34602,#34603);
#28749=AXIS2_PLACEMENT_3D('',#65337,#34604,#34605);
#28750=AXIS2_PLACEMENT_3D('',#65343,#34609,#34610);
#28751=AXIS2_PLACEMENT_3D('',#65349,#34614,#34615);
#28752=AXIS2_PLACEMENT_3D('',#65355,#34619,#34620);
#28753=AXIS2_PLACEMENT_3D('',#65363,#34625,#34626);
#28754=AXIS2_PLACEMENT_3D('',#65372,#34631,#34632);
#28755=AXIS2_PLACEMENT_3D('',#65373,#34633,#34634);
#28756=AXIS2_PLACEMENT_3D('',#65374,#34635,#34636);
#28757=AXIS2_PLACEMENT_3D('',#65375,#34637,#34638);
#28758=AXIS2_PLACEMENT_3D('',#65376,#34639,#34640);
#28759=AXIS2_PLACEMENT_3D('',#65377,#34641,#34642);
#28760=AXIS2_PLACEMENT_3D('',#65388,#34643,#34644);
#28761=AXIS2_PLACEMENT_3D('',#65390,#34646,#34647);
#28762=AXIS2_PLACEMENT_3D('',#65392,#34649,#34650);
#28763=AXIS2_PLACEMENT_3D('',#65393,#34651,#34652);
#28764=AXIS2_PLACEMENT_3D('',#65395,#34654,#34655);
#28765=AXIS2_PLACEMENT_3D('',#65397,#34657,#34658);
#28766=AXIS2_PLACEMENT_3D('',#65401,#34661,#34662);
#28767=AXIS2_PLACEMENT_3D('',#65407,#34666,#34667);
#28768=AXIS2_PLACEMENT_3D('',#65409,#34668,#34669);
#28769=AXIS2_PLACEMENT_3D('',#65426,#34670,#34671);
#28770=AXIS2_PLACEMENT_3D('',#65429,#34672,#34673);
#28771=AXIS2_PLACEMENT_3D('',#65430,#34674,#34675);
#28772=AXIS2_PLACEMENT_3D('',#65447,#34676,#34677);
#28773=AXIS2_PLACEMENT_3D('',#65449,#34679,#34680);
#28774=AXIS2_PLACEMENT_3D('',#65451,#34682,#34683);
#28775=AXIS2_PLACEMENT_3D('',#65459,#34684,#34685);
#28776=AXIS2_PLACEMENT_3D('',#65461,#34687,#34688);
#28777=AXIS2_PLACEMENT_3D('',#65464,#34691,#34692);
#28778=AXIS2_PLACEMENT_3D('',#65470,#34696,#34697);
#28779=AXIS2_PLACEMENT_3D('',#65474,#34700,#34701);
#28780=AXIS2_PLACEMENT_3D('',#65500,#34706,#34707);
#28781=AXIS2_PLACEMENT_3D('',#65526,#34712,#34713);
#28782=AXIS2_PLACEMENT_3D('',#65528,#34715,#34716);
#28783=AXIS2_PLACEMENT_3D('',#65529,#34717,#34718);
#28784=AXIS2_PLACEMENT_3D('',#65535,#34722,#34723);
#28785=AXIS2_PLACEMENT_3D('',#65539,#34726,#34727);
#28786=AXIS2_PLACEMENT_3D('',#65543,#34730,#34731);
#28787=AXIS2_PLACEMENT_3D('',#65547,#34734,#34735);
#28788=AXIS2_PLACEMENT_3D('',#65551,#34738,#34739);
#28789=AXIS2_PLACEMENT_3D('',#65555,#34742,#34743);
#28790=AXIS2_PLACEMENT_3D('',#65559,#34746,#34747);
#28791=AXIS2_PLACEMENT_3D('',#65563,#34750,#34751);
#28792=AXIS2_PLACEMENT_3D('',#65567,#34754,#34755);
#28793=AXIS2_PLACEMENT_3D('',#65569,#34757,#34758);
#28794=AXIS2_PLACEMENT_3D('',#65800,#34777,#34778);
#28795=AXIS2_PLACEMENT_3D('',#65801,#34779,#34780);
#28796=AXIS2_PLACEMENT_3D('',#65807,#34784,#34785);
#28797=AXIS2_PLACEMENT_3D('',#65811,#34788,#34789);
#28798=AXIS2_PLACEMENT_3D('',#65815,#34792,#34793);
#28799=AXIS2_PLACEMENT_3D('',#65817,#34795,#34796);
#28800=AXIS2_PLACEMENT_3D('',#65818,#34797,#34798);
#28801=AXIS2_PLACEMENT_3D('',#65820,#34799,#34800);
#28802=AXIS2_PLACEMENT_3D('',#65821,#34801,#34802);
#28803=AXIS2_PLACEMENT_3D('',#65823,#34804,#34805);
#28804=AXIS2_PLACEMENT_3D('',#65825,#34806,#34807);
#28805=AXIS2_PLACEMENT_3D('',#65826,#34808,#34809);
#28806=AXIS2_PLACEMENT_3D('',#65828,#34811,#34812);
#28807=AXIS2_PLACEMENT_3D('',#65830,#34814,#34815);
#28808=AXIS2_PLACEMENT_3D('',#65832,#34817,#34818);
#28809=AXIS2_PLACEMENT_3D('',#65834,#34820,#34821);
#28810=AXIS2_PLACEMENT_3D('',#65836,#34823,#34824);
#28811=AXIS2_PLACEMENT_3D('',#65837,#34825,#34826);
#28812=AXIS2_PLACEMENT_3D('',#65838,#34827,#34828);
#28813=AXIS2_PLACEMENT_3D('',#65842,#34831,#34832);
#28814=AXIS2_PLACEMENT_3D('',#65844,#34834,#34835);
#28815=AXIS2_PLACEMENT_3D('',#65846,#34837,#34838);
#28816=AXIS2_PLACEMENT_3D('',#65848,#34840,#34841);
#28817=AXIS2_PLACEMENT_3D('',#65852,#34844,#34845);
#28818=AXIS2_PLACEMENT_3D('',#65855,#34848,#34849);
#28819=AXIS2_PLACEMENT_3D('',#65856,#34850,#34851);
#28820=AXIS2_PLACEMENT_3D('',#65857,#34852,#34853);
#28821=AXIS2_PLACEMENT_3D('',#65859,#34854,#34855);
#28822=AXIS2_PLACEMENT_3D('',#65861,#34857,#34858);
#28823=AXIS2_PLACEMENT_3D('',#65863,#34859,#34860);
#28824=AXIS2_PLACEMENT_3D('',#65864,#34861,#34862);
#28825=AXIS2_PLACEMENT_3D('',#65866,#34863,#34864);
#28826=AXIS2_PLACEMENT_3D('',#65868,#34866,#34867);
#28827=AXIS2_PLACEMENT_3D('',#65870,#34868,#34869);
#28828=AXIS2_PLACEMENT_3D('',#65871,#34870,#34871);
#28829=AXIS2_PLACEMENT_3D('',#65874,#34873,#34874);
#28830=AXIS2_PLACEMENT_3D('',#65875,#34875,#34876);
#28831=AXIS2_PLACEMENT_3D('',#65878,#34878,#34879);
#28832=AXIS2_PLACEMENT_3D('',#65879,#34880,#34881);
#28833=AXIS2_PLACEMENT_3D('',#65880,#34882,#34883);
#28834=AXIS2_PLACEMENT_3D('',#65882,#34885,#34886);
#28835=AXIS2_PLACEMENT_3D('',#65885,#34888,#34889);
#28836=AXIS2_PLACEMENT_3D('',#65886,#34890,#34891);
#28837=AXIS2_PLACEMENT_3D('',#65888,#34892,#34893);
#28838=AXIS2_PLACEMENT_3D('',#65890,#34895,#34896);
#28839=AXIS2_PLACEMENT_3D('',#65892,#34898,#34899);
#28840=AXIS2_PLACEMENT_3D('',#65894,#34900,#34901);
#28841=AXIS2_PLACEMENT_3D('',#65896,#34903,#34904);
#28842=AXIS2_PLACEMENT_3D('',#65898,#34906,#34907);
#28843=AXIS2_PLACEMENT_3D('',#65900,#34909,#34910);
#28844=AXIS2_PLACEMENT_3D('',#65902,#34912,#34913);
#28845=AXIS2_PLACEMENT_3D('',#65903,#34914,#34915);
#28846=AXIS2_PLACEMENT_3D('',#65904,#34916,#34917);
#28847=AXIS2_PLACEMENT_3D('',#65906,#34919,#34920);
#28848=AXIS2_PLACEMENT_3D('',#65908,#34922,#34923);
#28849=AXIS2_PLACEMENT_3D('',#65909,#34924,#34925);
#28850=AXIS2_PLACEMENT_3D('',#65911,#34927,#34928);
#28851=AXIS2_PLACEMENT_3D('',#65919,#34929,#34930);
#28852=AXIS2_PLACEMENT_3D('',#65920,#34931,#34932);
#28853=AXIS2_PLACEMENT_3D('',#65921,#34933,#34934);
#28854=AXIS2_PLACEMENT_3D('',#65922,#34935,#34936);
#28855=AXIS2_PLACEMENT_3D('',#65923,#34937,#34938);
#28856=AXIS2_PLACEMENT_3D('',#65925,#34940,#34941);
#28857=AXIS2_PLACEMENT_3D('',#65927,#34943,#34944);
#28858=AXIS2_PLACEMENT_3D('',#65928,#34945,#34946);
#28859=AXIS2_PLACEMENT_3D('',#65929,#34947,#34948);
#28860=AXIS2_PLACEMENT_3D('',#65931,#34950,#34951);
#28861=AXIS2_PLACEMENT_3D('',#65933,#34953,#34954);
#28862=AXIS2_PLACEMENT_3D('',#65934,#34955,#34956);
#28863=AXIS2_PLACEMENT_3D('',#65940,#34960,#34961);
#28864=AXIS2_PLACEMENT_3D('',#65943,#34963,#34964);
#28865=AXIS2_PLACEMENT_3D('',#65944,#34965,#34966);
#28866=AXIS2_PLACEMENT_3D('',#65948,#34969,#34970);
#28867=AXIS2_PLACEMENT_3D('',#65949,#34971,#34972);
#28868=AXIS2_PLACEMENT_3D('',#65950,#34973,#34974);
#28869=AXIS2_PLACEMENT_3D('',#65953,#34976,#34977);
#28870=AXIS2_PLACEMENT_3D('',#65954,#34978,#34979);
#28871=AXIS2_PLACEMENT_3D('',#65958,#34982,#34983);
#28872=AXIS2_PLACEMENT_3D('',#65959,#34984,#34985);
#28873=AXIS2_PLACEMENT_3D('',#65960,#34986,#34987);
#28874=AXIS2_PLACEMENT_3D('',#65963,#34989,#34990);
#28875=AXIS2_PLACEMENT_3D('',#65964,#34991,#34992);
#28876=AXIS2_PLACEMENT_3D('',#65968,#34995,#34996);
#28877=AXIS2_PLACEMENT_3D('',#65971,#34998,#34999);
#28878=AXIS2_PLACEMENT_3D('',#65972,#35000,#35001);
#28879=AXIS2_PLACEMENT_3D('',#65976,#35004,#35005);
#28880=AXIS2_PLACEMENT_3D('',#65977,#35006,#35007);
#28881=AXIS2_PLACEMENT_3D('',#65979,#35009,#35010);
#28882=AXIS2_PLACEMENT_3D('',#65982,#35012,#35013);
#28883=AXIS2_PLACEMENT_3D('',#65983,#35014,#35015);
#28884=AXIS2_PLACEMENT_3D('',#65987,#35018,#35019);
#28885=AXIS2_PLACEMENT_3D('',#65989,#35021,#35022);
#28886=AXIS2_PLACEMENT_3D('',#65990,#35023,#35024);
#28887=AXIS2_PLACEMENT_3D('',#65992,#35026,#35027);
#28888=AXIS2_PLACEMENT_3D('',#65994,#35029,#35030);
#28889=AXIS2_PLACEMENT_3D('',#65995,#35031,#35032);
#28890=AXIS2_PLACEMENT_3D('',#65997,#35034,#35035);
#28891=AXIS2_PLACEMENT_3D('',#65999,#35037,#35038);
#28892=AXIS2_PLACEMENT_3D('',#66000,#35039,#35040);
#28893=AXIS2_PLACEMENT_3D('',#66001,#35041,#35042);
#28894=AXIS2_PLACEMENT_3D('',#66023,#35044,#35045);
#28895=AXIS2_PLACEMENT_3D('',#66034,#35046,#35047);
#28896=AXIS2_PLACEMENT_3D('',#66118,#35049,#35050);
#28897=AXIS2_PLACEMENT_3D('',#66208,#35052,#35053);
#28898=AXIS2_PLACEMENT_3D('',#66298,#35055,#35056);
#28899=AXIS2_PLACEMENT_3D('',#66382,#35058,#35059);
#28900=AXIS2_PLACEMENT_3D('',#66472,#35061,#35062);
#28901=AXIS2_PLACEMENT_3D('',#66559,#35064,#35065);
#28902=AXIS2_PLACEMENT_3D('',#66646,#35067,#35068);
#28903=AXIS2_PLACEMENT_3D('',#66736,#35070,#35071);
#28904=AXIS2_PLACEMENT_3D('',#66820,#35073,#35074);
#28905=AXIS2_PLACEMENT_3D('',#66910,#35076,#35077);
#28906=AXIS2_PLACEMENT_3D('',#67000,#35079,#35080);
#28907=AXIS2_PLACEMENT_3D('',#67084,#35082,#35083);
#28908=AXIS2_PLACEMENT_3D('',#67174,#35085,#35086);
#28909=AXIS2_PLACEMENT_3D('',#67179,#35088,#35089);
#28910=AXIS2_PLACEMENT_3D('',#67257,#35090,#35091);
#28911=AXIS2_PLACEMENT_3D('',#67274,#35093,#35094);
#28912=AXIS2_PLACEMENT_3D('',#67283,#35095,#35096);
#28913=AXIS2_PLACEMENT_3D('',#67321,#35098,#35099);
#28914=AXIS2_PLACEMENT_3D('',#67358,#35101,#35102);
#28915=AXIS2_PLACEMENT_3D('',#67395,#35104,#35105);
#28916=AXIS2_PLACEMENT_3D('',#67433,#35107,#35108);
#28917=AXIS2_PLACEMENT_3D('',#67470,#35110,#35111);
#28918=AXIS2_PLACEMENT_3D('',#67507,#35113,#35114);
#28919=AXIS2_PLACEMENT_3D('',#67545,#35116,#35117);
#28920=AXIS2_PLACEMENT_3D('',#67581,#35119,#35120);
#28921=AXIS2_PLACEMENT_3D('',#67619,#35122,#35123);
#28922=AXIS2_PLACEMENT_3D('',#67656,#35125,#35126);
#28923=AXIS2_PLACEMENT_3D('',#67693,#35128,#35129);
#28924=AXIS2_PLACEMENT_3D('',#67731,#35131,#35132);
#28925=AXIS2_PLACEMENT_3D('',#68263,#35167,#35168);
#28926=AXIS2_PLACEMENT_3D('',#68264,#35169,#35170);
#28927=AXIS2_PLACEMENT_3D('',#68273,#35175,#35176);
#28928=AXIS2_PLACEMENT_3D('',#68279,#35180,#35181);
#28929=AXIS2_PLACEMENT_3D('',#68285,#35185,#35186);
#28930=AXIS2_PLACEMENT_3D('',#68288,#35189,#35190);
#28931=AXIS2_PLACEMENT_3D('',#68784,#35224,#35225);
#28932=AXIS2_PLACEMENT_3D('',#68785,#35226,#35227);
#28933=AXIS2_PLACEMENT_3D('',#68786,#35228,#35229);
#28934=AXIS2_PLACEMENT_3D('',#68787,#35230,#35231);
#28935=AXIS2_PLACEMENT_3D('',#68788,#35232,#35233);
#28936=AXIS2_PLACEMENT_3D('',#68789,#35234,#35235);
#28937=AXIS2_PLACEMENT_3D('',#68864,#35236,#35237);
#28938=AXIS2_PLACEMENT_3D('',#68866,#35238,#35239);
#28939=AXIS2_PLACEMENT_3D('',#69786,#35240,#35241);
#28940=AXIS2_PLACEMENT_3D('',#69788,#35242,#35243);
#28941=AXIS2_PLACEMENT_3D('',#69789,#35244,#35245);
#28942=AXIS2_PLACEMENT_3D('',#69870,#35246,#35247);
#28943=AXIS2_PLACEMENT_3D('',#69871,#35248,#35249);
#28944=AXIS2_PLACEMENT_3D('',#70632,#35250,#35251);
#28945=AXIS2_PLACEMENT_3D('',#70634,#35252,#35253);
#28946=AXIS2_PLACEMENT_3D('',#70635,#35254,#35255);
#28947=AXIS2_PLACEMENT_3D('',#70636,#35256,#35257);
#28948=AXIS2_PLACEMENT_3D('',#70637,#35258,#35259);
#28949=AXIS2_PLACEMENT_3D('',#70650,#35266,#35267);
#28950=AXIS2_PLACEMENT_3D('',#70651,#35268,#35269);
#28951=AXIS2_PLACEMENT_3D('',#70675,#35271,#35272);
#28952=AXIS2_PLACEMENT_3D('',#70683,#35273,#35274);
#28953=AXIS2_PLACEMENT_3D('',#70686,#35277,#35278);
#28954=AXIS2_PLACEMENT_3D('',#70688,#35280,#35281);
#28955=AXIS2_PLACEMENT_3D('',#70690,#35283,#35284);
#28956=AXIS2_PLACEMENT_3D('',#70692,#35286,#35287);
#28957=AXIS2_PLACEMENT_3D('',#70694,#35289,#35290);
#28958=AXIS2_PLACEMENT_3D('',#70695,#35291,#35292);
#28959=AXIS2_PLACEMENT_3D('',#70696,#35293,#35294);
#28960=AXIS2_PLACEMENT_3D('',#70698,#35295,#35296);
#28961=AXIS2_PLACEMENT_3D('',#70699,#35297,#35298);
#28962=AXIS2_PLACEMENT_3D('',#70701,#35300,#35301);
#28963=AXIS2_PLACEMENT_3D('',#70702,#35302,#35303);
#28964=AXIS2_PLACEMENT_3D('',#70703,#35304,#35305);
#28965=AXIS2_PLACEMENT_3D('',#70704,#35306,#35307);
#28966=AXIS2_PLACEMENT_3D('',#70705,#35308,#35309);
#28967=AXIS2_PLACEMENT_3D('',#70706,#35310,#35311);
#28968=AXIS2_PLACEMENT_3D('',#70707,#35312,#35313);
#28969=AXIS2_PLACEMENT_3D('',#70708,#35314,#35315);
#28970=AXIS2_PLACEMENT_3D('',#70709,#35316,#35317);
#28971=AXIS2_PLACEMENT_3D('',#70710,#35318,#35319);
#28972=AXIS2_PLACEMENT_3D('',#70711,#35320,#35321);
#28973=AXIS2_PLACEMENT_3D('',#70712,#35322,#35323);
#28974=AXIS2_PLACEMENT_3D('',#70713,#35324,#35325);
#28975=AXIS2_PLACEMENT_3D('',#70714,#35326,#35327);
#28976=AXIS2_PLACEMENT_3D('',#70715,#35328,#35329);
#28977=AXIS2_PLACEMENT_3D('',#70716,#35330,#35331);
#28978=AXIS2_PLACEMENT_3D('',#70717,#35332,#35333);
#28979=AXIS2_PLACEMENT_3D('',#70718,#35334,#35335);
#28980=AXIS2_PLACEMENT_3D('',#70719,#35336,#35337);
#28981=AXIS2_PLACEMENT_3D('',#70720,#35338,#35339);
#28982=AXIS2_PLACEMENT_3D('',#70721,#35340,#35341);
#28983=AXIS2_PLACEMENT_3D('',#70722,#35342,#35343);
#28984=AXIS2_PLACEMENT_3D('',#70723,#35344,#35345);
#28985=DIRECTION('axis',(0.,0.,1.));
#28986=DIRECTION('refdir',(1.,0.,0.));
#28987=DIRECTION('axis',(0.,0.,1.));
#28988=DIRECTION('refdir',(1.,0.,0.));
#28989=DIRECTION('center_axis',(0.,-1.,0.));
#28990=DIRECTION('ref_axis',(-1.,0.,0.));
#28991=DIRECTION('center_axis',(0.,1.,0.));
#28992=DIRECTION('ref_axis',(-1.,0.,0.));
#28993=DIRECTION('center_axis',(0.,1.,0.));
#28994=DIRECTION('ref_axis',(-1.,0.,0.));
#28995=DIRECTION('',(-0.707106781186545,0.70710678118655,-8.65956056235491E-17));
#28996=DIRECTION('center_axis',(0.,-1.,0.));
#28997=DIRECTION('ref_axis',(-1.,0.,0.));
#28998=DIRECTION('center_axis',(0.,1.,0.));
#28999=DIRECTION('ref_axis',(0.,0.,1.));
#29000=DIRECTION('center_axis',(0.,-1.,0.));
#29001=DIRECTION('ref_axis',(1.,0.,0.));
#29002=DIRECTION('',(0.973234235146997,0.,0.229815411880577));
#29003=DIRECTION('center_axis',(0.,-1.,0.));
#29004=DIRECTION('ref_axis',(-0.966435998091082,0.,-0.256907496180421));
#29005=DIRECTION('',(-0.993142529173694,0.,-0.116909865907365));
#29006=DIRECTION('center_axis',(0.,-1.,0.));
#29007=DIRECTION('ref_axis',(1.,0.,0.));
#29008=DIRECTION('',(0.835939528954007,0.,0.548821559281478));
#29009=DIRECTION('center_axis',(0.,-1.,0.));
#29010=DIRECTION('ref_axis',(-0.820285237202974,0.,-0.571954656967543));
#29011=DIRECTION('',(-0.89326317695935,0.,-0.449534088461031));
#29012=DIRECTION('center_axis',(0.,-1.,0.));
#29013=DIRECTION('ref_axis',(1.,0.,0.));
#29014=DIRECTION('',(0.597818178415661,0.,0.801631726889462));
#29015=DIRECTION('center_axis',(0.,-1.,0.));
#29016=DIRECTION('ref_axis',(-0.575195970587437,0.,-0.818015644972623));
#29017=DIRECTION('',(-0.685643102443273,0.,-0.727937865529719));
#29018=DIRECTION('center_axis',(0.,-1.,0.));
#29019=DIRECTION('ref_axis',(1.,0.,0.));
#29020=DIRECTION('',(0.287591132703732,0.,0.957753277410307));
#29021=DIRECTION('center_axis',(0.,-1.,0.));
#29022=DIRECTION('ref_axis',(-0.260729580930624,0.,-0.965411873568862));
#29023=DIRECTION('',(-0.395324350758037,0.,-0.918541592796829));
#29024=DIRECTION('center_axis',(0.,-1.,0.));
#29025=DIRECTION('ref_axis',(1.,0.,0.));
#29026=DIRECTION('',(-0.0573236480053483,0.,0.998355647742506));
#29027=DIRECTION('center_axis',(0.,-1.,0.));
#29028=DIRECTION('ref_axis',(0.0851846441452059,0.,-0.996365182250893));
#29029=DIRECTION('',(-0.0573236480053483,0.,-0.998355647742506));
#29030=DIRECTION('center_axis',(0.,-1.,0.));
#29031=DIRECTION('ref_axis',(1.,0.,0.));
#29032=DIRECTION('',(-0.395324350758034,0.,0.918541592796831));
#29033=DIRECTION('center_axis',(0.,-1.,0.));
#29034=DIRECTION('ref_axis',(0.420824343945678,0.,-0.907142145169482));
#29035=DIRECTION('',(0.287591132703732,0.,-0.957753277410307));
#29036=DIRECTION('center_axis',(0.,-1.,0.));
#29037=DIRECTION('ref_axis',(1.,0.,0.));
#29038=DIRECTION('',(-0.68564310244327,0.,0.727937865529722));
#29039=DIRECTION('center_axis',(0.,-1.,0.));
#29040=DIRECTION('ref_axis',(0.705706417160429,0.,-0.708504377388447));
#29041=DIRECTION('',(0.597818178415657,0.,-0.801631726889465));
#29042=DIRECTION('center_axis',(0.,-1.,0.));
#29043=DIRECTION('ref_axis',(1.,0.,0.));
#29044=DIRECTION('',(-0.893263176959351,0.,0.449534088461028));
#29045=DIRECTION('center_axis',(0.,-1.,0.));
#29046=DIRECTION('ref_axis',(0.9054698813482,0.,-0.424410525283336));
#29047=DIRECTION('',(0.835939528953991,0.,-0.548821559281502));
#29048=DIRECTION('center_axis',(0.,-1.,0.));
#29049=DIRECTION('ref_axis',(1.,0.,0.));
#29050=DIRECTION('',(-0.993142529173694,0.,0.116909865907364));
#29051=DIRECTION('center_axis',(0.,-1.,0.));
#29052=DIRECTION('ref_axis',(0.996020314533121,0.,-0.0891265001968739));
#29053=DIRECTION('',(0.973234235146997,0.,-0.229815411880577));
#29054=DIRECTION('center_axis',(0.,-1.,0.));
#29055=DIRECTION('ref_axis',(1.,0.,0.));
#29056=DIRECTION('',(-0.973234235146997,0.,-0.229815411880577));
#29057=DIRECTION('center_axis',(0.,-1.,0.));
#29058=DIRECTION('ref_axis',(0.966435998091084,0.,0.256907496180414));
#29059=DIRECTION('',(0.993142529173694,0.,0.116909865907365));
#29060=DIRECTION('center_axis',(0.,-1.,0.));
#29061=DIRECTION('ref_axis',(1.,0.,0.));
#29062=DIRECTION('',(-0.835939528954005,0.,-0.548821559281481));
#29063=DIRECTION('center_axis',(0.,-1.,0.));
#29064=DIRECTION('ref_axis',(0.820285237202979,0.,0.571954656967538));
#29065=DIRECTION('',(0.89326317695935,0.,0.44953408846103));
#29066=DIRECTION('center_axis',(0.,-1.,0.));
#29067=DIRECTION('ref_axis',(1.,0.,0.));
#29068=DIRECTION('',(-0.597818178415659,0.,-0.801631726889463));
#29069=DIRECTION('center_axis',(0.,-1.,0.));
#29070=DIRECTION('ref_axis',(0.575195970587441,0.,0.818015644972621));
#29071=DIRECTION('',(0.685643102443272,0.,0.72793786552972));
#29072=DIRECTION('center_axis',(0.,-1.,0.));
#29073=DIRECTION('ref_axis',(1.,0.,0.));
#29074=DIRECTION('',(-0.287591132703736,0.,-0.957753277410306));
#29075=DIRECTION('center_axis',(0.,-1.,0.));
#29076=DIRECTION('ref_axis',(0.260729580930626,0.,0.965411873568862));
#29077=DIRECTION('',(0.395324350758034,0.,0.918541592796831));
#29078=DIRECTION('center_axis',(0.,-1.,0.));
#29079=DIRECTION('ref_axis',(1.,0.,0.));
#29080=DIRECTION('',(0.0573236480053483,0.,-0.998355647742506));
#29081=DIRECTION('center_axis',(0.,-1.,0.));
#29082=DIRECTION('ref_axis',(-0.0851846441452059,0.,0.996365182250893));
#29083=DIRECTION('',(0.0573236480053525,0.,0.998355647742506));
#29084=DIRECTION('center_axis',(0.,-1.,0.));
#29085=DIRECTION('ref_axis',(1.,0.,0.));
#29086=DIRECTION('',(0.395324350758046,0.,-0.918541592796826));
#29087=DIRECTION('center_axis',(0.,-1.,0.));
#29088=DIRECTION('ref_axis',(-0.420824343945662,0.,0.907142145169489));
#29089=DIRECTION('',(-0.287591132703732,0.,0.957753277410307));
#29090=DIRECTION('center_axis',(0.,-1.,0.));
#29091=DIRECTION('ref_axis',(1.,0.,0.));
#29092=DIRECTION('',(0.685643102443271,0.,-0.727937865529721));
#29093=DIRECTION('center_axis',(0.,-1.,0.));
#29094=DIRECTION('ref_axis',(-0.705706417160429,0.,0.708504377388447));
#29095=DIRECTION('',(-0.597818178415657,0.,0.801631726889465));
#29096=DIRECTION('center_axis',(0.,-1.,0.));
#29097=DIRECTION('ref_axis',(1.,0.,0.));
#29098=DIRECTION('',(0.89326317695935,0.,-0.44953408846103));
#29099=DIRECTION('center_axis',(0.,-1.,0.));
#29100=DIRECTION('ref_axis',(-0.905469881348196,0.,0.424410525283343));
#29101=DIRECTION('',(-0.835939528953991,0.,0.548821559281503));
#29102=DIRECTION('center_axis',(0.,-1.,0.));
#29103=DIRECTION('ref_axis',(1.,0.,0.));
#29104=DIRECTION('',(0.993142529173694,0.,-0.116909865907365));
#29105=DIRECTION('center_axis',(0.,-1.,0.));
#29106=DIRECTION('ref_axis',(-0.996020314533121,0.,0.0891265001968672));
#29107=DIRECTION('',(-0.973234235146997,0.,0.229815411880577));
#29108=DIRECTION('center_axis',(0.,-1.,0.));
#29109=DIRECTION('ref_axis',(1.,0.,0.));
#29110=DIRECTION('center_axis',(0.,-1.,0.));
#29111=DIRECTION('ref_axis',(1.,0.,0.));
#29112=DIRECTION('',(0.,1.,0.));
#29113=DIRECTION('center_axis',(0.,1.,0.));
#29114=DIRECTION('ref_axis',(-1.,0.,0.));
#29115=DIRECTION('center_axis',(0.,1.,0.));
#29116=DIRECTION('ref_axis',(-1.,0.,0.));
#29117=DIRECTION('',(0.707106781186548,0.707106781186548,8.65956056235493E-17));
#29118=DIRECTION('center_axis',(0.,-1.,0.));
#29119=DIRECTION('ref_axis',(-1.,0.,0.));
#29120=DIRECTION('center_axis',(0.,-1.,0.));
#29121=DIRECTION('ref_axis',(-1.,0.,0.));
#29122=DIRECTION('center_axis',(0.,-1.,0.));
#29123=DIRECTION('ref_axis',(0.,0.,-1.));
#29124=DIRECTION('',(0.973234235146997,0.,-0.229815411880577));
#29125=DIRECTION('center_axis',(0.,1.,0.));
#29126=DIRECTION('ref_axis',(-0.996020314533121,0.,0.0891265001968672));
#29127=DIRECTION('',(-0.993142529173694,0.,0.116909865907365));
#29128=DIRECTION('center_axis',(0.,1.,0.));
#29129=DIRECTION('ref_axis',(1.,0.,0.));
#29130=DIRECTION('',(0.835939528953991,0.,-0.548821559281503));
#29131=DIRECTION('center_axis',(0.,1.,0.));
#29132=DIRECTION('ref_axis',(-0.905469881348196,0.,0.424410525283343));
#29133=DIRECTION('',(-0.89326317695935,0.,0.44953408846103));
#29134=DIRECTION('center_axis',(0.,1.,0.));
#29135=DIRECTION('ref_axis',(1.,0.,0.));
#29136=DIRECTION('',(0.597818178415657,0.,-0.801631726889465));
#29137=DIRECTION('center_axis',(0.,1.,0.));
#29138=DIRECTION('ref_axis',(-0.705706417160429,0.,0.708504377388447));
#29139=DIRECTION('',(-0.685643102443271,0.,0.727937865529721));
#29140=DIRECTION('center_axis',(0.,1.,0.));
#29141=DIRECTION('ref_axis',(1.,0.,0.));
#29142=DIRECTION('',(0.287591132703732,0.,-0.957753277410307));
#29143=DIRECTION('center_axis',(0.,1.,0.));
#29144=DIRECTION('ref_axis',(-0.420824343945662,0.,0.907142145169489));
#29145=DIRECTION('',(-0.395324350758046,0.,0.918541592796826));
#29146=DIRECTION('center_axis',(0.,1.,0.));
#29147=DIRECTION('ref_axis',(1.,0.,0.));
#29148=DIRECTION('',(-0.0573236480053525,0.,-0.998355647742506));
#29149=DIRECTION('center_axis',(0.,1.,0.));
#29150=DIRECTION('ref_axis',(-0.0851846441452059,0.,0.996365182250893));
#29151=DIRECTION('',(-0.0573236480053483,0.,0.998355647742506));
#29152=DIRECTION('center_axis',(0.,1.,0.));
#29153=DIRECTION('ref_axis',(1.,0.,0.));
#29154=DIRECTION('',(-0.395324350758034,0.,-0.918541592796831));
#29155=DIRECTION('center_axis',(0.,1.,0.));
#29156=DIRECTION('ref_axis',(0.260729580930626,0.,0.965411873568862));
#29157=DIRECTION('',(0.287591132703736,0.,0.957753277410306));
#29158=DIRECTION('center_axis',(0.,1.,0.));
#29159=DIRECTION('ref_axis',(1.,0.,0.));
#29160=DIRECTION('',(-0.685643102443272,0.,-0.72793786552972));
#29161=DIRECTION('center_axis',(0.,1.,0.));
#29162=DIRECTION('ref_axis',(0.575195970587441,0.,0.818015644972621));
#29163=DIRECTION('',(0.597818178415659,0.,0.801631726889463));
#29164=DIRECTION('center_axis',(0.,1.,0.));
#29165=DIRECTION('ref_axis',(1.,0.,0.));
#29166=DIRECTION('',(-0.89326317695935,0.,-0.44953408846103));
#29167=DIRECTION('center_axis',(0.,1.,0.));
#29168=DIRECTION('ref_axis',(0.820285237202979,0.,0.571954656967538));
#29169=DIRECTION('',(0.835939528954005,0.,0.548821559281481));
#29170=DIRECTION('center_axis',(0.,1.,0.));
#29171=DIRECTION('ref_axis',(1.,0.,0.));
#29172=DIRECTION('',(-0.993142529173694,0.,-0.116909865907365));
#29173=DIRECTION('center_axis',(0.,1.,0.));
#29174=DIRECTION('ref_axis',(0.966435998091084,0.,0.256907496180414));
#29175=DIRECTION('',(0.973234235146997,0.,0.229815411880577));
#29176=DIRECTION('center_axis',(0.,1.,0.));
#29177=DIRECTION('ref_axis',(1.,0.,0.));
#29178=DIRECTION('',(-0.973234235146997,0.,0.229815411880577));
#29179=DIRECTION('center_axis',(0.,1.,0.));
#29180=DIRECTION('ref_axis',(0.996020314533121,0.,-0.0891265001968739));
#29181=DIRECTION('',(0.993142529173694,0.,-0.116909865907364));
#29182=DIRECTION('center_axis',(0.,1.,0.));
#29183=DIRECTION('ref_axis',(1.,0.,0.));
#29184=DIRECTION('',(-0.835939528953991,0.,0.548821559281502));
#29185=DIRECTION('center_axis',(0.,1.,0.));
#29186=DIRECTION('ref_axis',(0.9054698813482,0.,-0.424410525283336));
#29187=DIRECTION('',(0.893263176959351,0.,-0.449534088461028));
#29188=DIRECTION('center_axis',(0.,1.,0.));
#29189=DIRECTION('ref_axis',(1.,0.,0.));
#29190=DIRECTION('',(-0.597818178415657,0.,0.801631726889465));
#29191=DIRECTION('center_axis',(0.,1.,0.));
#29192=DIRECTION('ref_axis',(0.705706417160429,0.,-0.708504377388447));
#29193=DIRECTION('',(0.68564310244327,0.,-0.727937865529722));
#29194=DIRECTION('center_axis',(0.,1.,0.));
#29195=DIRECTION('ref_axis',(1.,0.,0.));
#29196=DIRECTION('',(-0.287591132703732,0.,0.957753277410307));
#29197=DIRECTION('center_axis',(0.,1.,0.));
#29198=DIRECTION('ref_axis',(0.420824343945678,0.,-0.907142145169482));
#29199=DIRECTION('',(0.395324350758034,0.,-0.918541592796831));
#29200=DIRECTION('center_axis',(0.,1.,0.));
#29201=DIRECTION('ref_axis',(1.,0.,0.));
#29202=DIRECTION('',(0.0573236480053483,0.,0.998355647742506));
#29203=DIRECTION('center_axis',(0.,1.,0.));
#29204=DIRECTION('ref_axis',(0.0851846441452059,0.,-0.996365182250893));
#29205=DIRECTION('',(0.0573236480053483,0.,-0.998355647742506));
#29206=DIRECTION('center_axis',(0.,1.,0.));
#29207=DIRECTION('ref_axis',(1.,0.,0.));
#29208=DIRECTION('',(0.395324350758037,0.,0.918541592796829));
#29209=DIRECTION('center_axis',(0.,1.,0.));
#29210=DIRECTION('ref_axis',(-0.260729580930624,0.,-0.965411873568862));
#29211=DIRECTION('',(-0.287591132703732,0.,-0.957753277410307));
#29212=DIRECTION('center_axis',(0.,1.,0.));
#29213=DIRECTION('ref_axis',(1.,0.,0.));
#29214=DIRECTION('',(0.685643102443273,0.,0.727937865529719));
#29215=DIRECTION('center_axis',(0.,1.,0.));
#29216=DIRECTION('ref_axis',(-0.575195970587437,0.,-0.818015644972623));
#29217=DIRECTION('',(-0.597818178415661,0.,-0.801631726889462));
#29218=DIRECTION('center_axis',(0.,1.,0.));
#29219=DIRECTION('ref_axis',(1.,0.,0.));
#29220=DIRECTION('',(0.89326317695935,0.,0.449534088461031));
#29221=DIRECTION('center_axis',(0.,1.,0.));
#29222=DIRECTION('ref_axis',(-0.820285237202974,0.,-0.571954656967543));
#29223=DIRECTION('',(-0.835939528954007,0.,-0.548821559281478));
#29224=DIRECTION('center_axis',(0.,1.,0.));
#29225=DIRECTION('ref_axis',(1.,0.,0.));
#29226=DIRECTION('',(0.993142529173694,0.,0.116909865907365));
#29227=DIRECTION('center_axis',(0.,1.,0.));
#29228=DIRECTION('ref_axis',(-0.966435998091082,0.,-0.256907496180421));
#29229=DIRECTION('',(-0.973234235146997,0.,-0.229815411880577));
#29230=DIRECTION('center_axis',(0.,1.,0.));
#29231=DIRECTION('ref_axis',(1.,0.,0.));
#29232=DIRECTION('center_axis',(0.,-1.,0.));
#29233=DIRECTION('ref_axis',(1.,0.,0.));
#29234=DIRECTION('',(0.,1.,0.));
#29235=DIRECTION('center_axis',(0.,-1.,0.));
#29236=DIRECTION('ref_axis',(1.,0.,0.));
#29237=DIRECTION('center_axis',(0.,1.,0.));
#29238=DIRECTION('ref_axis',(0.,0.,1.));
#29239=DIRECTION('center_axis',(0.,-1.,0.));
#29240=DIRECTION('ref_axis',(1.,0.,0.));
#29241=DIRECTION('center_axis',(0.,-1.,0.));
#29242=DIRECTION('ref_axis',(1.,0.,0.));
#29243=DIRECTION('center_axis',(0.,-1.,0.));
#29244=DIRECTION('ref_axis',(1.,0.,0.));
#29245=DIRECTION('',(0.707106781186541,0.707106781186554,8.65956056235486E-17));
#29246=DIRECTION('center_axis',(0.,-1.,0.));
#29247=DIRECTION('ref_axis',(1.,0.,0.));
#29248=DIRECTION('center_axis',(0.,-1.,0.));
#29249=DIRECTION('ref_axis',(1.,0.,0.));
#29250=DIRECTION('',(0.,1.,0.));
#29251=DIRECTION('center_axis',(0.,1.,0.));
#29252=DIRECTION('ref_axis',(0.,0.,1.));
#29253=DIRECTION('center_axis',(0.,-1.,0.));
#29254=DIRECTION('ref_axis',(1.,0.,0.));
#29255=DIRECTION('center_axis',(0.,-1.,0.));
#29256=DIRECTION('ref_axis',(1.,0.,0.));
#29257=DIRECTION('',(0.707106781186543,0.707106781186552,8.65956056235488E-17));
#29258=DIRECTION('center_axis',(0.,1.,0.));
#29259=DIRECTION('ref_axis',(1.,0.,0.));
#29260=DIRECTION('center_axis',(0.,-1.,0.));
#29261=DIRECTION('ref_axis',(1.,0.,0.));
#29262=DIRECTION('',(-0.707106781186543,0.707106781186552,-8.65956056235488E-17));
#29263=DIRECTION('center_axis',(0.,-1.,0.));
#29264=DIRECTION('ref_axis',(0.,0.,-1.));
#29265=DIRECTION('center_axis',(0.,-1.,0.));
#29266=DIRECTION('ref_axis',(1.,0.,0.));
#29267=DIRECTION('center_axis',(0.,-1.,0.));
#29268=DIRECTION('ref_axis',(1.,0.,0.));
#29269=DIRECTION('center_axis',(0.,-1.,0.));
#29270=DIRECTION('ref_axis',(1.,0.,0.));
#29271=DIRECTION('',(0.,1.,0.));
#29272=DIRECTION('center_axis',(0.,1.,0.));
#29273=DIRECTION('ref_axis',(1.,0.,0.));
#29274=DIRECTION('center_axis',(0.,-1.,0.));
#29275=DIRECTION('ref_axis',(1.,0.,0.));
#29276=DIRECTION('',(-0.707106781186541,0.707106781186554,-8.65956056235486E-17));
#29277=DIRECTION('center_axis',(0.,-1.,0.));
#29278=DIRECTION('ref_axis',(0.,0.,-1.));
#29279=DIRECTION('',(0.,1.,0.));
#29280=DIRECTION('center_axis',(0.,1.,0.));
#29281=DIRECTION('ref_axis',(-0.905469881348196,0.,0.424410525283343));
#29282=DIRECTION('',(0.,-1.,0.));
#29283=DIRECTION('',(0.,1.,0.));
#29284=DIRECTION('center_axis',(0.44953408846103,0.,0.89326317695935));
#29285=DIRECTION('ref_axis',(0.89326317695935,0.,-0.44953408846103));
#29286=DIRECTION('',(0.,1.,0.));
#29287=DIRECTION('center_axis',(-0.548821559281503,0.,-0.835939528953991));
#29288=DIRECTION('ref_axis',(-0.835939528953991,0.,0.548821559281503));
#29289=DIRECTION('',(0.,1.,0.));
#29290=DIRECTION('center_axis',(0.,1.,0.));
#29291=DIRECTION('ref_axis',(-0.420824343945662,0.,0.907142145169489));
#29292=DIRECTION('',(0.,-1.,0.));
#29293=DIRECTION('',(0.,1.,0.));
#29294=DIRECTION('center_axis',(0.918541592796826,0.,0.395324350758046));
#29295=DIRECTION('ref_axis',(0.395324350758046,0.,-0.918541592796826));
#29296=DIRECTION('',(0.,1.,0.));
#29297=DIRECTION('center_axis',(-0.957753277410307,0.,-0.287591132703732));
#29298=DIRECTION('ref_axis',(-0.287591132703732,0.,0.957753277410307));
#29299=DIRECTION('',(0.,1.,0.));
#29300=DIRECTION('center_axis',(0.,1.,0.));
#29301=DIRECTION('ref_axis',(0.260729580930626,0.,0.965411873568862));
#29302=DIRECTION('',(0.,-1.,0.));
#29303=DIRECTION('',(0.,1.,0.));
#29304=DIRECTION('center_axis',(0.957753277410306,0.,-0.287591132703736));
#29305=DIRECTION('ref_axis',(-0.287591132703736,0.,-0.957753277410306));
#29306=DIRECTION('',(0.,1.,0.));
#29307=DIRECTION('center_axis',(-0.918541592796831,0.,0.395324350758034));
#29308=DIRECTION('ref_axis',(0.395324350758034,0.,0.918541592796831));
#29309=DIRECTION('',(0.,1.,0.));
#29310=DIRECTION('center_axis',(0.,1.,0.));
#29311=DIRECTION('ref_axis',(0.820285237202979,0.,0.571954656967538));
#29312=DIRECTION('',(0.,-1.,0.));
#29313=DIRECTION('',(0.,1.,0.));
#29314=DIRECTION('center_axis',(0.548821559281481,0.,-0.835939528954005));
#29315=DIRECTION('ref_axis',(-0.835939528954005,0.,-0.548821559281481));
#29316=DIRECTION('',(0.,1.,0.));
#29317=DIRECTION('center_axis',(-0.44953408846103,0.,0.89326317695935));
#29318=DIRECTION('ref_axis',(0.89326317695935,0.,0.44953408846103));
#29319=DIRECTION('',(0.,1.,0.));
#29320=DIRECTION('center_axis',(0.,1.,0.));
#29321=DIRECTION('ref_axis',(-0.966435998091082,0.,-0.256907496180421));
#29322=DIRECTION('',(0.,-1.,0.));
#29323=DIRECTION('',(0.,1.,0.));
#29324=DIRECTION('center_axis',(-0.229815411880577,0.,0.973234235146997));
#29325=DIRECTION('ref_axis',(0.973234235146997,0.,0.229815411880577));
#29326=DIRECTION('',(0.,1.,0.));
#29327=DIRECTION('center_axis',(0.116909865907365,0.,-0.993142529173694));
#29328=DIRECTION('ref_axis',(-0.993142529173694,0.,-0.116909865907365));
#29329=DIRECTION('',(0.,1.,0.));
#29330=DIRECTION('center_axis',(0.,1.,0.));
#29331=DIRECTION('ref_axis',(0.9054698813482,0.,-0.424410525283336));
#29332=DIRECTION('',(0.,-1.,0.));
#29333=DIRECTION('',(0.,1.,0.));
#29334=DIRECTION('center_axis',(-0.449534088461028,0.,-0.893263176959351));
#29335=DIRECTION('ref_axis',(-0.893263176959351,0.,0.449534088461028));
#29336=DIRECTION('',(0.,1.,0.));
#29337=DIRECTION('center_axis',(0.548821559281502,0.,0.835939528953991));
#29338=DIRECTION('ref_axis',(0.835939528953991,0.,-0.548821559281502));
#29339=DIRECTION('',(0.,1.,0.));
#29340=DIRECTION('center_axis',(0.,1.,0.));
#29341=DIRECTION('ref_axis',(0.420824343945678,0.,-0.907142145169482));
#29342=DIRECTION('',(0.,-1.,0.));
#29343=DIRECTION('',(0.,1.,0.));
#29344=DIRECTION('center_axis',(-0.918541592796831,0.,-0.395324350758034));
#29345=DIRECTION('ref_axis',(-0.395324350758034,0.,0.918541592796831));
#29346=DIRECTION('',(0.,1.,0.));
#29347=DIRECTION('center_axis',(0.957753277410307,0.,0.287591132703732));
#29348=DIRECTION('ref_axis',(0.287591132703732,0.,-0.957753277410307));
#29349=DIRECTION('',(0.,1.,0.));
#29350=DIRECTION('center_axis',(0.,1.,0.));
#29351=DIRECTION('ref_axis',(-0.260729580930624,0.,-0.965411873568862));
#29352=DIRECTION('',(0.,-1.,0.));
#29353=DIRECTION('',(0.,1.,0.));
#29354=DIRECTION('center_axis',(-0.957753277410307,0.,0.287591132703732));
#29355=DIRECTION('ref_axis',(0.287591132703732,0.,0.957753277410307));
#29356=DIRECTION('',(0.,1.,0.));
#29357=DIRECTION('center_axis',(0.918541592796829,0.,-0.395324350758037));
#29358=DIRECTION('ref_axis',(-0.395324350758037,0.,-0.918541592796829));
#29359=DIRECTION('',(0.,1.,0.));
#29360=DIRECTION('center_axis',(0.,1.,0.));
#29361=DIRECTION('ref_axis',(-0.820285237202974,0.,-0.571954656967543));
#29362=DIRECTION('',(0.,-1.,0.));
#29363=DIRECTION('',(0.,1.,0.));
#29364=DIRECTION('center_axis',(-0.548821559281478,0.,0.835939528954007));
#29365=DIRECTION('ref_axis',(0.835939528954007,0.,0.548821559281478));
#29366=DIRECTION('',(0.,1.,0.));
#29367=DIRECTION('center_axis',(0.449534088461031,0.,-0.89326317695935));
#29368=DIRECTION('ref_axis',(-0.89326317695935,0.,-0.449534088461031));
#29369=DIRECTION('',(0.,1.,0.));
#29370=DIRECTION('center_axis',(0.,1.,0.));
#29371=DIRECTION('ref_axis',(-0.575195970587437,0.,-0.818015644972623));
#29372=DIRECTION('',(0.,-1.,0.));
#29373=DIRECTION('',(0.,1.,0.));
#29374=DIRECTION('center_axis',(-0.801631726889462,0.,0.597818178415661));
#29375=DIRECTION('ref_axis',(0.597818178415661,0.,0.801631726889462));
#29376=DIRECTION('',(0.,1.,0.));
#29377=DIRECTION('center_axis',(0.727937865529719,0.,-0.685643102443273));
#29378=DIRECTION('ref_axis',(-0.685643102443273,0.,-0.727937865529719));
#29379=DIRECTION('',(0.,1.,0.));
#29380=DIRECTION('center_axis',(0.,1.,0.));
#29381=DIRECTION('ref_axis',(0.0851846441452059,0.,-0.996365182250893));
#29382=DIRECTION('',(0.,-1.,0.));
#29383=DIRECTION('',(0.,1.,0.));
#29384=DIRECTION('center_axis',(-0.998355647742506,0.,-0.0573236480053483));
#29385=DIRECTION('ref_axis',(-0.0573236480053483,0.,0.998355647742506));
#29386=DIRECTION('',(0.,1.,0.));
#29387=DIRECTION('center_axis',(0.998355647742506,0.,-0.0573236480053483));
#29388=DIRECTION('ref_axis',(-0.0573236480053483,0.,-0.998355647742506));
#29389=DIRECTION('',(0.,1.,0.));
#29390=DIRECTION('center_axis',(0.,1.,0.));
#29391=DIRECTION('ref_axis',(0.705706417160429,0.,-0.708504377388447));
#29392=DIRECTION('',(0.,-1.,0.));
#29393=DIRECTION('',(0.,1.,0.));
#29394=DIRECTION('center_axis',(-0.727937865529722,0.,-0.68564310244327));
#29395=DIRECTION('ref_axis',(-0.68564310244327,0.,0.727937865529722));
#29396=DIRECTION('',(0.,1.,0.));
#29397=DIRECTION('center_axis',(0.801631726889465,0.,0.597818178415657));
#29398=DIRECTION('ref_axis',(0.597818178415657,0.,-0.801631726889465));
#29399=DIRECTION('',(0.,1.,0.));
#29400=DIRECTION('center_axis',(0.,1.,0.));
#29401=DIRECTION('ref_axis',(0.996020314533121,0.,-0.0891265001968739));
#29402=DIRECTION('',(0.,-1.,0.));
#29403=DIRECTION('',(0.,1.,0.));
#29404=DIRECTION('center_axis',(-0.116909865907364,0.,-0.993142529173694));
#29405=DIRECTION('ref_axis',(-0.993142529173694,0.,0.116909865907364));
#29406=DIRECTION('',(0.,1.,0.));
#29407=DIRECTION('center_axis',(0.229815411880577,0.,0.973234235146997));
#29408=DIRECTION('ref_axis',(0.973234235146997,0.,-0.229815411880577));
#29409=DIRECTION('',(0.,1.,0.));
#29410=DIRECTION('center_axis',(0.,1.,0.));
#29411=DIRECTION('ref_axis',(0.966435998091084,0.,0.256907496180414));
#29412=DIRECTION('',(0.,-1.,0.));
#29413=DIRECTION('',(0.,1.,0.));
#29414=DIRECTION('center_axis',(0.229815411880577,0.,-0.973234235146997));
#29415=DIRECTION('ref_axis',(-0.973234235146997,0.,-0.229815411880577));
#29416=DIRECTION('',(0.,1.,0.));
#29417=DIRECTION('center_axis',(-0.116909865907365,0.,0.993142529173694));
#29418=DIRECTION('ref_axis',(0.993142529173694,0.,0.116909865907365));
#29419=DIRECTION('',(0.,1.,0.));
#29420=DIRECTION('center_axis',(0.,1.,0.));
#29421=DIRECTION('ref_axis',(0.575195970587441,0.,0.818015644972621));
#29422=DIRECTION('',(0.,-1.,0.));
#29423=DIRECTION('',(0.,1.,0.));
#29424=DIRECTION('center_axis',(0.801631726889463,0.,-0.597818178415659));
#29425=DIRECTION('ref_axis',(-0.597818178415659,0.,-0.801631726889463));
#29426=DIRECTION('',(0.,1.,0.));
#29427=DIRECTION('center_axis',(-0.72793786552972,0.,0.685643102443272));
#29428=DIRECTION('ref_axis',(0.685643102443272,0.,0.72793786552972));
#29429=DIRECTION('',(0.,1.,0.));
#29430=DIRECTION('center_axis',(0.,1.,0.));
#29431=DIRECTION('ref_axis',(-0.0851846441452059,0.,0.996365182250893));
#29432=DIRECTION('',(0.,-1.,0.));
#29433=DIRECTION('',(0.,1.,0.));
#29434=DIRECTION('center_axis',(0.998355647742506,0.,0.0573236480053483));
#29435=DIRECTION('ref_axis',(0.0573236480053483,0.,-0.998355647742506));
#29436=DIRECTION('',(0.,1.,0.));
#29437=DIRECTION('center_axis',(-0.998355647742506,0.,0.0573236480053525));
#29438=DIRECTION('ref_axis',(0.0573236480053525,0.,0.998355647742506));
#29439=DIRECTION('',(0.,1.,0.));
#29440=DIRECTION('center_axis',(0.,1.,0.));
#29441=DIRECTION('ref_axis',(-0.705706417160429,0.,0.708504377388447));
#29442=DIRECTION('',(0.,-1.,0.));
#29443=DIRECTION('',(0.,1.,0.));
#29444=DIRECTION('center_axis',(0.727937865529721,0.,0.685643102443271));
#29445=DIRECTION('ref_axis',(0.685643102443271,0.,-0.727937865529721));
#29446=DIRECTION('',(0.,1.,0.));
#29447=DIRECTION('center_axis',(-0.801631726889465,0.,-0.597818178415657));
#29448=DIRECTION('ref_axis',(-0.597818178415657,0.,0.801631726889465));
#29449=DIRECTION('',(0.,1.,0.));
#29450=DIRECTION('center_axis',(0.,1.,0.));
#29451=DIRECTION('ref_axis',(-0.996020314533121,0.,0.0891265001968672));
#29452=DIRECTION('',(0.,-1.,0.));
#29453=DIRECTION('',(0.,1.,0.));
#29454=DIRECTION('center_axis',(0.116909865907365,0.,0.993142529173694));
#29455=DIRECTION('ref_axis',(0.993142529173694,0.,-0.116909865907365));
#29456=DIRECTION('',(0.,1.,0.));
#29457=DIRECTION('center_axis',(-0.229815411880577,0.,-0.973234235146997));
#29458=DIRECTION('ref_axis',(-0.973234235146997,0.,0.229815411880577));
#29459=DIRECTION('center_axis',(0.,1.,0.));
#29460=DIRECTION('ref_axis',(1.,0.,0.));
#29461=DIRECTION('center_axis',(0.,1.,0.));
#29462=DIRECTION('ref_axis',(1.,0.,0.));
#29463=DIRECTION('center_axis',(0.,1.,0.));
#29464=DIRECTION('ref_axis',(1.,0.,0.));
#29465=DIRECTION('center_axis',(0.,1.,0.));
#29466=DIRECTION('ref_axis',(1.,0.,0.));
#29467=DIRECTION('center_axis',(0.,1.,0.));
#29468=DIRECTION('ref_axis',(1.,0.,0.));
#29469=DIRECTION('center_axis',(0.,1.,0.));
#29470=DIRECTION('ref_axis',(1.,0.,0.));
#29471=DIRECTION('center_axis',(0.,1.,0.));
#29472=DIRECTION('ref_axis',(1.,0.,0.));
#29473=DIRECTION('center_axis',(0.,1.,0.));
#29474=DIRECTION('ref_axis',(1.,0.,0.));
#29475=DIRECTION('center_axis',(0.,1.,0.));
#29476=DIRECTION('ref_axis',(1.,0.,0.));
#29477=DIRECTION('center_axis',(0.,1.,0.));
#29478=DIRECTION('ref_axis',(-1.,0.,-2.5785718345414E-11));
#29479=DIRECTION('center_axis',(0.,1.,0.));
#29480=DIRECTION('ref_axis',(1.,0.,0.));
#29481=DIRECTION('center_axis',(0.,1.,0.));
#29482=DIRECTION('ref_axis',(1.,0.,0.));
#29483=DIRECTION('center_axis',(0.,1.,0.));
#29484=DIRECTION('ref_axis',(1.,0.,0.));
#29485=DIRECTION('center_axis',(0.,1.,0.));
#29486=DIRECTION('ref_axis',(1.,0.,0.));
#29487=DIRECTION('center_axis',(0.,1.,0.));
#29488=DIRECTION('ref_axis',(1.,0.,0.));
#29489=DIRECTION('center_axis',(0.,1.,0.));
#29490=DIRECTION('ref_axis',(1.,0.,0.));
#29491=DIRECTION('center_axis',(0.,1.,0.));
#29492=DIRECTION('ref_axis',(1.,0.,0.));
#29493=DIRECTION('center_axis',(0.,1.,0.));
#29494=DIRECTION('ref_axis',(1.,0.,0.));
#29495=DIRECTION('axis',(0.,0.,1.));
#29496=DIRECTION('refdir',(1.,0.,0.));
#29497=DIRECTION('center_axis',(0.,0.,1.));
#29498=DIRECTION('ref_axis',(1.,0.,0.));
#29499=DIRECTION('',(0.,0.,-1.));
#29500=DIRECTION('center_axis',(0.,0.,-1.));
#29501=DIRECTION('ref_axis',(1.,0.,0.));
#29502=DIRECTION('center_axis',(0.,0.,1.));
#29503=DIRECTION('ref_axis',(1.,0.,0.));
#29504=DIRECTION('',(0.,0.,-1.));
#29505=DIRECTION('center_axis',(0.,0.,1.));
#29506=DIRECTION('ref_axis',(1.,0.,0.));
#29507=DIRECTION('',(0.,0.,-1.));
#29508=DIRECTION('center_axis',(0.,0.,1.));
#29509=DIRECTION('ref_axis',(1.,0.,0.));
#29510=DIRECTION('',(0.,0.,-1.));
#29511=DIRECTION('center_axis',(0.,0.,1.));
#29512=DIRECTION('ref_axis',(1.,0.,0.));
#29513=DIRECTION('',(0.,0.,-1.));
#29514=DIRECTION('center_axis',(0.,0.,1.));
#29515=DIRECTION('ref_axis',(1.,0.,0.));
#29516=DIRECTION('',(0.,0.,-1.));
#29517=DIRECTION('center_axis',(0.,0.,1.));
#29518=DIRECTION('ref_axis',(1.,0.,0.));
#29519=DIRECTION('',(0.,0.,-1.));
#29520=DIRECTION('center_axis',(0.,0.,1.));
#29521=DIRECTION('ref_axis',(1.,0.,0.));
#29522=DIRECTION('',(0.,0.,-1.));
#29523=DIRECTION('center_axis',(0.,0.,1.));
#29524=DIRECTION('ref_axis',(1.,0.,0.));
#29525=DIRECTION('',(0.,0.,-1.));
#29526=DIRECTION('center_axis',(0.,0.,1.));
#29527=DIRECTION('ref_axis',(1.,0.,0.));
#29528=DIRECTION('',(0.,0.,-1.));
#29529=DIRECTION('center_axis',(0.,0.,1.));
#29530=DIRECTION('ref_axis',(1.,0.,0.));
#29531=DIRECTION('',(0.,0.,-1.));
#29532=DIRECTION('center_axis',(0.,0.,1.));
#29533=DIRECTION('ref_axis',(1.,0.,0.));
#29534=DIRECTION('',(0.,0.,-1.));
#29535=DIRECTION('center_axis',(0.,0.,1.));
#29536=DIRECTION('ref_axis',(1.,0.,0.));
#29537=DIRECTION('',(0.,0.,-1.));
#29538=DIRECTION('center_axis',(0.,0.,1.));
#29539=DIRECTION('ref_axis',(1.,7.08873565758722E-14,0.));
#29540=DIRECTION('',(0.,0.,1.));
#29541=DIRECTION('center_axis',(0.,0.,1.));
#29542=DIRECTION('ref_axis',(1.,7.08873565758722E-14,0.));
#29543=DIRECTION('center_axis',(0.,0.,1.));
#29544=DIRECTION('ref_axis',(1.,7.08873565758722E-14,0.));
#29545=DIRECTION('',(0.,0.,1.));
#29546=DIRECTION('center_axis',(0.,0.,1.));
#29547=DIRECTION('ref_axis',(1.,7.08873565758722E-14,0.));
#29548=DIRECTION('center_axis',(0.,0.,1.));
#29549=DIRECTION('ref_axis',(1.,7.08873565758722E-14,0.));
#29550=DIRECTION('',(0.,0.,1.));
#29551=DIRECTION('center_axis',(0.,0.,1.));
#29552=DIRECTION('ref_axis',(1.,7.08873565758722E-14,0.));
#29553=DIRECTION('',(0.,0.,1.));
#29554=DIRECTION('center_axis',(0.,0.,1.));
#29555=DIRECTION('ref_axis',(1.,7.08873565758722E-14,0.));
#29556=DIRECTION('',(0.,0.,1.));
#29557=DIRECTION('center_axis',(0.,0.,1.));
#29558=DIRECTION('ref_axis',(1.,7.08873565758722E-14,0.));
#29559=DIRECTION('',(0.,0.,1.));
#29560=DIRECTION('center_axis',(0.,0.,1.));
#29561=DIRECTION('ref_axis',(1.,7.08873565758722E-14,0.));
#29562=DIRECTION('',(0.,0.,1.));
#29563=DIRECTION('center_axis',(0.,0.,1.));
#29564=DIRECTION('ref_axis',(1.,7.08873565758722E-14,0.));
#29565=DIRECTION('',(0.,0.,1.));
#29566=DIRECTION('center_axis',(0.,0.,1.));
#29567=DIRECTION('ref_axis',(1.,7.08873565758722E-14,0.));
#29568=DIRECTION('',(0.,0.,1.));
#29569=DIRECTION('center_axis',(0.,0.,1.));
#29570=DIRECTION('ref_axis',(1.,7.08873565758722E-14,0.));
#29571=DIRECTION('',(0.,0.,1.));
#29572=DIRECTION('center_axis',(0.,0.,1.));
#29573=DIRECTION('ref_axis',(1.,7.08873565758722E-14,0.));
#29574=DIRECTION('',(0.,0.,1.));
#29575=DIRECTION('center_axis',(0.,0.,1.));
#29576=DIRECTION('ref_axis',(1.,7.08873565758722E-14,0.));
#29577=DIRECTION('',(0.,0.,1.));
#29578=DIRECTION('center_axis',(0.,0.,1.));
#29579=DIRECTION('ref_axis',(1.,7.08873565758722E-14,0.));
#29580=DIRECTION('',(0.,0.,1.));
#29581=DIRECTION('center_axis',(0.,0.,1.));
#29582=DIRECTION('ref_axis',(1.,0.,0.));
#29583=DIRECTION('center_axis',(0.,0.,-1.));
#29584=DIRECTION('ref_axis',(1.,0.,0.));
#29585=DIRECTION('center_axis',(0.,0.,-1.));
#29586=DIRECTION('ref_axis',(1.,0.,0.));
#29587=DIRECTION('center_axis',(0.,0.,1.));
#29588=DIRECTION('ref_axis',(1.,0.,0.));
#29589=DIRECTION('center_axis',(0.,0.,-1.));
#29590=DIRECTION('ref_axis',(1.,0.,0.));
#29591=DIRECTION('center_axis',(0.,0.,-1.));
#29592=DIRECTION('ref_axis',(1.,0.,0.));
#29593=DIRECTION('center_axis',(0.,0.,-1.));
#29594=DIRECTION('ref_axis',(1.,7.08873565758722E-14,0.));
#29595=DIRECTION('center_axis',(0.,0.,1.));
#29596=DIRECTION('ref_axis',(0.888987612330369,0.457931244973685,0.));
#29597=DIRECTION('center_axis',(0.,0.,1.));
#29598=DIRECTION('ref_axis',(1.,0.,0.));
#29599=DIRECTION('center_axis',(0.,0.,-1.));
#29600=DIRECTION('ref_axis',(1.,0.,0.));
#29601=DIRECTION('center_axis',(0.,0.,-1.));
#29602=DIRECTION('ref_axis',(-1.,0.,0.));
#29603=DIRECTION('center_axis',(0.,0.,1.));
#29604=DIRECTION('ref_axis',(1.,0.,0.));
#29605=DIRECTION('center_axis',(0.,0.,1.));
#29606=DIRECTION('ref_axis',(1.,0.,0.));
#29607=DIRECTION('center_axis',(0.,0.,1.));
#29608=DIRECTION('ref_axis',(1.,0.,0.));
#29609=DIRECTION('',(0.707106781186547,8.65956056235492E-17,-0.707106781186548));
#29610=DIRECTION('center_axis',(0.,0.,1.));
#29611=DIRECTION('ref_axis',(1.,0.,0.));
#29612=DIRECTION('center_axis',(0.,0.,1.));
#29613=DIRECTION('ref_axis',(1.,0.,0.));
#29614=DIRECTION('',(0.,0.,-1.));
#29615=DIRECTION('center_axis',(0.,0.,1.));
#29616=DIRECTION('ref_axis',(1.,0.,0.));
#29617=DIRECTION('center_axis',(0.,0.,1.));
#29618=DIRECTION('ref_axis',(1.,0.,0.));
#29619=DIRECTION('center_axis',(0.,0.,-1.));
#29620=DIRECTION('ref_axis',(1.,0.,0.));
#29621=DIRECTION('',(-0.707106781186568,-8.65956056235518E-17,-0.707106781186527));
#29622=DIRECTION('center_axis',(0.,0.,-1.));
#29623=DIRECTION('ref_axis',(1.,0.,0.));
#29624=DIRECTION('center_axis',(0.,0.,1.));
#29625=DIRECTION('ref_axis',(1.,0.,0.));
#29626=DIRECTION('',(-0.707106781186551,-8.65956056235497E-17,-0.707106781186544));
#29627=DIRECTION('center_axis',(0.,0.,1.));
#29628=DIRECTION('ref_axis',(1.,0.,0.));
#29629=DIRECTION('axis',(0.,0.,1.));
#29630=DIRECTION('refdir',(1.,0.,0.));
#29631=DIRECTION('center_axis',(-0.676715943576134,0.736244206571341,0.));
#29632=DIRECTION('ref_axis',(0.,0.,1.));
#29633=DIRECTION('',(0.,0.,-1.));
#29634=DIRECTION('',(-0.592886939594824,-0.54494967998502,0.592886939594817));
#29635=DIRECTION('',(0.,0.,1.));
#29636=DIRECTION('',(0.592886939594818,0.544949679985014,0.592886939594828));
#29637=DIRECTION('center_axis',(0.,0.,1.));
#29638=DIRECTION('ref_axis',(1.,0.,0.));
#29639=DIRECTION('center_axis',(0.,0.,1.));
#29640=DIRECTION('ref_axis',(1.,0.,0.));
#29641=DIRECTION('',(0.,0.,1.));
#29642=DIRECTION('center_axis',(0.,0.,-1.));
#29643=DIRECTION('ref_axis',(1.,0.,0.));
#29644=DIRECTION('center_axis',(0.,0.,-1.));
#29645=DIRECTION('ref_axis',(1.,0.,0.));
#29646=DIRECTION('center_axis',(0.,0.,1.));
#29647=DIRECTION('ref_axis',(1.,6.12323399573677E-17,0.));
#29648=DIRECTION('center_axis',(-0.707106781186554,1.3579178021049E-16,
0.707106781186541));
#29649=DIRECTION('ref_axis',(0.707106781186541,0.,0.707106781186554));
#29650=DIRECTION('',(-1.9203857723246E-16,-1.,0.));
#29651=DIRECTION('',(0.707106781186541,0.,0.707106781186554));
#29652=DIRECTION('',(1.9203857723246E-16,1.,0.));
#29653=DIRECTION('center_axis',(0.676715943576129,0.736244206571345,0.));
#29654=DIRECTION('ref_axis',(0.,0.,-1.));
#29655=DIRECTION('',(0.,0.,1.));
#29656=DIRECTION('',(0.59288693959482,-0.54494967998501,-0.59288693959483));
#29657=DIRECTION('',(0.,0.,-1.));
#29658=DIRECTION('',(-0.592886939594826,0.544949679985016,-0.592886939594819));
#29659=DIRECTION('center_axis',(0.707106781186543,-1.35791780210488E-16,
-0.707106781186552));
#29660=DIRECTION('ref_axis',(-0.707106781186552,0.,-0.707106781186543));
#29661=DIRECTION('',(-1.9203857723246E-16,-1.,0.));
#29662=DIRECTION('',(-0.707106781186552,0.,-0.707106781186543));
#29663=DIRECTION('',(1.9203857723246E-16,1.,0.));
#29664=DIRECTION('center_axis',(-1.,1.9203857723246E-16,0.));
#29665=DIRECTION('ref_axis',(1.9203857723246E-16,1.,0.));
#29666=DIRECTION('',(1.9203857723246E-16,1.,0.));
#29667=DIRECTION('',(0.,0.,-1.));
#29668=DIRECTION('center_axis',(0.707106781186554,-1.3579178021049E-16,
0.707106781186541));
#29669=DIRECTION('ref_axis',(0.707106781186541,0.,-0.707106781186554));
#29670=DIRECTION('',(-1.9203857723246E-16,-1.,0.));
#29671=DIRECTION('',(-0.707106781186548,0.,0.707106781186548));
#29672=DIRECTION('center_axis',(0.,0.,-1.));
#29673=DIRECTION('ref_axis',(-1.,0.,0.));
#29674=DIRECTION('',(0.707106781186548,0.,-0.707106781186548));
#29675=DIRECTION('center_axis',(0.,0.,-1.));
#29676=DIRECTION('ref_axis',(-1.,0.,0.));
#29677=DIRECTION('center_axis',(0.,0.,1.));
#29678=DIRECTION('ref_axis',(-1.,0.,0.));
#29679=DIRECTION('center_axis',(-0.707106781186543,1.35791780210488E-16,
-0.707106781186552));
#29680=DIRECTION('ref_axis',(-0.707106781186552,0.,0.707106781186543));
#29681=DIRECTION('',(-1.9203857723246E-16,-1.,0.));
#29682=DIRECTION('',(1.9203857723246E-16,1.,0.));
#29683=DIRECTION('center_axis',(0.,0.,1.));
#29684=DIRECTION('ref_axis',(1.,0.,0.));
#29685=DIRECTION('center_axis',(0.,0.,1.));
#29686=DIRECTION('ref_axis',(1.,0.,0.));
#29687=DIRECTION('',(1.,0.,0.));
#29688=DIRECTION('center_axis',(0.,0.,-1.));
#29689=DIRECTION('ref_axis',(0.,1.,0.));
#29690=DIRECTION('',(-1.,0.,0.));
#29691=DIRECTION('center_axis',(0.,0.,1.));
#29692=DIRECTION('ref_axis',(1.,0.,0.));
#29693=DIRECTION('',(-1.9203857723246E-16,-1.,0.));
#29694=DIRECTION('center_axis',(0.,0.,-1.));
#29695=DIRECTION('ref_axis',(1.,0.,0.));
#29696=DIRECTION('',(1.44028932924345E-16,1.,0.));
#29697=DIRECTION('center_axis',(0.,0.,1.));
#29698=DIRECTION('ref_axis',(1.,0.,0.));
#29699=DIRECTION('',(-1.,1.20024110770287E-16,0.));
#29700=DIRECTION('center_axis',(0.,0.,-1.));
#29701=DIRECTION('ref_axis',(-2.88998133608509E-16,-1.,0.));
#29702=DIRECTION('',(1.,-1.44028932924345E-16,0.));
#29703=DIRECTION('center_axis',(0.,0.,1.));
#29704=DIRECTION('ref_axis',(1.,0.,0.));
#29705=DIRECTION('center_axis',(0.,0.,-1.));
#29706=DIRECTION('ref_axis',(1.,0.,0.));
#29707=DIRECTION('center_axis',(0.,0.,1.));
#29708=DIRECTION('ref_axis',(1.,0.,0.));
#29709=DIRECTION('center_axis',(0.76788343892593,0.640589591098144,0.));
#29710=DIRECTION('ref_axis',(0.,0.,-1.));
#29711=DIRECTION('',(0.,0.,-1.));
#29712=DIRECTION('',(-0.508077317375032,0.609039177544843,0.609039177544837));
#29713=DIRECTION('',(0.,0.,1.));
#29714=DIRECTION('',(0.508077317375028,-0.609039177544838,0.609039177544846));
#29715=DIRECTION('center_axis',(0.,0.707106781186552,0.707106781186543));
#29716=DIRECTION('ref_axis',(1.,0.,0.));
#29717=DIRECTION('',(-1.,0.,0.));
#29718=DIRECTION('',(0.,-0.707106781186543,0.707106781186552));
#29719=DIRECTION('',(1.,0.,0.));
#29720=DIRECTION('center_axis',(0.,-1.,0.));
#29721=DIRECTION('ref_axis',(-1.,0.,0.));
#29722=DIRECTION('',(1.,0.,0.));
#29723=DIRECTION('',(0.,0.,-1.));
#29724=DIRECTION('center_axis',(0.,0.707106781186544,-0.707106781186551));
#29725=DIRECTION('ref_axis',(-1.,0.,0.));
#29726=DIRECTION('',(0.,-0.707106781186548,-0.707106781186548));
#29727=DIRECTION('center_axis',(0.76788343892593,-0.640589591098144,0.));
#29728=DIRECTION('ref_axis',(0.,0.,-1.));
#29729=DIRECTION('',(-0.508077317375028,-0.609039177544838,-0.609039177544846));
#29730=DIRECTION('',(0.,0.,-1.));
#29731=DIRECTION('',(0.508077317375032,0.609039177544843,-0.609039177544837));
#29732=DIRECTION('center_axis',(0.,-0.707106781186544,-0.707106781186551));
#29733=DIRECTION('ref_axis',(-1.,0.,0.));
#29734=DIRECTION('',(-1.,0.,0.));
#29735=DIRECTION('',(0.,0.707106781186551,-0.707106781186544));
#29736=DIRECTION('center_axis',(0.,0.,-1.));
#29737=DIRECTION('ref_axis',(0.,1.,0.));
#29738=DIRECTION('center_axis',(0.,0.,1.));
#29739=DIRECTION('ref_axis',(0.,1.,0.));
#29740=DIRECTION('center_axis',(0.,0.,1.));
#29741=DIRECTION('ref_axis',(1.,0.,0.));
#29742=DIRECTION('center_axis',(0.,0.,-1.));
#29743=DIRECTION('ref_axis',(1.,0.,0.));
#29744=DIRECTION('center_axis',(0.,0.,-1.));
#29745=DIRECTION('ref_axis',(0.,1.,0.));
#29746=DIRECTION('',(0.,0.,-1.));
#29747=DIRECTION('center_axis',(0.,0.,-1.));
#29748=DIRECTION('ref_axis',(0.,1.,0.));
#29749=DIRECTION('center_axis',(0.,1.,0.));
#29750=DIRECTION('ref_axis',(1.,0.,0.));
#29751=DIRECTION('',(1.,0.,0.));
#29752=DIRECTION('center_axis',(0.,0.,-1.));
#29753=DIRECTION('ref_axis',(1.,0.,0.));
#29754=DIRECTION('',(0.707106781186548,-8.65956056235493E-17,0.707106781186548));
#29755=DIRECTION('center_axis',(0.,0.,1.));
#29756=DIRECTION('ref_axis',(1.,0.,0.));
#29757=DIRECTION('center_axis',(0.,0.,-1.));
#29758=DIRECTION('ref_axis',(1.,0.,0.));
#29759=DIRECTION('center_axis',(0.,0.,-1.));
#29760=DIRECTION('ref_axis',(1.,0.,0.));
#29761=DIRECTION('',(0.,0.,-1.));
#29762=DIRECTION('center_axis',(-0.752232026437047,-0.658898306571215,0.));
#29763=DIRECTION('ref_axis',(0.,0.,1.));
#29764=DIRECTION('',(0.,0.,-1.));
#29765=DIRECTION('',(0.526553973041879,-0.601140962451329,0.601140962451322));
#29766=DIRECTION('',(0.,0.,1.));
#29767=DIRECTION('',(-0.526553973041875,0.601140962451325,0.60114096245133));
#29768=DIRECTION('center_axis',(-1.01843835157867E-16,-0.707106781186551,
0.707106781186544));
#29769=DIRECTION('ref_axis',(1.,0.,1.44028932924346E-16));
#29770=DIRECTION('',(1.,-1.44028932924345E-16,0.));
#29771=DIRECTION('',(-3.23639307574421E-16,0.707106781186544,0.707106781186551));
#29772=DIRECTION('',(-1.,1.44028932924345E-16,0.));
#29773=DIRECTION('center_axis',(1.44028932924345E-16,1.,0.));
#29774=DIRECTION('ref_axis',(1.,-1.44028932924345E-16,0.));
#29775=DIRECTION('',(-1.,1.44028932924345E-16,0.));
#29776=DIRECTION('',(0.,0.,-1.));
#29777=DIRECTION('center_axis',(-1.01843835157866E-16,-0.707106781186543,
-0.707106781186552));
#29778=DIRECTION('ref_axis',(-1.,0.,1.44028932924343E-16));
#29779=DIRECTION('',(2.9094814564838E-16,0.707106781186548,-0.707106781186548));
#29780=DIRECTION('center_axis',(-0.752232026437047,0.658898306571214,0.));
#29781=DIRECTION('ref_axis',(0.,0.,1.));
#29782=DIRECTION('',(0.,0.,1.));
#29783=DIRECTION('',(0.526553973041873,0.601140962451323,-0.601140962451333));
#29784=DIRECTION('',(0.,0.,-1.));
#29785=DIRECTION('',(-0.526553973041878,-0.601140962451329,-0.601140962451323));
#29786=DIRECTION('center_axis',(0.,0.,1.));
#29787=DIRECTION('ref_axis',(1.,0.,0.));
#29788=DIRECTION('center_axis',(0.,0.,-1.));
#29789=DIRECTION('ref_axis',(1.,0.,0.));
#29790=DIRECTION('',(0.,0.,-1.));
#29791=DIRECTION('center_axis',(0.,0.,1.));
#29792=DIRECTION('ref_axis',(1.,0.,0.));
#29793=DIRECTION('center_axis',(0.,0.,1.));
#29794=DIRECTION('ref_axis',(1.,0.,0.));
#29795=DIRECTION('center_axis',(8.4869862631555E-17,0.707106781186544,-0.707106781186551));
#29796=DIRECTION('ref_axis',(-1.,0.,-1.20024110770286E-16));
#29797=DIRECTION('',(1.,-1.20024110770287E-16,0.));
#29798=DIRECTION('',(-9.38848536597713E-16,-0.707106781186551,-0.707106781186544));
#29799=DIRECTION('center_axis',(0.,0.,-1.));
#29800=DIRECTION('ref_axis',(-2.88998133608509E-16,-1.,0.));
#29801=DIRECTION('center_axis',(0.,0.,1.));
#29802=DIRECTION('ref_axis',(-2.88998133608509E-16,-1.,0.));
#29803=DIRECTION('center_axis',(0.,0.,-1.));
#29804=DIRECTION('ref_axis',(-2.88998133608509E-16,-1.,0.));
#29805=DIRECTION('',(0.,0.,-1.));
#29806=DIRECTION('center_axis',(0.,0.,-1.));
#29807=DIRECTION('ref_axis',(-2.88998133608509E-16,-1.,0.));
#29808=DIRECTION('center_axis',(-1.20024110770287E-16,-1.,0.));
#29809=DIRECTION('ref_axis',(-1.,1.20024110770287E-16,0.));
#29810=DIRECTION('',(-1.,1.20024110770287E-16,0.));
#29811=DIRECTION('center_axis',(0.621746515478052,-0.783218533035895,0.));
#29812=DIRECTION('ref_axis',(0.,0.,-1.));
#29813=DIRECTION('',(0.616605963274096,0.48948357695602,0.616605963274087));
#29814=DIRECTION('',(0.,0.,1.));
#29815=DIRECTION('',(-0.616605963274091,-0.489483576956017,0.616605963274094));
#29816=DIRECTION('center_axis',(0.707106781186549,-1.01843835157867E-16,
0.707106781186546));
#29817=DIRECTION('ref_axis',(0.707106781186546,0.,-0.707106781186549));
#29818=DIRECTION('',(1.44028932924345E-16,1.,0.));
#29819=DIRECTION('',(-0.707106781186544,0.,0.707106781186551));
#29820=DIRECTION('',(-1.44028932924345E-16,-1.,0.));
#29821=DIRECTION('center_axis',(-1.,1.44028932924345E-16,0.));
#29822=DIRECTION('ref_axis',(1.44028932924345E-16,1.,0.));
#29823=DIRECTION('',(-1.44028932924345E-16,-1.,0.));
#29824=DIRECTION('',(0.,0.,-1.));
#29825=DIRECTION('center_axis',(0.707106781186542,-1.01843835157866E-16,
-0.707106781186553));
#29826=DIRECTION('ref_axis',(-0.707106781186553,0.,-0.707106781186542));
#29827=DIRECTION('',(-0.707106781186546,4.18691322315673E-15,-0.707106781186549));
#29828=DIRECTION('center_axis',(-0.621746515478056,-0.783218533035893,0.));
#29829=DIRECTION('ref_axis',(0.,0.,1.));
#29830=DIRECTION('',(0.,0.,1.));
#29831=DIRECTION('',(-0.616605963274087,0.489483576956018,-0.616605963274098));
#29832=DIRECTION('',(0.,0.,-1.));
#29833=DIRECTION('',(0.616605963274094,-0.489483576956023,-0.616605963274087));
#29834=DIRECTION('center_axis',(0.,0.,1.));
#29835=DIRECTION('ref_axis',(1.,0.,0.));
#29836=DIRECTION('center_axis',(0.,0.,1.));
#29837=DIRECTION('ref_axis',(1.,0.,0.));
#29838=DIRECTION('center_axis',(-0.707106781186543,1.35791780210488E-16,
-0.707106781186552));
#29839=DIRECTION('ref_axis',(-0.707106781186552,0.,0.707106781186543));
#29840=DIRECTION('',(1.9203857723246E-16,1.,0.));
#29841=DIRECTION('',(0.707106781186552,0.,-0.707106781186543));
#29842=DIRECTION('center_axis',(0.,0.,-1.));
#29843=DIRECTION('ref_axis',(1.,0.,0.));
#29844=DIRECTION('center_axis',(0.,0.,1.));
#29845=DIRECTION('ref_axis',(1.,0.,0.));
#29846=DIRECTION('center_axis',(0.,0.,-1.));
#29847=DIRECTION('ref_axis',(1.,0.,0.));
#29848=DIRECTION('',(0.,0.,-1.));
#29849=DIRECTION('center_axis',(0.,0.,-1.));
#29850=DIRECTION('ref_axis',(1.,0.,0.));
#29851=DIRECTION('center_axis',(1.,-1.9203857723246E-16,0.));
#29852=DIRECTION('ref_axis',(-1.9203857723246E-16,-1.,0.));
#29853=DIRECTION('',(-1.9203857723246E-16,-1.,0.));
#29854=DIRECTION('center_axis',(0.,-1.35268490144193E-14,-1.));
#29855=DIRECTION('ref_axis',(-1.,-3.07843832903329E-17,0.));
#29856=DIRECTION('center_axis',(0.,0.,-1.));
#29857=DIRECTION('ref_axis',(-1.,0.,0.));
#29858=DIRECTION('center_axis',(0.,0.,1.));
#29859=DIRECTION('ref_axis',(-1.,-6.12323399573677E-17,0.));
#29860=DIRECTION('center_axis',(0.,-1.35268490144193E-14,-1.));
#29861=DIRECTION('ref_axis',(-1.,-3.07843832903329E-17,0.));
#29862=DIRECTION('center_axis',(0.,0.,1.));
#29863=DIRECTION('ref_axis',(-1.,-6.12323399573677E-17,0.));
#29864=DIRECTION('center_axis',(0.,0.,-1.));
#29865=DIRECTION('ref_axis',(-1.,0.,0.));
#29866=DIRECTION('center_axis',(-2.51214793389404E-14,-1.35268490144193E-14,
-1.));
#29867=DIRECTION('ref_axis',(1.,3.07843832903329E-17,0.));
#29868=DIRECTION('center_axis',(0.,0.,-1.));
#29869=DIRECTION('ref_axis',(1.,0.,0.));
#29870=DIRECTION('center_axis',(1.25607396694696E-14,-1.35268490144186E-14,
-1.));
#29871=DIRECTION('ref_axis',(1.,3.07843832903329E-17,0.));
#29872=DIRECTION('center_axis',(-6.96322261624857E-33,1.13718055215539E-16,
1.));
#29873=DIRECTION('ref_axis',(1.,6.12323399573677E-17,0.));
#29874=DIRECTION('center_axis',(0.,0.,-1.));
#29875=DIRECTION('ref_axis',(1.,0.,0.));
#29876=DIRECTION('center_axis',(0.,0.,1.));
#29877=DIRECTION('ref_axis',(0.,1.,0.));
#29878=DIRECTION('',(0.,0.707106781186548,0.707106781186548));
#29879=DIRECTION('center_axis',(0.,0.,1.));
#29880=DIRECTION('ref_axis',(0.,1.,0.));
#29881=DIRECTION('center_axis',(0.,-0.707106781186552,0.707106781186543));
#29882=DIRECTION('ref_axis',(1.,0.,0.));
#29883=DIRECTION('',(-1.,0.,0.));
#29884=DIRECTION('center_axis',(0.,0.,1.));
#29885=DIRECTION('ref_axis',(1.,0.,0.));
#29886=DIRECTION('',(0.707106781186548,6.28036983473512E-15,0.707106781186548));
#29887=DIRECTION('center_axis',(0.,0.,1.));
#29888=DIRECTION('ref_axis',(1.,0.,0.));
#29889=DIRECTION('center_axis',(-0.707106781186554,1.3579178021049E-16,
0.707106781186541));
#29890=DIRECTION('ref_axis',(0.707106781186541,0.,0.707106781186554));
#29891=DIRECTION('',(1.9203857723246E-16,1.,0.));
#29892=DIRECTION('center_axis',(0.,0.,1.));
#29893=DIRECTION('ref_axis',(-1.,0.,0.));
#29894=DIRECTION('center_axis',(0.,0.,1.));
#29895=DIRECTION('ref_axis',(-1.,0.,0.));
#29896=DIRECTION('center_axis',(0.,0.,-1.));
#29897=DIRECTION('ref_axis',(-1.,0.,0.));
#29898=DIRECTION('center_axis',(0.,0.,1.));
#29899=DIRECTION('ref_axis',(-2.88998133608509E-16,-1.,0.));
#29900=DIRECTION('',(3.43266289616425E-15,-0.707106781186548,0.707106781186547));
#29901=DIRECTION('center_axis',(0.,0.,1.));
#29902=DIRECTION('ref_axis',(-2.88998133608509E-16,-1.,0.));
#29903=DIRECTION('center_axis',(8.48698626315561E-17,0.707106781186553,
0.707106781186542));
#29904=DIRECTION('ref_axis',(1.,0.,-1.20024110770289E-16));
#29905=DIRECTION('',(1.,-1.20024110770287E-16,0.));
#29906=DIRECTION('center_axis',(0.,0.,-1.));
#29907=DIRECTION('ref_axis',(1.,0.,0.));
#29908=DIRECTION('center_axis',(0.,0.,-1.));
#29909=DIRECTION('ref_axis',(1.,0.,0.));
#29910=DIRECTION('center_axis',(0.,0.,1.));
#29911=DIRECTION('ref_axis',(1.,0.,0.));
#29912=DIRECTION('center_axis',(0.,0.,1.));
#29913=DIRECTION('ref_axis',(1.,0.,0.));
#29914=DIRECTION('center_axis',(0.,0.,1.));
#29915=DIRECTION('ref_axis',(1.,0.,0.));
#29916=DIRECTION('',(0.707106781186548,8.65956056235493E-17,-0.707106781186548));
#29917=DIRECTION('center_axis',(0.,0.,-1.));
#29918=DIRECTION('ref_axis',(-1.,0.,0.));
#29919=DIRECTION('',(0.,0.,-1.));
#29920=DIRECTION('center_axis',(1.,-1.9203857723246E-16,0.));
#29921=DIRECTION('ref_axis',(-1.9203857723246E-16,-1.,0.));
#29922=DIRECTION('center_axis',(0.,0.,-1.));
#29923=DIRECTION('ref_axis',(1.,0.,0.));
#29924=DIRECTION('center_axis',(0.,0.,1.));
#29925=DIRECTION('ref_axis',(1.,0.,0.));
#29926=DIRECTION('center_axis',(0.,0.,1.));
#29927=DIRECTION('ref_axis',(1.,0.,0.));
#29928=DIRECTION('center_axis',(0.,0.,-1.));
#29929=DIRECTION('ref_axis',(1.,0.,0.));
#29930=DIRECTION('center_axis',(0.,0.,1.));
#29931=DIRECTION('ref_axis',(1.,0.,0.));
#29932=DIRECTION('axis',(0.,0.,1.));
#29933=DIRECTION('refdir',(1.,0.,0.));
#29934=DIRECTION('center_axis',(0.,0.,-1.));
#29935=DIRECTION('ref_axis',(-1.,0.,0.));
#29936=DIRECTION('center_axis',(0.,0.,1.));
#29937=DIRECTION('ref_axis',(1.,0.,0.));
#29938=DIRECTION('center_axis',(0.,0.,1.));
#29939=DIRECTION('ref_axis',(1.,0.,0.));
#29940=DIRECTION('center_axis',(0.,0.,1.));
#29941=DIRECTION('ref_axis',(1.,0.,0.));
#29942=DIRECTION('',(0.707106781186547,8.65956056235493E-17,-0.707106781186547));
#29943=DIRECTION('center_axis',(0.,0.,1.));
#29944=DIRECTION('ref_axis',(1.,0.,0.));
#29945=DIRECTION('center_axis',(0.,0.,1.));
#29946=DIRECTION('ref_axis',(1.,0.,0.));
#29947=DIRECTION('',(0.,0.,-1.));
#29948=DIRECTION('center_axis',(0.,0.,-1.));
#29949=DIRECTION('ref_axis',(1.,0.,0.));
#29950=DIRECTION('center_axis',(0.,0.,1.));
#29951=DIRECTION('ref_axis',(1.,0.,0.));
#29952=DIRECTION('',(-0.707106781186547,-8.65956056235493E-17,-0.707106781186547));
#29953=DIRECTION('center_axis',(0.,0.,1.));
#29954=DIRECTION('ref_axis',(1.,0.,0.));
#29955=DIRECTION('axis',(0.,0.,1.));
#29956=DIRECTION('refdir',(1.,0.,0.));
#29957=DIRECTION('',(0.747418957963599,8.91271585113921E-15,-0.664352994481554));
#29958=DIRECTION('center_axis',(0.,0.,1.));
#29959=DIRECTION('ref_axis',(1.,0.,0.));
#29960=DIRECTION('',(0.,0.,1.));
#29961=DIRECTION('center_axis',(0.,-1.,0.));
#29962=DIRECTION('ref_axis',(1.,0.,0.));
#29963=DIRECTION('center_axis',(0.,-1.,0.));
#29964=DIRECTION('ref_axis',(1.,0.,0.));
#29965=DIRECTION('',(0.,1.,0.));
#29966=DIRECTION('',(0.,1.,0.));
#29967=DIRECTION('center_axis',(0.,-1.,0.));
#29968=DIRECTION('ref_axis',(1.,0.,0.));
#29969=DIRECTION('',(0.000174853042027504,0.707106750910439,0.707106789843866));
#29970=DIRECTION('center_axis',(0.,-1.,0.));
#29971=DIRECTION('ref_axis',(1.,0.,0.));
#29972=DIRECTION('center_axis',(0.,-1.,0.));
#29973=DIRECTION('ref_axis',(1.,0.,0.));
#29974=DIRECTION('',(0.,1.,0.));
#29975=DIRECTION('center_axis',(0.,-1.,0.));
#29976=DIRECTION('ref_axis',(1.,0.,0.));
#29977=DIRECTION('center_axis',(0.,-1.,0.));
#29978=DIRECTION('ref_axis',(0.,0.,-1.));
#29979=DIRECTION('center_axis',(-1.,0.,-1.55820775385987E-16));
#29980=DIRECTION('ref_axis',(-1.55820775385987E-16,0.,1.));
#29981=DIRECTION('center_axis',(0.,1.,0.));
#29982=DIRECTION('ref_axis',(0.,0.,-1.));
#29983=DIRECTION('center_axis',(0.,1.,0.));
#29984=DIRECTION('ref_axis',(0.,0.,-1.));
#29985=DIRECTION('center_axis',(0.,1.,0.));
#29986=DIRECTION('ref_axis',(0.,0.,-1.));
#29987=DIRECTION('center_axis',(0.,1.,0.));
#29988=DIRECTION('ref_axis',(0.,0.,-1.));
#29989=DIRECTION('center_axis',(0.,1.,0.));
#29990=DIRECTION('ref_axis',(0.,0.,-1.));
#29991=DIRECTION('center_axis',(0.,1.,0.));
#29992=DIRECTION('ref_axis',(0.,0.,-1.));
#29993=DIRECTION('center_axis',(0.,1.,0.));
#29994=DIRECTION('ref_axis',(0.,0.,-1.));
#29995=DIRECTION('center_axis',(-0.500000000000001,0.,0.866025403784438));
#29996=DIRECTION('ref_axis',(0.866025403784439,0.,0.499999999999999));
#29997=DIRECTION('',(0.500000000000001,0.,-0.866025403784438));
#29998=DIRECTION('center_axis',(0.500000000000001,0.,0.866025403784438));
#29999=DIRECTION('ref_axis',(0.866025403784437,0.,-0.500000000000002));
#30000=DIRECTION('',(-0.500000000000001,0.,-0.866025403784438));
#30001=DIRECTION('center_axis',(1.,0.,0.));
#30002=DIRECTION('ref_axis',(0.,0.,-1.));
#30003=DIRECTION('',(-1.,0.,0.));
#30004=DIRECTION('center_axis',(0.5,0.,-0.866025403784439));
#30005=DIRECTION('ref_axis',(-0.866025403784439,0.,-0.5));
#30006=DIRECTION('',(-0.5,0.,0.866025403784439));
#30007=DIRECTION('center_axis',(-0.500000000000001,0.,-0.866025403784438));
#30008=DIRECTION('ref_axis',(-0.866025403784437,0.,0.500000000000003));
#30009=DIRECTION('',(0.500000000000001,0.,0.866025403784438));
#30010=DIRECTION('center_axis',(-1.,0.,0.));
#30011=DIRECTION('ref_axis',(0.,0.,1.));
#30012=DIRECTION('',(1.,0.,0.));
#30013=DIRECTION('center_axis',(0.,1.,0.));
#30014=DIRECTION('ref_axis',(1.,0.,0.));
#30015=DIRECTION('',(-0.707106781186541,0.707106781186554,-8.65956056235486E-17));
#30016=DIRECTION('center_axis',(0.,-1.,0.));
#30017=DIRECTION('ref_axis',(1.,0.,0.));
#30018=DIRECTION('center_axis',(0.,1.,0.));
#30019=DIRECTION('ref_axis',(0.,0.,1.));
#30020=DIRECTION('center_axis',(0.,-1.,0.));
#30021=DIRECTION('ref_axis',(1.,0.,0.));
#30022=DIRECTION('center_axis',(0.,-1.,0.));
#30023=DIRECTION('ref_axis',(1.,0.,0.));
#30024=DIRECTION('',(0.707106781186548,0.707106781186548,8.65956056235493E-17));
#30025=DIRECTION('center_axis',(0.,1.,0.));
#30026=DIRECTION('ref_axis',(1.,0.,0.));
#30027=DIRECTION('center_axis',(0.,-1.,0.));
#30028=DIRECTION('ref_axis',(1.,0.,0.));
#30029=DIRECTION('',(-0.707106781186548,0.707106781186548,-8.65956056235493E-17));
#30030=DIRECTION('center_axis',(0.,-1.,0.));
#30031=DIRECTION('ref_axis',(0.,0.,-1.));
#30032=DIRECTION('center_axis',(0.,-1.,0.));
#30033=DIRECTION('ref_axis',(1.,0.,0.));
#30034=DIRECTION('center_axis',(0.,-1.,0.));
#30035=DIRECTION('ref_axis',(1.,0.,0.));
#30036=DIRECTION('',(0.707106781186547,0.707106781186547,8.65956056235493E-17));
#30037=DIRECTION('axis',(0.,0.,1.));
#30038=DIRECTION('refdir',(1.,0.,0.));
#30039=DIRECTION('center_axis',(0.,0.,1.));
#30040=DIRECTION('ref_axis',(1.,0.,0.));
#30041=DIRECTION('',(0.,0.,-1.));
#30042=DIRECTION('center_axis',(0.,0.,1.));
#30043=DIRECTION('ref_axis',(1.,0.,0.));
#30044=DIRECTION('center_axis',(0.,0.,1.));
#30045=DIRECTION('ref_axis',(1.,0.,0.));
#30046=DIRECTION('',(0.,0.,-1.));
#30047=DIRECTION('center_axis',(0.,0.,1.));
#30048=DIRECTION('ref_axis',(1.,0.,0.));
#30049=DIRECTION('',(0.,0.,-1.));
#30050=DIRECTION('center_axis',(0.,0.,1.));
#30051=DIRECTION('ref_axis',(1.,0.,0.));
#30052=DIRECTION('',(0.,0.,-1.));
#30053=DIRECTION('center_axis',(0.,0.,1.));
#30054=DIRECTION('ref_axis',(1.,0.,0.));
#30055=DIRECTION('',(0.,0.,-1.));
#30056=DIRECTION('center_axis',(0.,0.,1.));
#30057=DIRECTION('ref_axis',(1.,0.,0.));
#30058=DIRECTION('',(0.,0.,-1.));
#30059=DIRECTION('center_axis',(0.,0.,1.));
#30060=DIRECTION('ref_axis',(1.,0.,0.));
#30061=DIRECTION('',(0.,0.,-1.));
#30062=DIRECTION('center_axis',(0.,0.,1.));
#30063=DIRECTION('ref_axis',(-0.938278381435466,-0.345881018459878,0.));
#30064=DIRECTION('',(0.,0.,1.));
#30065=DIRECTION('center_axis',(0.,0.,1.));
#30066=DIRECTION('ref_axis',(1.,2.10412784742716E-14,0.));
#30067=DIRECTION('center_axis',(0.,0.,1.));
#30068=DIRECTION('ref_axis',(1.,2.10412784742716E-14,0.));
#30069=DIRECTION('',(0.,0.,1.));
#30070=DIRECTION('center_axis',(0.,0.,1.));
#30071=DIRECTION('ref_axis',(1.,2.10412784742716E-14,0.));
#30072=DIRECTION('center_axis',(0.,0.,1.));
#30073=DIRECTION('ref_axis',(1.,2.10412784742716E-14,0.));
#30074=DIRECTION('',(0.,0.,1.));
#30075=DIRECTION('center_axis',(0.,0.,1.));
#30076=DIRECTION('ref_axis',(1.,2.10412784742716E-14,0.));
#30077=DIRECTION('',(0.,0.,1.));
#30078=DIRECTION('center_axis',(0.,0.,1.));
#30079=DIRECTION('ref_axis',(1.,2.10412784742716E-14,0.));
#30080=DIRECTION('',(0.,0.,1.));
#30081=DIRECTION('center_axis',(0.,0.,1.));
#30082=DIRECTION('ref_axis',(1.,2.10412784742716E-14,0.));
#30083=DIRECTION('',(0.,0.,1.));
#30084=DIRECTION('center_axis',(0.,0.,1.));
#30085=DIRECTION('ref_axis',(1.,2.10412784742716E-14,0.));
#30086=DIRECTION('',(0.,0.,1.));
#30087=DIRECTION('center_axis',(0.,0.,1.));
#30088=DIRECTION('ref_axis',(1.,0.,0.));
#30089=DIRECTION('center_axis',(0.,0.,-1.));
#30090=DIRECTION('ref_axis',(1.,0.,0.));
#30091=DIRECTION('center_axis',(0.,0.,-1.));
#30092=DIRECTION('ref_axis',(1.,0.,0.));
#30093=DIRECTION('center_axis',(0.,0.,1.));
#30094=DIRECTION('ref_axis',(1.,0.,0.));
#30095=DIRECTION('center_axis',(0.,0.,1.));
#30096=DIRECTION('ref_axis',(1.,0.,0.));
#30097=DIRECTION('center_axis',(0.,0.,1.));
#30098=DIRECTION('ref_axis',(1.,0.,0.));
#30099=DIRECTION('center_axis',(0.,0.,-1.));
#30100=DIRECTION('ref_axis',(1.,2.10412784742716E-14,0.));
#30101=DIRECTION('center_axis',(0.,0.,1.));
#30102=DIRECTION('ref_axis',(0.88903119899841,0.457846619740114,0.));
#30103=DIRECTION('center_axis',(0.,0.,1.));
#30104=DIRECTION('ref_axis',(1.,0.,0.));
#30105=DIRECTION('',(-1.,1.92296268638356E-16,0.));
#30106=DIRECTION('center_axis',(0.,0.,1.));
#30107=DIRECTION('ref_axis',(1.,0.,0.));
#30108=DIRECTION('center_axis',(0.,0.,1.));
#30109=DIRECTION('ref_axis',(1.,0.,0.));
#30110=DIRECTION('',(-0.5,0.866025403784439,0.));
#30111=DIRECTION('center_axis',(0.,0.,1.));
#30112=DIRECTION('ref_axis',(1.,0.,0.));
#30113=DIRECTION('center_axis',(0.,0.,1.));
#30114=DIRECTION('ref_axis',(1.,0.,0.));
#30115=DIRECTION('',(0.5,0.866025403784438,0.));
#30116=DIRECTION('center_axis',(0.,0.,1.));
#30117=DIRECTION('ref_axis',(1.,0.,0.));
#30118=DIRECTION('center_axis',(0.,0.,1.));
#30119=DIRECTION('ref_axis',(1.,0.,0.));
#30120=DIRECTION('',(1.,-1.92296268638356E-16,0.));
#30121=DIRECTION('center_axis',(0.,0.,1.));
#30122=DIRECTION('ref_axis',(1.,0.,0.));
#30123=DIRECTION('center_axis',(0.,0.,1.));
#30124=DIRECTION('ref_axis',(1.,0.,0.));
#30125=DIRECTION('',(0.5,-0.866025403784439,0.));
#30126=DIRECTION('center_axis',(0.,0.,1.));
#30127=DIRECTION('ref_axis',(1.,0.,0.));
#30128=DIRECTION('center_axis',(0.,0.,1.));
#30129=DIRECTION('ref_axis',(1.,0.,0.));
#30130=DIRECTION('',(-0.5,-0.866025403784439,0.));
#30131=DIRECTION('center_axis',(0.,0.,1.));
#30132=DIRECTION('ref_axis',(1.,0.,0.));
#30133=DIRECTION('center_axis',(0.,0.,1.));
#30134=DIRECTION('ref_axis',(1.,0.,0.));
#30135=DIRECTION('',(-0.856837487509096,-1.04932328646748E-16,0.515586578567653));
#30136=DIRECTION('center_axis',(0.,0.,-1.));
#30137=DIRECTION('ref_axis',(1.,0.,0.));
#30138=DIRECTION('center_axis',(0.,0.,-1.));
#30139=DIRECTION('ref_axis',(1.,0.,0.));
#30140=DIRECTION('center_axis',(0.,0.,-1.));
#30141=DIRECTION('ref_axis',(1.,0.,0.));
#30142=DIRECTION('center_axis',(0.,0.,-1.));
#30143=DIRECTION('ref_axis',(1.,0.,0.));
#30144=DIRECTION('center_axis',(0.,0.,-1.));
#30145=DIRECTION('ref_axis',(1.,0.,0.));
#30146=DIRECTION('center_axis',(0.,0.,-1.));
#30147=DIRECTION('ref_axis',(1.,0.,0.));
#30148=DIRECTION('center_axis',(0.,0.,-1.));
#30149=DIRECTION('ref_axis',(1.,0.,0.));
#30150=DIRECTION('center_axis',(-0.866025403784438,0.5,0.));
#30151=DIRECTION('ref_axis',(0.5,0.866025403784438,0.));
#30152=DIRECTION('',(0.,0.,-1.));
#30153=DIRECTION('',(0.5,0.866025403784438,0.));
#30154=DIRECTION('',(0.,0.,-1.));
#30155=DIRECTION('center_axis',(-0.866025403784438,0.5,0.));
#30156=DIRECTION('ref_axis',(0.5,0.866025403784438,0.));
#30157=DIRECTION('',(0.,0.,-1.));
#30158=DIRECTION('',(0.5,0.866025403784438,0.));
#30159=DIRECTION('center_axis',(1.92296268638356E-16,1.,0.));
#30160=DIRECTION('ref_axis',(1.,-1.92296268638356E-16,0.));
#30161=DIRECTION('',(0.,0.,-1.));
#30162=DIRECTION('',(1.,-1.92296268638356E-16,0.));
#30163=DIRECTION('center_axis',(1.92296268638356E-16,1.,0.));
#30164=DIRECTION('ref_axis',(1.,-1.92296268638356E-16,0.));
#30165=DIRECTION('',(1.,-1.92296268638356E-16,0.));
#30166=DIRECTION('',(0.,0.,-1.));
#30167=DIRECTION('center_axis',(1.92296268638356E-16,1.,0.));
#30168=DIRECTION('ref_axis',(1.,-1.92296268638356E-16,0.));
#30169=DIRECTION('',(0.,0.,-1.));
#30170=DIRECTION('',(1.,-1.92296268638356E-16,0.));
#30171=DIRECTION('center_axis',(-0.866025403784439,-0.5,0.));
#30172=DIRECTION('ref_axis',(-0.5,0.866025403784439,0.));
#30173=DIRECTION('',(-0.5,0.866025403784439,0.));
#30174=DIRECTION('',(0.,0.,-1.));
#30175=DIRECTION('center_axis',(-0.866025403784439,-0.5,0.));
#30176=DIRECTION('ref_axis',(-0.5,0.866025403784439,0.));
#30177=DIRECTION('',(0.,0.,-1.));
#30178=DIRECTION('',(-0.5,0.866025403784439,0.));
#30179=DIRECTION('center_axis',(0.866025403784439,0.5,0.));
#30180=DIRECTION('ref_axis',(0.5,-0.866025403784439,0.));
#30181=DIRECTION('',(0.,0.,-1.));
#30182=DIRECTION('',(0.5,-0.866025403784439,0.));
#30183=DIRECTION('center_axis',(0.866025403784439,0.5,0.));
#30184=DIRECTION('ref_axis',(0.5,-0.866025403784439,0.));
#30185=DIRECTION('',(0.5,-0.866025403784439,0.));
#30186=DIRECTION('',(0.,0.,-1.));
#30187=DIRECTION('center_axis',(0.866025403784439,0.5,0.));
#30188=DIRECTION('ref_axis',(0.5,-0.866025403784439,0.));
#30189=DIRECTION('',(0.5,-0.866025403784439,0.));
#30190=DIRECTION('center_axis',(0.,0.,-1.));
#30191=DIRECTION('ref_axis',(-1.,0.,0.));
#30192=DIRECTION('',(0.5,0.866025403784438,0.));
#30193=DIRECTION('center_axis',(0.,0.,-1.));
#30194=DIRECTION('ref_axis',(-1.,0.,0.));
#30195=DIRECTION('center_axis',(0.,0.,-1.));
#30196=DIRECTION('ref_axis',(-1.,0.,0.));
#30197=DIRECTION('',(-0.5,-0.866025403784439,0.));
#30198=DIRECTION('center_axis',(0.,0.,-1.));
#30199=DIRECTION('ref_axis',(-1.,0.,0.));
#30200=DIRECTION('',(-1.,1.92296268638356E-16,0.));
#30201=DIRECTION('',(-0.5,-0.866025403784439,0.));
#30202=DIRECTION('center_axis',(0.,0.,-1.));
#30203=DIRECTION('ref_axis',(-1.,0.,0.));
#30204=DIRECTION('',(-1.,1.92296268638356E-16,0.));
#30205=DIRECTION('center_axis',(0.,0.,-1.));
#30206=DIRECTION('ref_axis',(-1.,0.,0.));
#30207=DIRECTION('',(-0.5,0.866025403784439,0.));
#30208=DIRECTION('center_axis',(0.866025403784439,-0.5,0.));
#30209=DIRECTION('ref_axis',(-0.5,-0.866025403784439,0.));
#30210=DIRECTION('',(0.,0.,-1.));
#30211=DIRECTION('',(-0.5,-0.866025403784439,0.));
#30212=DIRECTION('center_axis',(0.866025403784439,-0.5,0.));
#30213=DIRECTION('ref_axis',(-0.5,-0.866025403784439,0.));
#30214=DIRECTION('',(0.,0.,-1.));
#30215=DIRECTION('center_axis',(0.866025403784439,-0.5,0.));
#30216=DIRECTION('ref_axis',(-0.5,-0.866025403784439,0.));
#30217=DIRECTION('center_axis',(-1.92296268638356E-16,-1.,0.));
#30218=DIRECTION('ref_axis',(-1.,1.92296268638356E-16,0.));
#30219=DIRECTION('center_axis',(-1.92296268638356E-16,-1.,0.));
#30220=DIRECTION('ref_axis',(-1.,1.92296268638356E-16,0.));
#30221=DIRECTION('',(-1.,1.92296268638356E-16,0.));
#30222=DIRECTION('center_axis',(-0.866025403784438,0.5,0.));
#30223=DIRECTION('ref_axis',(0.5,0.866025403784438,0.));
#30224=DIRECTION('center_axis',(-0.866025403784439,-0.5,0.));
#30225=DIRECTION('ref_axis',(-0.5,0.866025403784439,0.));
#30226=DIRECTION('center_axis',(-1.92296268638356E-16,-1.,0.));
#30227=DIRECTION('ref_axis',(-1.,1.92296268638356E-16,0.));
#30228=DIRECTION('center_axis',(0.,0.,-1.));
#30229=DIRECTION('ref_axis',(-1.,0.,0.));
#30230=DIRECTION('center_axis',(0.,0.,1.));
#30231=DIRECTION('ref_axis',(1.,0.,0.));
#30232=DIRECTION('center_axis',(0.,0.,1.));
#30233=DIRECTION('ref_axis',(1.,0.,0.));
#30234=DIRECTION('',(0.707106781186548,8.65956056235493E-17,-0.707106781186547));
#30235=DIRECTION('center_axis',(0.,0.,1.));
#30236=DIRECTION('ref_axis',(0.266308421152316,-0.963887869424323,0.));
#30237=DIRECTION('center_axis',(0.,0.,-1.));
#30238=DIRECTION('ref_axis',(1.,0.,0.));
#30239=DIRECTION('center_axis',(0.,0.,-1.));
#30240=DIRECTION('ref_axis',(1.,0.,0.));
#30241=DIRECTION('center_axis',(0.,0.,1.));
#30242=DIRECTION('ref_axis',(1.,0.,0.));
#30243=DIRECTION('',(-0.707106781186548,-8.65956056235494E-17,-0.707106781186547));
#30244=DIRECTION('center_axis',(0.,0.,1.));
#30245=DIRECTION('ref_axis',(1.,0.,0.));
#30246=DIRECTION('axis',(0.,0.,1.));
#30247=DIRECTION('refdir',(1.,0.,0.));
#30248=DIRECTION('center_axis',(0.,0.,-1.));
#30249=DIRECTION('ref_axis',(0.,-1.,0.));
#30250=DIRECTION('',(0.,-1.,0.));
#30251=DIRECTION('',(-1.,0.,0.));
#30252=DIRECTION('',(0.,-1.,0.));
#30253=DIRECTION('',(-1.,0.,0.));
#30254=DIRECTION('center_axis',(0.,1.,0.));
#30255=DIRECTION('ref_axis',(0.,0.,-1.));
#30256=DIRECTION('',(0.,0.,-1.));
#30257=DIRECTION('',(-1.,0.,0.));
#30258=DIRECTION('',(0.,0.,-1.));
#30259=DIRECTION('center_axis',(0.,0.,1.));
#30260=DIRECTION('ref_axis',(0.,1.,0.));
#30261=DIRECTION('',(0.,1.,0.));
#30262=DIRECTION('',(-1.,0.,0.));
#30263=DIRECTION('',(0.,1.,0.));
#30264=DIRECTION('center_axis',(0.,-1.,0.));
#30265=DIRECTION('ref_axis',(0.,0.,1.));
#30266=DIRECTION('',(0.,0.,1.));
#30267=DIRECTION('',(0.,0.,1.));
#30268=DIRECTION('center_axis',(-1.,0.,0.));
#30269=DIRECTION('ref_axis',(0.,0.,1.));
#30270=DIRECTION('center_axis',(0.,0.,-1.));
#30271=DIRECTION('ref_axis',(0.,-1.,0.));
#30272=DIRECTION('',(0.,-1.,0.));
#30273=DIRECTION('',(-1.,0.,0.));
#30274=DIRECTION('',(0.,-1.,0.));
#30275=DIRECTION('',(-1.,0.,0.));
#30276=DIRECTION('center_axis',(0.,1.,0.));
#30277=DIRECTION('ref_axis',(0.,0.,-1.));
#30278=DIRECTION('',(0.,0.,-1.));
#30279=DIRECTION('',(-1.,0.,0.));
#30280=DIRECTION('',(0.,0.,-1.));
#30281=DIRECTION('center_axis',(0.,0.,1.));
#30282=DIRECTION('ref_axis',(0.,1.,0.));
#30283=DIRECTION('',(0.,1.,0.));
#30284=DIRECTION('',(-1.,0.,0.));
#30285=DIRECTION('',(0.,1.,0.));
#30286=DIRECTION('center_axis',(0.,-1.,0.));
#30287=DIRECTION('ref_axis',(0.,0.,1.));
#30288=DIRECTION('',(0.,0.,1.));
#30289=DIRECTION('',(0.,0.,1.));
#30290=DIRECTION('center_axis',(-1.,0.,0.));
#30291=DIRECTION('ref_axis',(0.,0.,1.));
#30292=DIRECTION('center_axis',(-0.577350269189615,-0.577350269189615,0.577350269189648));
#30293=DIRECTION('ref_axis',(0.707106781186568,0.,0.707106781186527));
#30294=DIRECTION('',(0.707106781186566,0.,0.707106781186529));
#30295=DIRECTION('',(-0.707106781186548,0.707106781186548,0.));
#30296=DIRECTION('',(0.,-0.707106781186568,-0.707106781186527));
#30297=DIRECTION('center_axis',(0.577350269189615,-0.577350269189615,0.577350269189648));
#30298=DIRECTION('ref_axis',(0.707106781186568,0.,-0.707106781186527));
#30299=DIRECTION('',(0.,0.707106781186568,0.707106781186527));
#30300=DIRECTION('',(-0.707106781186548,-0.707106781186548,0.));
#30301=DIRECTION('',(0.707106781186566,-3.14018491736764E-15,-0.707106781186529));
#30302=DIRECTION('center_axis',(-0.577350269189615,-0.577350269189612,-0.577350269189651));
#30303=DIRECTION('ref_axis',(-0.70710678118657,0.,0.707106781186525));
#30304=DIRECTION('',(0.707106781186548,-0.707106781186548,0.));
#30305=DIRECTION('',(-0.70710678118657,0.,0.707106781186526));
#30306=DIRECTION('',(6.28036983473528E-15,0.707106781186568,-0.707106781186527));
#30307=DIRECTION('center_axis',(-0.577350269189615,0.577350269189615,0.577350269189648));
#30308=DIRECTION('ref_axis',(0.707106781186568,0.,0.707106781186527));
#30309=DIRECTION('',(0.,-0.707106781186568,0.707106781186527));
#30310=DIRECTION('',(0.707106781186548,0.707106781186548,0.));
#30311=DIRECTION('',(-0.707106781186566,3.14018491736764E-15,-0.707106781186529));
#30312=DIRECTION('center_axis',(0.577350269189613,-0.577350269189613,-0.577350269189651));
#30313=DIRECTION('ref_axis',(-0.707106781186571,0.,-0.707106781186524));
#30314=DIRECTION('',(0.707106781186548,0.707106781186548,0.));
#30315=DIRECTION('',(6.28036983473528E-15,-0.707106781186568,0.707106781186527));
#30316=DIRECTION('',(-0.70710678118657,3.14018491736763E-15,-0.707106781186526));
#30317=DIRECTION('center_axis',(0.,-0.707106781186527,-0.707106781186568));
#30318=DIRECTION('ref_axis',(-1.,0.,0.));
#30319=DIRECTION('',(-1.,0.,0.));
#30320=DIRECTION('',(1.,0.,0.));
#30321=DIRECTION('center_axis',(0.577350269189615,0.577350269189615,0.577350269189648));
#30322=DIRECTION('ref_axis',(0.707106781186568,0.,-0.707106781186527));
#30323=DIRECTION('',(-0.707106781186566,0.,0.707106781186529));
#30324=DIRECTION('',(0.707106781186548,-0.707106781186548,0.));
#30325=DIRECTION('',(0.,0.707106781186568,-0.707106781186527));
#30326=DIRECTION('center_axis',(-0.577350269189613,0.577350269189613,-0.577350269189651));
#30327=DIRECTION('ref_axis',(-0.707106781186571,0.,0.707106781186524));
#30328=DIRECTION('',(-6.28036983473528E-15,0.707106781186568,0.707106781186527));
#30329=DIRECTION('',(0.70710678118657,-3.14018491736763E-15,-0.707106781186526));
#30330=DIRECTION('',(-0.707106781186548,-0.707106781186548,0.));
#30331=DIRECTION('center_axis',(-0.707106781186526,0.,-0.70710678118657));
#30332=DIRECTION('ref_axis',(-0.70710678118657,0.,0.707106781186526));
#30333=DIRECTION('',(0.,1.,0.));
#30334=DIRECTION('',(0.,-1.,0.));
#30335=DIRECTION('center_axis',(-0.707106781186548,0.707106781186548,0.));
#30336=DIRECTION('ref_axis',(0.,0.,1.));
#30337=DIRECTION('',(0.,0.,-1.));
#30338=DIRECTION('',(0.,0.,1.));
#30339=DIRECTION('center_axis',(0.577350269189615,0.577350269189612,-0.577350269189651));
#30340=DIRECTION('ref_axis',(-0.70710678118657,0.,-0.707106781186525));
#30341=DIRECTION('',(-0.707106781186548,0.707106781186548,0.));
#30342=DIRECTION('',(0.70710678118657,0.,0.707106781186526));
#30343=DIRECTION('',(-6.28036983473528E-15,-0.707106781186568,-0.707106781186527));
#30344=DIRECTION('center_axis',(0.707106781186526,0.,-0.70710678118657));
#30345=DIRECTION('ref_axis',(-0.70710678118657,0.,-0.707106781186526));
#30346=DIRECTION('',(0.,-1.,0.));
#30347=DIRECTION('',(0.,1.,0.));
#30348=DIRECTION('center_axis',(0.,0.707106781186527,-0.707106781186568));
#30349=DIRECTION('ref_axis',(-1.,0.,0.));
#30350=DIRECTION('',(1.,0.,0.));
#30351=DIRECTION('',(-1.,0.,0.));
#30352=DIRECTION('center_axis',(0.707106781186548,0.707106781186548,0.));
#30353=DIRECTION('ref_axis',(0.,0.,-1.));
#30354=DIRECTION('',(0.,0.,-1.));
#30355=DIRECTION('',(0.,0.,1.));
#30356=DIRECTION('center_axis',(0.,0.707106781186527,0.707106781186568));
#30357=DIRECTION('ref_axis',(1.,0.,0.));
#30358=DIRECTION('',(1.,0.,0.));
#30359=DIRECTION('',(-1.,0.,0.));
#30360=DIRECTION('center_axis',(0.707106781186529,0.,0.707106781186566));
#30361=DIRECTION('ref_axis',(0.707106781186566,0.,-0.707106781186529));
#30362=DIRECTION('',(0.,-1.,0.));
#30363=DIRECTION('',(0.,1.,0.));
#30364=DIRECTION('center_axis',(0.707106781186548,-0.707106781186548,0.));
#30365=DIRECTION('ref_axis',(0.,0.,-1.));
#30366=DIRECTION('',(0.,0.,-1.));
#30367=DIRECTION('',(0.,0.,1.));
#30368=DIRECTION('center_axis',(-0.707106781186529,0.,0.707106781186566));
#30369=DIRECTION('ref_axis',(0.707106781186566,0.,0.707106781186529));
#30370=DIRECTION('',(0.,1.,0.));
#30371=DIRECTION('',(0.,-1.,0.));
#30372=DIRECTION('center_axis',(-0.707106781186548,-0.707106781186548,0.));
#30373=DIRECTION('ref_axis',(0.,0.,1.));
#30374=DIRECTION('',(0.,0.,-1.));
#30375=DIRECTION('',(0.,0.,1.));
#30376=DIRECTION('center_axis',(0.,-0.707106781186527,0.707106781186568));
#30377=DIRECTION('ref_axis',(1.,0.,0.));
#30378=DIRECTION('',(-1.,0.,0.));
#30379=DIRECTION('',(1.,0.,0.));
#30380=DIRECTION('center_axis',(0.,-1.,0.));
#30381=DIRECTION('ref_axis',(1.,0.,0.));
#30382=DIRECTION('center_axis',(0.,0.,1.));
#30383=DIRECTION('ref_axis',(1.,0.,0.));
#30384=DIRECTION('center_axis',(-1.,0.,0.));
#30385=DIRECTION('ref_axis',(0.,-1.,0.));
#30386=DIRECTION('center_axis',(0.,1.,0.));
#30387=DIRECTION('ref_axis',(-1.,0.,0.));
#30388=DIRECTION('center_axis',(1.,0.,0.));
#30389=DIRECTION('ref_axis',(0.,1.,0.));
#30390=DIRECTION('center_axis',(0.,0.,1.));
#30391=DIRECTION('ref_axis',(1.,0.,0.));
#30392=DIRECTION('axis',(0.,0.,1.));
#30393=DIRECTION('refdir',(1.,0.,0.));
#30394=DIRECTION('center_axis',(0.,0.,1.));
#30395=DIRECTION('ref_axis',(1.,0.,0.));
#30396=DIRECTION('',(0.,0.,-1.));
#30397=DIRECTION('center_axis',(0.,0.,1.));
#30398=DIRECTION('ref_axis',(1.,0.,0.));
#30399=DIRECTION('center_axis',(0.,0.,1.));
#30400=DIRECTION('ref_axis',(1.,0.,0.));
#30401=DIRECTION('',(0.,0.,-1.));
#30402=DIRECTION('center_axis',(0.,0.,1.));
#30403=DIRECTION('ref_axis',(1.,0.,0.));
#30404=DIRECTION('',(0.,0.,-1.));
#30405=DIRECTION('center_axis',(0.,0.,1.));
#30406=DIRECTION('ref_axis',(1.,0.,0.));
#30407=DIRECTION('',(0.,0.,-1.));
#30408=DIRECTION('center_axis',(0.,0.,1.));
#30409=DIRECTION('ref_axis',(1.,0.,0.));
#30410=DIRECTION('',(0.,0.,-1.));
#30411=DIRECTION('center_axis',(0.,0.,1.));
#30412=DIRECTION('ref_axis',(1.,0.,0.));
#30413=DIRECTION('',(0.,0.,-1.));
#30414=DIRECTION('center_axis',(0.,0.,1.));
#30415=DIRECTION('ref_axis',(1.,0.,0.));
#30416=DIRECTION('',(0.,0.,-1.));
#30417=DIRECTION('center_axis',(0.,0.,1.));
#30418=DIRECTION('ref_axis',(1.,0.,0.));
#30419=DIRECTION('',(0.,0.,-1.));
#30420=DIRECTION('center_axis',(0.,0.,1.));
#30421=DIRECTION('ref_axis',(1.,0.,0.));
#30422=DIRECTION('',(0.,0.,-1.));
#30423=DIRECTION('center_axis',(0.,0.,1.));
#30424=DIRECTION('ref_axis',(1.,0.,0.));
#30425=DIRECTION('',(0.,0.,-1.));
#30426=DIRECTION('center_axis',(0.,0.,1.));
#30427=DIRECTION('ref_axis',(1.,0.,0.));
#30428=DIRECTION('',(0.,0.,-1.));
#30429=DIRECTION('center_axis',(0.,0.,1.));
#30430=DIRECTION('ref_axis',(1.,0.,0.));
#30431=DIRECTION('',(0.,0.,-1.));
#30432=DIRECTION('center_axis',(0.,0.,1.));
#30433=DIRECTION('ref_axis',(1.,0.,0.));
#30434=DIRECTION('',(0.,0.,-1.));
#30435=DIRECTION('center_axis',(0.,0.,1.));
#30436=DIRECTION('ref_axis',(1.,0.,0.));
#30437=DIRECTION('',(0.,0.,-1.));
#30438=DIRECTION('center_axis',(0.,0.,1.));
#30439=DIRECTION('ref_axis',(1.,0.,0.));
#30440=DIRECTION('',(0.,0.,-1.));
#30441=DIRECTION('center_axis',(0.,0.,1.));
#30442=DIRECTION('ref_axis',(1.,0.,0.));
#30443=DIRECTION('',(0.,0.,-1.));
#30444=DIRECTION('center_axis',(0.,0.,1.));
#30445=DIRECTION('ref_axis',(1.,0.,0.));
#30446=DIRECTION('',(0.,0.,-1.));
#30447=DIRECTION('center_axis',(0.,0.,1.));
#30448=DIRECTION('ref_axis',(1.,0.,0.));
#30449=DIRECTION('',(0.,0.,-1.));
#30450=DIRECTION('center_axis',(0.,0.,1.));
#30451=DIRECTION('ref_axis',(1.,0.,0.));
#30452=DIRECTION('',(0.,0.,-1.));
#30453=DIRECTION('center_axis',(0.,0.,1.));
#30454=DIRECTION('ref_axis',(1.,0.,0.));
#30455=DIRECTION('',(0.,0.,-1.));
#30456=DIRECTION('center_axis',(0.,0.,1.));
#30457=DIRECTION('ref_axis',(1.,0.,0.));
#30458=DIRECTION('',(0.,0.,-1.));
#30459=DIRECTION('center_axis',(0.,0.,1.));
#30460=DIRECTION('ref_axis',(1.,0.,0.));
#30461=DIRECTION('',(0.,0.,-1.));
#30462=DIRECTION('center_axis',(0.,0.,1.));
#30463=DIRECTION('ref_axis',(1.,0.,0.));
#30464=DIRECTION('',(0.,0.,-1.));
#30465=DIRECTION('center_axis',(0.,0.,1.));
#30466=DIRECTION('ref_axis',(1.,0.,0.));
#30467=DIRECTION('',(0.,0.,-1.));
#30468=DIRECTION('center_axis',(0.,0.,1.));
#30469=DIRECTION('ref_axis',(1.,0.,0.));
#30470=DIRECTION('',(0.,0.,-1.));
#30471=DIRECTION('center_axis',(0.,0.,1.));
#30472=DIRECTION('ref_axis',(1.,0.,0.));
#30473=DIRECTION('',(0.,0.,-1.));
#30474=DIRECTION('center_axis',(0.,0.,1.));
#30475=DIRECTION('ref_axis',(1.,0.,0.));
#30476=DIRECTION('',(0.,0.,-1.));
#30477=DIRECTION('center_axis',(0.,0.,1.));
#30478=DIRECTION('ref_axis',(1.,0.,0.));
#30479=DIRECTION('',(0.,0.,-1.));
#30480=DIRECTION('center_axis',(0.,0.,1.));
#30481=DIRECTION('ref_axis',(1.,0.,0.));
#30482=DIRECTION('',(0.,0.,-1.));
#30483=DIRECTION('center_axis',(0.,0.,1.));
#30484=DIRECTION('ref_axis',(-0.993035081806481,-0.11781904048835,0.));
#30485=DIRECTION('',(0.,0.,1.));
#30486=DIRECTION('center_axis',(0.,0.,1.));
#30487=DIRECTION('ref_axis',(1.,-1.07699989592456E-13,0.));
#30488=DIRECTION('center_axis',(0.,0.,1.));
#30489=DIRECTION('ref_axis',(1.,-1.07699989592456E-13,0.));
#30490=DIRECTION('',(0.,0.,1.));
#30491=DIRECTION('center_axis',(0.,0.,1.));
#30492=DIRECTION('ref_axis',(1.,-1.07699989592456E-13,0.));
#30493=DIRECTION('center_axis',(0.,0.,1.));
#30494=DIRECTION('ref_axis',(1.,-1.07699989592456E-13,0.));
#30495=DIRECTION('',(0.,0.,1.));
#30496=DIRECTION('center_axis',(0.,0.,1.));
#30497=DIRECTION('ref_axis',(1.,-1.07699989592456E-13,0.));
#30498=DIRECTION('',(0.,0.,1.));
#30499=DIRECTION('center_axis',(0.,0.,1.));
#30500=DIRECTION('ref_axis',(1.,-1.07699989592456E-13,0.));
#30501=DIRECTION('',(0.,0.,1.));
#30502=DIRECTION('center_axis',(0.,0.,1.));
#30503=DIRECTION('ref_axis',(1.,-1.07699989592456E-13,0.));
#30504=DIRECTION('',(0.,0.,1.));
#30505=DIRECTION('center_axis',(0.,0.,1.));
#30506=DIRECTION('ref_axis',(1.,-1.07699989592456E-13,0.));
#30507=DIRECTION('',(0.,0.,1.));
#30508=DIRECTION('center_axis',(0.,0.,1.));
#30509=DIRECTION('ref_axis',(1.,-1.07699989592456E-13,0.));
#30510=DIRECTION('',(0.,0.,1.));
#30511=DIRECTION('center_axis',(0.,0.,1.));
#30512=DIRECTION('ref_axis',(1.,-1.07699989592456E-13,0.));
#30513=DIRECTION('',(0.,0.,1.));
#30514=DIRECTION('center_axis',(0.,0.,1.));
#30515=DIRECTION('ref_axis',(1.,-1.07699989592456E-13,0.));
#30516=DIRECTION('',(0.,0.,1.));
#30517=DIRECTION('center_axis',(0.,0.,1.));
#30518=DIRECTION('ref_axis',(1.,-1.07699989592456E-13,0.));
#30519=DIRECTION('',(0.,0.,1.));
#30520=DIRECTION('center_axis',(0.,0.,1.));
#30521=DIRECTION('ref_axis',(1.,-1.07699989592456E-13,0.));
#30522=DIRECTION('',(0.,0.,1.));
#30523=DIRECTION('center_axis',(0.,0.,1.));
#30524=DIRECTION('ref_axis',(1.,-1.07699989592456E-13,0.));
#30525=DIRECTION('',(0.,0.,1.));
#30526=DIRECTION('center_axis',(0.,0.,1.));
#30527=DIRECTION('ref_axis',(1.,-1.07699989592456E-13,0.));
#30528=DIRECTION('',(0.,0.,1.));
#30529=DIRECTION('center_axis',(0.,0.,1.));
#30530=DIRECTION('ref_axis',(1.,-1.07699989592456E-13,0.));
#30531=DIRECTION('',(0.,0.,1.));
#30532=DIRECTION('center_axis',(0.,0.,1.));
#30533=DIRECTION('ref_axis',(1.,-1.07699989592456E-13,0.));
#30534=DIRECTION('',(0.,0.,1.));
#30535=DIRECTION('center_axis',(0.,0.,1.));
#30536=DIRECTION('ref_axis',(1.,-1.07699989592456E-13,0.));
#30537=DIRECTION('',(0.,0.,1.));
#30538=DIRECTION('center_axis',(0.,0.,1.));
#30539=DIRECTION('ref_axis',(1.,-1.07699989592456E-13,0.));
#30540=DIRECTION('',(0.,0.,1.));
#30541=DIRECTION('center_axis',(0.,0.,1.));
#30542=DIRECTION('ref_axis',(1.,-1.07699989592456E-13,0.));
#30543=DIRECTION('',(0.,0.,1.));
#30544=DIRECTION('center_axis',(0.,0.,1.));
#30545=DIRECTION('ref_axis',(1.,-1.07699989592456E-13,0.));
#30546=DIRECTION('',(0.,0.,1.));
#30547=DIRECTION('center_axis',(0.,0.,1.));
#30548=DIRECTION('ref_axis',(1.,-1.07699989592456E-13,0.));
#30549=DIRECTION('',(0.,0.,1.));
#30550=DIRECTION('center_axis',(0.,0.,1.));
#30551=DIRECTION('ref_axis',(1.,-1.07699989592456E-13,0.));
#30552=DIRECTION('',(0.,0.,1.));
#30553=DIRECTION('center_axis',(0.,0.,1.));
#30554=DIRECTION('ref_axis',(1.,-1.07699989592456E-13,0.));
#30555=DIRECTION('',(0.,0.,1.));
#30556=DIRECTION('center_axis',(0.,0.,1.));
#30557=DIRECTION('ref_axis',(1.,-1.07699989592456E-13,0.));
#30558=DIRECTION('',(0.,0.,1.));
#30559=DIRECTION('center_axis',(0.,0.,1.));
#30560=DIRECTION('ref_axis',(1.,-1.07699989592456E-13,0.));
#30561=DIRECTION('',(0.,0.,1.));
#30562=DIRECTION('center_axis',(0.,0.,1.));
#30563=DIRECTION('ref_axis',(1.,-1.07699989592456E-13,0.));
#30564=DIRECTION('',(0.,0.,1.));
#30565=DIRECTION('center_axis',(0.,0.,1.));
#30566=DIRECTION('ref_axis',(1.,-1.07699989592456E-13,0.));
#30567=DIRECTION('',(0.,0.,1.));
#30568=DIRECTION('center_axis',(0.,0.,1.));
#30569=DIRECTION('ref_axis',(1.,-1.07699989592456E-13,0.));
#30570=DIRECTION('',(0.,0.,1.));
#30571=DIRECTION('center_axis',(0.,0.,1.));
#30572=DIRECTION('ref_axis',(1.,-1.07699989592456E-13,0.));
#30573=DIRECTION('',(0.,0.,1.));
#30574=DIRECTION('center_axis',(0.,0.,1.));
#30575=DIRECTION('ref_axis',(1.,0.,0.));
#30576=DIRECTION('center_axis',(0.,0.,-1.));
#30577=DIRECTION('ref_axis',(1.,0.,0.));
#30578=DIRECTION('center_axis',(0.,0.,-1.));
#30579=DIRECTION('ref_axis',(1.,0.,0.));
#30580=DIRECTION('center_axis',(0.,0.,1.));
#30581=DIRECTION('ref_axis',(1.,0.,0.));
#30582=DIRECTION('center_axis',(0.,0.,1.));
#30583=DIRECTION('ref_axis',(1.,0.,0.));
#30584=DIRECTION('center_axis',(0.,0.,1.));
#30585=DIRECTION('ref_axis',(1.,0.,0.));
#30586=DIRECTION('center_axis',(0.,0.,-1.));
#30587=DIRECTION('ref_axis',(1.,-1.07699989592456E-13,0.));
#30588=DIRECTION('center_axis',(0.,0.,1.));
#30589=DIRECTION('ref_axis',(0.888987032667973,0.457932370277743,0.));
#30590=DIRECTION('center_axis',(0.,0.,1.));
#30591=DIRECTION('ref_axis',(1.,0.,0.));
#30592=DIRECTION('',(-1.,2.40370335797945E-16,0.));
#30593=DIRECTION('center_axis',(0.,0.,1.));
#30594=DIRECTION('ref_axis',(1.,0.,0.));
#30595=DIRECTION('center_axis',(0.,0.,1.));
#30596=DIRECTION('ref_axis',(1.,0.,0.));
#30597=DIRECTION('',(-0.5,0.866025403784439,0.));
#30598=DIRECTION('center_axis',(0.,0.,1.));
#30599=DIRECTION('ref_axis',(1.,0.,0.));
#30600=DIRECTION('center_axis',(0.,0.,1.));
#30601=DIRECTION('ref_axis',(1.,0.,0.));
#30602=DIRECTION('',(0.5,0.866025403784439,0.));
#30603=DIRECTION('center_axis',(0.,0.,1.));
#30604=DIRECTION('ref_axis',(1.,0.,0.));
#30605=DIRECTION('center_axis',(0.,0.,1.));
#30606=DIRECTION('ref_axis',(1.,0.,0.));
#30607=DIRECTION('',(1.,-1.20185167898973E-16,0.));
#30608=DIRECTION('center_axis',(0.,0.,1.));
#30609=DIRECTION('ref_axis',(1.,0.,0.));
#30610=DIRECTION('center_axis',(0.,0.,1.));
#30611=DIRECTION('ref_axis',(1.,0.,0.));
#30612=DIRECTION('',(0.5,-0.866025403784439,0.));
#30613=DIRECTION('center_axis',(0.,0.,1.));
#30614=DIRECTION('ref_axis',(1.,0.,0.));
#30615=DIRECTION('center_axis',(0.,0.,1.));
#30616=DIRECTION('ref_axis',(1.,0.,0.));
#30617=DIRECTION('',(-0.5,-0.866025403784439,0.));
#30618=DIRECTION('center_axis',(0.,0.,1.));
#30619=DIRECTION('ref_axis',(1.,0.,0.));
#30620=DIRECTION('center_axis',(0.,0.,1.));
#30621=DIRECTION('ref_axis',(1.,0.,0.));
#30622=DIRECTION('',(-0.856673567959776,-1.04912254291608E-16,0.515858893457375));
#30623=DIRECTION('center_axis',(0.,0.,-1.));
#30624=DIRECTION('ref_axis',(1.,0.,0.));
#30625=DIRECTION('center_axis',(0.,0.,-1.));
#30626=DIRECTION('ref_axis',(1.,0.,0.));
#30627=DIRECTION('center_axis',(0.,0.,-1.));
#30628=DIRECTION('ref_axis',(1.,0.,0.));
#30629=DIRECTION('center_axis',(0.,0.,-1.));
#30630=DIRECTION('ref_axis',(1.,0.,0.));
#30631=DIRECTION('center_axis',(0.,0.,-1.));
#30632=DIRECTION('ref_axis',(1.,0.,0.));
#30633=DIRECTION('center_axis',(0.,0.,-1.));
#30634=DIRECTION('ref_axis',(1.,0.,0.));
#30635=DIRECTION('center_axis',(0.,0.,-1.));
#30636=DIRECTION('ref_axis',(1.,0.,0.));
#30637=DIRECTION('center_axis',(-0.866025403784439,0.5,0.));
#30638=DIRECTION('ref_axis',(0.5,0.866025403784439,0.));
#30639=DIRECTION('',(0.,0.,-1.));
#30640=DIRECTION('',(0.5,0.866025403784439,0.));
#30641=DIRECTION('',(0.,0.,-1.));
#30642=DIRECTION('center_axis',(-0.866025403784439,0.5,0.));
#30643=DIRECTION('ref_axis',(0.5,0.866025403784439,0.));
#30644=DIRECTION('',(0.,0.,-1.));
#30645=DIRECTION('',(0.5,0.866025403784439,0.));
#30646=DIRECTION('center_axis',(1.20185167898973E-16,1.,0.));
#30647=DIRECTION('ref_axis',(1.,-1.20185167898973E-16,0.));
#30648=DIRECTION('',(0.,0.,-1.));
#30649=DIRECTION('',(1.,-1.20185167898973E-16,0.));
#30650=DIRECTION('center_axis',(1.20185167898973E-16,1.,0.));
#30651=DIRECTION('ref_axis',(1.,-1.20185167898973E-16,0.));
#30652=DIRECTION('',(1.,-1.20185167898973E-16,0.));
#30653=DIRECTION('',(0.,0.,-1.));
#30654=DIRECTION('center_axis',(1.20185167898973E-16,1.,0.));
#30655=DIRECTION('ref_axis',(1.,-1.20185167898973E-16,0.));
#30656=DIRECTION('',(0.,0.,-1.));
#30657=DIRECTION('',(1.,-1.20185167898973E-16,0.));
#30658=DIRECTION('center_axis',(-0.866025403784439,-0.5,0.));
#30659=DIRECTION('ref_axis',(-0.5,0.866025403784439,0.));
#30660=DIRECTION('',(-0.5,0.866025403784439,0.));
#30661=DIRECTION('',(0.,0.,-1.));
#30662=DIRECTION('center_axis',(-0.866025403784439,-0.5,0.));
#30663=DIRECTION('ref_axis',(-0.5,0.866025403784439,0.));
#30664=DIRECTION('',(0.,0.,-1.));
#30665=DIRECTION('',(-0.5,0.866025403784439,0.));
#30666=DIRECTION('center_axis',(0.866025403784439,0.5,0.));
#30667=DIRECTION('ref_axis',(0.5,-0.866025403784439,0.));
#30668=DIRECTION('',(0.,0.,-1.));
#30669=DIRECTION('',(0.5,-0.866025403784439,0.));
#30670=DIRECTION('center_axis',(0.866025403784439,0.5,0.));
#30671=DIRECTION('ref_axis',(0.5,-0.866025403784439,0.));
#30672=DIRECTION('',(0.5,-0.866025403784439,0.));
#30673=DIRECTION('',(0.,0.,-1.));
#30674=DIRECTION('center_axis',(0.866025403784439,0.5,0.));
#30675=DIRECTION('ref_axis',(0.5,-0.866025403784439,0.));
#30676=DIRECTION('',(0.5,-0.866025403784439,0.));
#30677=DIRECTION('center_axis',(0.,0.,-1.));
#30678=DIRECTION('ref_axis',(-1.,0.,0.));
#30679=DIRECTION('',(0.5,0.866025403784439,0.));
#30680=DIRECTION('center_axis',(0.,0.,-1.));
#30681=DIRECTION('ref_axis',(-1.,0.,0.));
#30682=DIRECTION('center_axis',(0.,0.,-1.));
#30683=DIRECTION('ref_axis',(-1.,0.,0.));
#30684=DIRECTION('',(-0.5,-0.866025403784439,0.));
#30685=DIRECTION('center_axis',(0.,0.,-1.));
#30686=DIRECTION('ref_axis',(-1.,0.,0.));
#30687=DIRECTION('',(-1.,2.40370335797945E-16,0.));
#30688=DIRECTION('',(-0.5,-0.866025403784439,0.));
#30689=DIRECTION('center_axis',(0.,0.,-1.));
#30690=DIRECTION('ref_axis',(-1.,0.,0.));
#30691=DIRECTION('',(-1.,2.40370335797945E-16,0.));
#30692=DIRECTION('center_axis',(0.,0.,-1.));
#30693=DIRECTION('ref_axis',(-1.,0.,0.));
#30694=DIRECTION('',(-0.5,0.866025403784439,0.));
#30695=DIRECTION('center_axis',(0.866025403784439,-0.5,0.));
#30696=DIRECTION('ref_axis',(-0.5,-0.866025403784439,0.));
#30697=DIRECTION('',(0.,0.,-1.));
#30698=DIRECTION('',(-0.5,-0.866025403784439,0.));
#30699=DIRECTION('center_axis',(0.866025403784439,-0.5,0.));
#30700=DIRECTION('ref_axis',(-0.5,-0.866025403784439,0.));
#30701=DIRECTION('',(0.,0.,-1.));
#30702=DIRECTION('center_axis',(0.866025403784439,-0.5,0.));
#30703=DIRECTION('ref_axis',(-0.5,-0.866025403784439,0.));
#30704=DIRECTION('center_axis',(-2.40370335797945E-16,-1.,0.));
#30705=DIRECTION('ref_axis',(-1.,2.40370335797945E-16,0.));
#30706=DIRECTION('center_axis',(-2.40370335797945E-16,-1.,0.));
#30707=DIRECTION('ref_axis',(-1.,2.40370335797945E-16,0.));
#30708=DIRECTION('',(-1.,2.40370335797945E-16,0.));
#30709=DIRECTION('center_axis',(-0.866025403784439,0.5,0.));
#30710=DIRECTION('ref_axis',(0.5,0.866025403784439,0.));
#30711=DIRECTION('center_axis',(-0.866025403784439,-0.5,0.));
#30712=DIRECTION('ref_axis',(-0.5,0.866025403784439,0.));
#30713=DIRECTION('center_axis',(-2.40370335797945E-16,-1.,0.));
#30714=DIRECTION('ref_axis',(-1.,2.40370335797945E-16,0.));
#30715=DIRECTION('center_axis',(0.,0.,-1.));
#30716=DIRECTION('ref_axis',(-1.,0.,0.));
#30717=DIRECTION('center_axis',(0.,0.,1.));
#30718=DIRECTION('ref_axis',(1.,0.,0.));
#30719=DIRECTION('center_axis',(0.,0.,1.));
#30720=DIRECTION('ref_axis',(1.,0.,0.));
#30721=DIRECTION('',(0.707106781186547,8.65956056235493E-17,-0.707106781186548));
#30722=DIRECTION('center_axis',(0.,0.,1.));
#30723=DIRECTION('ref_axis',(0.0319324370611075,-0.999490029696814,0.));
#30724=DIRECTION('center_axis',(0.,0.,-1.));
#30725=DIRECTION('ref_axis',(1.,0.,0.));
#30726=DIRECTION('center_axis',(0.,0.,-1.));
#30727=DIRECTION('ref_axis',(1.,0.,0.));
#30728=DIRECTION('center_axis',(0.,0.,1.));
#30729=DIRECTION('ref_axis',(1.,0.,0.));
#30730=DIRECTION('',(-0.707106781186548,-8.65956056235494E-17,-0.707106781186547));
#30731=DIRECTION('center_axis',(0.,0.,1.));
#30732=DIRECTION('ref_axis',(1.,0.,0.));
#30733=DIRECTION('axis',(0.,0.,1.));
#30734=DIRECTION('refdir',(1.,0.,0.));
#30735=DIRECTION('center_axis',(0.,0.,-1.));
#30736=DIRECTION('ref_axis',(1.,0.,0.));
#30737=DIRECTION('center_axis',(0.,0.,1.));
#30738=DIRECTION('ref_axis',(1.,0.,0.));
#30739=DIRECTION('',(-0.707106781186547,-8.65956056235493E-17,-0.707106781186548));
#30740=DIRECTION('center_axis',(0.,0.,-1.));
#30741=DIRECTION('ref_axis',(1.,0.,0.));
#30742=DIRECTION('center_axis',(0.,0.,1.));
#30743=DIRECTION('ref_axis',(1.,0.,0.));
#30744=DIRECTION('center_axis',(0.,0.,-1.));
#30745=DIRECTION('ref_axis',(1.,0.,0.));
#30746=DIRECTION('',(0.,0.,-1.));
#30747=DIRECTION('center_axis',(0.,0.,1.));
#30748=DIRECTION('ref_axis',(1.,0.,0.));
#30749=DIRECTION('center_axis',(0.,0.,-1.));
#30750=DIRECTION('ref_axis',(1.,0.,0.));
#30751=DIRECTION('center_axis',(0.,0.,1.));
#30752=DIRECTION('ref_axis',(1.,0.,0.));
#30753=DIRECTION('center_axis',(0.,0.,1.));
#30754=DIRECTION('ref_axis',(1.,0.,0.));
#30755=DIRECTION('',(0.707106781186547,8.65956056235493E-17,-0.707106781186548));
#30756=DIRECTION('center_axis',(0.,0.,1.));
#30757=DIRECTION('ref_axis',(1.,0.,0.));
#30758=DIRECTION('center_axis',(0.,0.,1.));
#30759=DIRECTION('ref_axis',(1.,0.,0.));
#30760=DIRECTION('center_axis',(0.,0.,1.));
#30761=DIRECTION('ref_axis',(1.,0.,0.));
#30762=DIRECTION('',(-0.866025403784439,-1.06057523872491E-16,0.5));
#30763=DIRECTION('center_axis',(0.5,-0.866025403784439,0.));
#30764=DIRECTION('ref_axis',(0.866025403784439,0.5,0.));
#30765=DIRECTION('',(0.,0.,1.));
#30766=DIRECTION('',(0.,0.,1.));
#30767=DIRECTION('center_axis',(1.,-3.20493781063927E-16,0.));
#30768=DIRECTION('ref_axis',(3.20493781063927E-16,1.,0.));
#30769=DIRECTION('',(0.,0.,1.));
#30770=DIRECTION('center_axis',(0.5,0.866025403784439,0.));
#30771=DIRECTION('ref_axis',(-0.866025403784439,0.5,0.));
#30772=DIRECTION('',(0.,0.,1.));
#30773=DIRECTION('center_axis',(0.,0.,-1.));
#30774=DIRECTION('ref_axis',(1.,0.,0.));
#30775=DIRECTION('',(0.866025403784439,1.06057523872491E-16,0.5));
#30776=DIRECTION('center_axis',(-0.5,0.866025403784439,0.));
#30777=DIRECTION('ref_axis',(-0.866025403784439,-0.5,0.));
#30778=DIRECTION('',(0.,0.,1.));
#30779=DIRECTION('center_axis',(-0.5,-0.866025403784439,0.));
#30780=DIRECTION('ref_axis',(0.866025403784439,-0.5,0.));
#30781=DIRECTION('',(0.,0.,1.));
#30782=DIRECTION('center_axis',(-1.,-1.60246890531964E-16,0.));
#30783=DIRECTION('ref_axis',(1.60246890531964E-16,-1.,0.));
#30784=DIRECTION('axis',(0.,0.,1.));
#30785=DIRECTION('refdir',(1.,0.,0.));
#30786=DIRECTION('center_axis',(0.,0.,1.));
#30787=DIRECTION('ref_axis',(1.,0.,0.));
#30788=DIRECTION('',(0.,0.,-1.));
#30789=DIRECTION('center_axis',(0.,0.,1.));
#30790=DIRECTION('ref_axis',(1.,0.,0.));
#30791=DIRECTION('center_axis',(0.,0.,1.));
#30792=DIRECTION('ref_axis',(1.,0.,0.));
#30793=DIRECTION('',(0.,0.,-1.));
#30794=DIRECTION('center_axis',(0.,0.,1.));
#30795=DIRECTION('ref_axis',(1.,0.,0.));
#30796=DIRECTION('',(0.,0.,-1.));
#30797=DIRECTION('center_axis',(0.,0.,1.));
#30798=DIRECTION('ref_axis',(1.,0.,0.));
#30799=DIRECTION('',(0.,0.,-1.));
#30800=DIRECTION('center_axis',(0.,0.,1.));
#30801=DIRECTION('ref_axis',(1.,0.,0.));
#30802=DIRECTION('',(0.,0.,-1.));
#30803=DIRECTION('center_axis',(0.,0.,1.));
#30804=DIRECTION('ref_axis',(1.,0.,0.));
#30805=DIRECTION('',(0.,0.,-1.));
#30806=DIRECTION('center_axis',(0.,0.,1.));
#30807=DIRECTION('ref_axis',(1.,0.,0.));
#30808=DIRECTION('',(0.,0.,-1.));
#30809=DIRECTION('center_axis',(0.,0.,1.));
#30810=DIRECTION('ref_axis',(1.,0.,0.));
#30811=DIRECTION('',(0.,0.,-1.));
#30812=DIRECTION('center_axis',(0.,0.,1.));
#30813=DIRECTION('ref_axis',(1.,0.,0.));
#30814=DIRECTION('',(0.,0.,-1.));
#30815=DIRECTION('center_axis',(0.,0.,1.));
#30816=DIRECTION('ref_axis',(1.,0.,0.));
#30817=DIRECTION('',(0.,0.,-1.));
#30818=DIRECTION('center_axis',(0.,0.,1.));
#30819=DIRECTION('ref_axis',(1.,0.,0.));
#30820=DIRECTION('',(0.,0.,-1.));
#30821=DIRECTION('center_axis',(0.,0.,1.));
#30822=DIRECTION('ref_axis',(1.,0.,0.));
#30823=DIRECTION('',(0.,0.,-1.));
#30824=DIRECTION('center_axis',(0.,0.,1.));
#30825=DIRECTION('ref_axis',(1.,0.,0.));
#30826=DIRECTION('',(0.,0.,-1.));
#30827=DIRECTION('center_axis',(0.,0.,1.));
#30828=DIRECTION('ref_axis',(1.,0.,0.));
#30829=DIRECTION('',(0.,0.,-1.));
#30830=DIRECTION('center_axis',(0.,0.,1.));
#30831=DIRECTION('ref_axis',(1.,0.,0.));
#30832=DIRECTION('',(0.,0.,-1.));
#30833=DIRECTION('center_axis',(0.,0.,1.));
#30834=DIRECTION('ref_axis',(1.,0.,0.));
#30835=DIRECTION('',(0.,0.,-1.));
#30836=DIRECTION('center_axis',(0.,0.,1.));
#30837=DIRECTION('ref_axis',(1.,0.,0.));
#30838=DIRECTION('',(0.,0.,-1.));
#30839=DIRECTION('center_axis',(0.,0.,1.));
#30840=DIRECTION('ref_axis',(1.,0.,0.));
#30841=DIRECTION('',(0.,0.,-1.));
#30842=DIRECTION('center_axis',(0.,0.,1.));
#30843=DIRECTION('ref_axis',(1.,0.,0.));
#30844=DIRECTION('',(0.,0.,-1.));
#30845=DIRECTION('center_axis',(0.,0.,1.));
#30846=DIRECTION('ref_axis',(-0.993035084685104,-0.117819016225942,0.));
#30847=DIRECTION('',(0.,0.,1.));
#30848=DIRECTION('center_axis',(0.,0.,1.));
#30849=DIRECTION('ref_axis',(1.,1.24885942597212E-13,0.));
#30850=DIRECTION('center_axis',(0.,0.,1.));
#30851=DIRECTION('ref_axis',(1.,1.24885942597212E-13,0.));
#30852=DIRECTION('',(0.,0.,1.));
#30853=DIRECTION('center_axis',(0.,0.,1.));
#30854=DIRECTION('ref_axis',(1.,1.24885942597212E-13,0.));
#30855=DIRECTION('center_axis',(0.,0.,1.));
#30856=DIRECTION('ref_axis',(1.,1.24885942597212E-13,0.));
#30857=DIRECTION('',(0.,0.,1.));
#30858=DIRECTION('center_axis',(0.,0.,1.));
#30859=DIRECTION('ref_axis',(1.,1.24885942597212E-13,0.));
#30860=DIRECTION('',(0.,0.,1.));
#30861=DIRECTION('center_axis',(0.,0.,1.));
#30862=DIRECTION('ref_axis',(1.,1.24885942597212E-13,0.));
#30863=DIRECTION('',(0.,0.,1.));
#30864=DIRECTION('center_axis',(0.,0.,1.));
#30865=DIRECTION('ref_axis',(1.,1.24885942597212E-13,0.));
#30866=DIRECTION('',(0.,0.,1.));
#30867=DIRECTION('center_axis',(0.,0.,1.));
#30868=DIRECTION('ref_axis',(1.,1.24885942597212E-13,0.));
#30869=DIRECTION('',(0.,0.,1.));
#30870=DIRECTION('center_axis',(0.,0.,1.));
#30871=DIRECTION('ref_axis',(1.,1.24885942597212E-13,0.));
#30872=DIRECTION('',(0.,0.,1.));
#30873=DIRECTION('center_axis',(0.,0.,1.));
#30874=DIRECTION('ref_axis',(1.,1.24885942597212E-13,0.));
#30875=DIRECTION('',(0.,0.,1.));
#30876=DIRECTION('center_axis',(0.,0.,1.));
#30877=DIRECTION('ref_axis',(1.,1.24885942597212E-13,0.));
#30878=DIRECTION('',(0.,0.,1.));
#30879=DIRECTION('center_axis',(0.,0.,1.));
#30880=DIRECTION('ref_axis',(1.,1.24885942597212E-13,0.));
#30881=DIRECTION('',(0.,0.,1.));
#30882=DIRECTION('center_axis',(0.,0.,1.));
#30883=DIRECTION('ref_axis',(1.,1.24885942597212E-13,0.));
#30884=DIRECTION('',(0.,0.,1.));
#30885=DIRECTION('center_axis',(0.,0.,1.));
#30886=DIRECTION('ref_axis',(1.,1.24885942597212E-13,0.));
#30887=DIRECTION('',(0.,0.,1.));
#30888=DIRECTION('center_axis',(0.,0.,1.));
#30889=DIRECTION('ref_axis',(1.,1.24885942597212E-13,0.));
#30890=DIRECTION('',(0.,0.,1.));
#30891=DIRECTION('center_axis',(0.,0.,1.));
#30892=DIRECTION('ref_axis',(1.,1.24885942597212E-13,0.));
#30893=DIRECTION('',(0.,0.,1.));
#30894=DIRECTION('center_axis',(0.,0.,1.));
#30895=DIRECTION('ref_axis',(1.,1.24885942597212E-13,0.));
#30896=DIRECTION('',(0.,0.,1.));
#30897=DIRECTION('center_axis',(0.,0.,1.));
#30898=DIRECTION('ref_axis',(1.,1.24885942597212E-13,0.));
#30899=DIRECTION('',(0.,0.,1.));
#30900=DIRECTION('center_axis',(0.,0.,1.));
#30901=DIRECTION('ref_axis',(1.,1.24885942597212E-13,0.));
#30902=DIRECTION('',(0.,0.,1.));
#30903=DIRECTION('center_axis',(0.,0.,1.));
#30904=DIRECTION('ref_axis',(1.,1.24885942597212E-13,0.));
#30905=DIRECTION('',(0.,0.,1.));
#30906=DIRECTION('center_axis',(0.,0.,1.));
#30907=DIRECTION('ref_axis',(1.,0.,0.));
#30908=DIRECTION('center_axis',(0.,0.,-1.));
#30909=DIRECTION('ref_axis',(1.,0.,0.));
#30910=DIRECTION('center_axis',(0.,0.,-1.));
#30911=DIRECTION('ref_axis',(1.,0.,0.));
#30912=DIRECTION('center_axis',(0.,0.,1.));
#30913=DIRECTION('ref_axis',(1.,0.,0.));
#30914=DIRECTION('center_axis',(0.,0.,1.));
#30915=DIRECTION('ref_axis',(1.,0.,0.));
#30916=DIRECTION('center_axis',(0.,0.,1.));
#30917=DIRECTION('ref_axis',(1.,0.,0.));
#30918=DIRECTION('center_axis',(0.,0.,-1.));
#30919=DIRECTION('ref_axis',(1.,1.24885942597212E-13,0.));
#30920=DIRECTION('center_axis',(0.,0.,1.));
#30921=DIRECTION('ref_axis',(0.88898726725207,0.457931914877853,0.));
#30922=DIRECTION('center_axis',(0.,0.,1.));
#30923=DIRECTION('ref_axis',(1.,0.,0.));
#30924=DIRECTION('',(-1.,2.40370335797945E-16,0.));
#30925=DIRECTION('center_axis',(0.,0.,1.));
#30926=DIRECTION('ref_axis',(1.,0.,0.));
#30927=DIRECTION('center_axis',(0.,0.,1.));
#30928=DIRECTION('ref_axis',(1.,0.,0.));
#30929=DIRECTION('',(-0.5,0.866025403784439,0.));
#30930=DIRECTION('center_axis',(0.,0.,1.));
#30931=DIRECTION('ref_axis',(1.,0.,0.));
#30932=DIRECTION('center_axis',(0.,0.,1.));
#30933=DIRECTION('ref_axis',(1.,0.,0.));
#30934=DIRECTION('',(0.5,0.866025403784439,0.));
#30935=DIRECTION('center_axis',(0.,0.,1.));
#30936=DIRECTION('ref_axis',(1.,0.,0.));
#30937=DIRECTION('center_axis',(0.,0.,1.));
#30938=DIRECTION('ref_axis',(1.,0.,0.));
#30939=DIRECTION('',(1.,-1.20185167898973E-16,0.));
#30940=DIRECTION('center_axis',(0.,0.,1.));
#30941=DIRECTION('ref_axis',(1.,0.,0.));
#30942=DIRECTION('center_axis',(0.,0.,1.));
#30943=DIRECTION('ref_axis',(1.,0.,0.));
#30944=DIRECTION('',(0.5,-0.866025403784439,0.));
#30945=DIRECTION('center_axis',(0.,0.,1.));
#30946=DIRECTION('ref_axis',(1.,0.,0.));
#30947=DIRECTION('center_axis',(0.,0.,1.));
#30948=DIRECTION('ref_axis',(1.,0.,0.));
#30949=DIRECTION('',(-0.5,-0.866025403784439,0.));
#30950=DIRECTION('center_axis',(0.,0.,1.));
#30951=DIRECTION('ref_axis',(1.,0.,0.));
#30952=DIRECTION('center_axis',(0.,0.,1.));
#30953=DIRECTION('ref_axis',(1.,0.,0.));
#30954=DIRECTION('',(-0.856673567959776,-1.04912254291608E-16,0.515858893457375));
#30955=DIRECTION('center_axis',(0.,0.,-1.));
#30956=DIRECTION('ref_axis',(1.,0.,0.));
#30957=DIRECTION('center_axis',(0.,0.,-1.));
#30958=DIRECTION('ref_axis',(1.,0.,0.));
#30959=DIRECTION('center_axis',(0.,0.,-1.));
#30960=DIRECTION('ref_axis',(1.,0.,0.));
#30961=DIRECTION('center_axis',(0.,0.,-1.));
#30962=DIRECTION('ref_axis',(1.,0.,0.));
#30963=DIRECTION('center_axis',(0.,0.,-1.));
#30964=DIRECTION('ref_axis',(1.,0.,0.));
#30965=DIRECTION('center_axis',(0.,0.,-1.));
#30966=DIRECTION('ref_axis',(1.,0.,0.));
#30967=DIRECTION('center_axis',(0.,0.,-1.));
#30968=DIRECTION('ref_axis',(1.,0.,0.));
#30969=DIRECTION('center_axis',(-0.866025403784439,0.5,0.));
#30970=DIRECTION('ref_axis',(0.5,0.866025403784439,0.));
#30971=DIRECTION('',(0.,0.,-1.));
#30972=DIRECTION('',(0.5,0.866025403784439,0.));
#30973=DIRECTION('',(0.,0.,-1.));
#30974=DIRECTION('center_axis',(-0.866025403784439,0.5,0.));
#30975=DIRECTION('ref_axis',(0.5,0.866025403784439,0.));
#30976=DIRECTION('',(0.,0.,-1.));
#30977=DIRECTION('',(0.5,0.866025403784439,0.));
#30978=DIRECTION('center_axis',(1.20185167898973E-16,1.,0.));
#30979=DIRECTION('ref_axis',(1.,-1.20185167898973E-16,0.));
#30980=DIRECTION('',(0.,0.,-1.));
#30981=DIRECTION('',(1.,-1.20185167898973E-16,0.));
#30982=DIRECTION('center_axis',(1.20185167898973E-16,1.,0.));
#30983=DIRECTION('ref_axis',(1.,-1.20185167898973E-16,0.));
#30984=DIRECTION('',(1.,-1.20185167898973E-16,0.));
#30985=DIRECTION('',(0.,0.,-1.));
#30986=DIRECTION('center_axis',(1.20185167898973E-16,1.,0.));
#30987=DIRECTION('ref_axis',(1.,-1.20185167898973E-16,0.));
#30988=DIRECTION('',(0.,0.,-1.));
#30989=DIRECTION('',(1.,-1.20185167898973E-16,0.));
#30990=DIRECTION('center_axis',(-0.866025403784439,-0.5,0.));
#30991=DIRECTION('ref_axis',(-0.5,0.866025403784439,0.));
#30992=DIRECTION('',(-0.5,0.866025403784439,0.));
#30993=DIRECTION('',(0.,0.,-1.));
#30994=DIRECTION('center_axis',(-0.866025403784439,-0.5,0.));
#30995=DIRECTION('ref_axis',(-0.5,0.866025403784439,0.));
#30996=DIRECTION('',(0.,0.,-1.));
#30997=DIRECTION('',(-0.5,0.866025403784439,0.));
#30998=DIRECTION('center_axis',(0.866025403784439,0.5,0.));
#30999=DIRECTION('ref_axis',(0.5,-0.866025403784439,0.));
#31000=DIRECTION('',(0.,0.,-1.));
#31001=DIRECTION('',(0.5,-0.866025403784439,0.));
#31002=DIRECTION('center_axis',(0.866025403784439,0.5,0.));
#31003=DIRECTION('ref_axis',(0.5,-0.866025403784439,0.));
#31004=DIRECTION('',(0.5,-0.866025403784439,0.));
#31005=DIRECTION('',(0.,0.,-1.));
#31006=DIRECTION('center_axis',(0.866025403784439,0.5,0.));
#31007=DIRECTION('ref_axis',(0.5,-0.866025403784439,0.));
#31008=DIRECTION('',(0.5,-0.866025403784439,0.));
#31009=DIRECTION('center_axis',(0.,0.,-1.));
#31010=DIRECTION('ref_axis',(-1.,0.,0.));
#31011=DIRECTION('',(0.5,0.866025403784439,0.));
#31012=DIRECTION('center_axis',(0.,0.,-1.));
#31013=DIRECTION('ref_axis',(-1.,0.,0.));
#31014=DIRECTION('center_axis',(0.,0.,-1.));
#31015=DIRECTION('ref_axis',(-1.,0.,0.));
#31016=DIRECTION('',(-0.5,-0.866025403784439,0.));
#31017=DIRECTION('center_axis',(0.,0.,-1.));
#31018=DIRECTION('ref_axis',(-1.,0.,0.));
#31019=DIRECTION('',(-1.,2.40370335797945E-16,0.));
#31020=DIRECTION('',(-0.5,-0.866025403784439,0.));
#31021=DIRECTION('center_axis',(0.,0.,-1.));
#31022=DIRECTION('ref_axis',(-1.,0.,0.));
#31023=DIRECTION('',(-1.,2.40370335797945E-16,0.));
#31024=DIRECTION('center_axis',(0.,0.,-1.));
#31025=DIRECTION('ref_axis',(-1.,0.,0.));
#31026=DIRECTION('',(-0.5,0.866025403784439,0.));
#31027=DIRECTION('center_axis',(0.866025403784439,-0.5,0.));
#31028=DIRECTION('ref_axis',(-0.5,-0.866025403784439,0.));
#31029=DIRECTION('',(0.,0.,-1.));
#31030=DIRECTION('',(-0.5,-0.866025403784439,0.));
#31031=DIRECTION('center_axis',(0.866025403784439,-0.5,0.));
#31032=DIRECTION('ref_axis',(-0.5,-0.866025403784439,0.));
#31033=DIRECTION('',(0.,0.,-1.));
#31034=DIRECTION('center_axis',(0.866025403784439,-0.5,0.));
#31035=DIRECTION('ref_axis',(-0.5,-0.866025403784439,0.));
#31036=DIRECTION('center_axis',(-2.40370335797945E-16,-1.,0.));
#31037=DIRECTION('ref_axis',(-1.,2.40370335797945E-16,0.));
#31038=DIRECTION('center_axis',(-2.40370335797945E-16,-1.,0.));
#31039=DIRECTION('ref_axis',(-1.,2.40370335797945E-16,0.));
#31040=DIRECTION('',(-1.,2.40370335797945E-16,0.));
#31041=DIRECTION('center_axis',(-0.866025403784439,0.5,0.));
#31042=DIRECTION('ref_axis',(0.5,0.866025403784439,0.));
#31043=DIRECTION('center_axis',(-0.866025403784439,-0.5,0.));
#31044=DIRECTION('ref_axis',(-0.5,0.866025403784439,0.));
#31045=DIRECTION('center_axis',(-2.40370335797945E-16,-1.,0.));
#31046=DIRECTION('ref_axis',(-1.,2.40370335797945E-16,0.));
#31047=DIRECTION('center_axis',(0.,0.,-1.));
#31048=DIRECTION('ref_axis',(-1.,0.,0.));
#31049=DIRECTION('center_axis',(0.,0.,1.));
#31050=DIRECTION('ref_axis',(1.,0.,0.));
#31051=DIRECTION('center_axis',(0.,0.,1.));
#31052=DIRECTION('ref_axis',(1.,0.,0.));
#31053=DIRECTION('',(0.707106781186547,8.65956056235493E-17,-0.707106781186548));
#31054=DIRECTION('center_axis',(0.,0.,1.));
#31055=DIRECTION('ref_axis',(0.0319324117378754,-0.999490030505859,0.));
#31056=DIRECTION('center_axis',(0.,0.,-1.));
#31057=DIRECTION('ref_axis',(1.,0.,0.));
#31058=DIRECTION('center_axis',(0.,0.,-1.));
#31059=DIRECTION('ref_axis',(1.,0.,0.));
#31060=DIRECTION('center_axis',(0.,0.,1.));
#31061=DIRECTION('ref_axis',(1.,0.,0.));
#31062=DIRECTION('',(-0.707106781186548,-8.65956056235494E-17,-0.707106781186547));
#31063=DIRECTION('center_axis',(0.,0.,1.));
#31064=DIRECTION('ref_axis',(1.,0.,0.));
#31065=DIRECTION('axis',(0.,0.,1.));
#31066=DIRECTION('refdir',(1.,0.,0.));
#31067=DIRECTION('',(0.545504242983751,0.,0.838108060387636));
#31068=DIRECTION('center_axis',(0.,-1.,0.));
#31069=DIRECTION('ref_axis',(1.,0.,0.));
#31070=DIRECTION('center_axis',(0.,-1.,0.));
#31071=DIRECTION('ref_axis',(1.,0.,0.));
#31072=DIRECTION('',(0.,1.,0.));
#31073=DIRECTION('center_axis',(0.,-1.,0.));
#31074=DIRECTION('ref_axis',(1.,0.,0.));
#31075=DIRECTION('center_axis',(-0.342020143325669,0.,0.939692620785908));
#31076=DIRECTION('ref_axis',(0.939692620785909,0.,0.342020143325668));
#31077=DIRECTION('',(-0.342020143325669,0.,0.939692620785908));
#31078=DIRECTION('',(0.342020143325669,0.,-0.939692620785908));
#31079=DIRECTION('',(-0.342020143325669,0.,0.939692620785908));
#31080=DIRECTION('',(0.956605970831105,0.,-0.291384653971824));
#31081=DIRECTION('center_axis',(0.,-1.,0.));
#31082=DIRECTION('ref_axis',(1.,0.,0.));
#31083=DIRECTION('center_axis',(0.,-1.,0.));
#31084=DIRECTION('ref_axis',(1.,0.,0.));
#31085=DIRECTION('',(0.707106781186552,0.707106781186543,8.65956056235498E-17));
#31086=DIRECTION('center_axis',(0.,1.,0.));
#31087=DIRECTION('ref_axis',(1.,0.,0.));
#31088=DIRECTION('center_axis',(0.,-1.,0.));
#31089=DIRECTION('ref_axis',(1.,0.,0.));
#31090=DIRECTION('center_axis',(0.,-1.,0.));
#31091=DIRECTION('ref_axis',(1.,0.,0.));
#31092=DIRECTION('center_axis',(0.,-1.,0.));
#31093=DIRECTION('ref_axis',(1.,0.,0.));
#31094=DIRECTION('',(0.,-1.,0.));
#31095=DIRECTION('center_axis',(0.,-1.,0.));
#31096=DIRECTION('ref_axis',(1.,0.,0.));
#31097=DIRECTION('center_axis',(0.,-1.,0.));
#31098=DIRECTION('ref_axis',(0.,0.,-1.));
#31099=DIRECTION('center_axis',(0.,-1.,0.));
#31100=DIRECTION('ref_axis',(1.,0.,0.));
#31101=DIRECTION('',(0.657622941203057,-0.70669776106396,0.260979581022399));
#31102=DIRECTION('center_axis',(-0.939692620785908,0.,-0.342020143325669));
#31103=DIRECTION('ref_axis',(-0.342020143325669,0.,0.939692620785908));
#31104=DIRECTION('',(-0.939692620785908,0.,-0.342020143325669));
#31105=DIRECTION('center_axis',(0.,-1.,0.));
#31106=DIRECTION('ref_axis',(1.,0.,0.));
#31107=DIRECTION('center_axis',(0.,-1.,0.));
#31108=DIRECTION('ref_axis',(1.,0.,0.));
#31109=DIRECTION('',(0.,1.,0.));
#31110=DIRECTION('center_axis',(0.,-1.,0.));
#31111=DIRECTION('ref_axis',(1.,0.,0.));
#31112=DIRECTION('',(-0.87991994563834,0.,0.475121973042524));
#31113=DIRECTION('center_axis',(0.,1.,0.));
#31114=DIRECTION('ref_axis',(0.,0.,1.));
#31115=DIRECTION('center_axis',(0.,1.,0.));
#31116=DIRECTION('ref_axis',(0.,0.,1.));
#31117=DIRECTION('center_axis',(0.,1.,0.));
#31118=DIRECTION('ref_axis',(0.,0.,1.));
#31119=DIRECTION('center_axis',(0.,1.,0.));
#31120=DIRECTION('ref_axis',(1.,0.,0.));
#31121=DIRECTION('',(-0.707106781186547,0.707106781186547,-8.65956056235493E-17));
#31122=DIRECTION('center_axis',(0.,-1.,0.));
#31123=DIRECTION('ref_axis',(1.,0.,0.));
#31124=DIRECTION('center_axis',(0.,1.,0.));
#31125=DIRECTION('ref_axis',(0.,0.,1.));
#31126=DIRECTION('center_axis',(0.,-1.,0.));
#31127=DIRECTION('ref_axis',(1.,0.,0.));
#31128=DIRECTION('center_axis',(0.,-1.,0.));
#31129=DIRECTION('ref_axis',(1.,0.,0.));
#31130=DIRECTION('',(0.707106781186548,0.707106781186548,8.65956056235493E-17));
#31131=DIRECTION('center_axis',(0.,1.,0.));
#31132=DIRECTION('ref_axis',(1.,0.,0.));
#31133=DIRECTION('',(-0.707106781186548,0.707106781186548,-8.65956056235493E-17));
#31134=DIRECTION('axis',(0.,0.,1.));
#31135=DIRECTION('refdir',(1.,0.,0.));
#31136=DIRECTION('center_axis',(0.819152044289004,0.,-0.573576436351029));
#31137=DIRECTION('ref_axis',(-0.573576436351029,0.,-0.819152044289004));
#31138=DIRECTION('',(0.497542812164512,-0.497542812164512,0.710564775461646));
#31139=DIRECTION('',(0.,-1.,0.));
#31140=DIRECTION('',(-0.497542812164512,-0.497542812164512,-0.710564775461646));
#31141=DIRECTION('',(-0.497542812164487,0.497542812164587,-0.71056477546161));
#31142=DIRECTION('',(0.,1.,0.));
#31143=DIRECTION('',(0.4975428121645,0.497542812164547,0.710564775461629));
#31144=DIRECTION('center_axis',(0.24184476264798,0.707106781186536,-0.664463024388686));
#31145=DIRECTION('ref_axis',(-0.939692620785908,0.,-0.342020143325669));
#31146=DIRECTION('',(-0.939692620785908,0.,-0.342020143325669));
#31147=DIRECTION('',(-0.633687274224646,0.63368727422465,0.443712606279642));
#31148=DIRECTION('',(0.939692620785908,0.,0.342020143325669));
#31149=DIRECTION('',(0.633687274224648,-0.633687274224648,-0.44371260627964));
#31150=DIRECTION('center_axis',(-0.342020143325669,0.,0.939692620785908));
#31151=DIRECTION('ref_axis',(0.939692620785908,0.,0.342020143325669));
#31152=DIRECTION('',(0.939692620785908,0.,0.342020143325669));
#31153=DIRECTION('',(0.,1.,0.));
#31154=DIRECTION('center_axis',(0.241844762647992,-0.707106781186498,-0.664463024388721));
#31155=DIRECTION('ref_axis',(-0.939692620785908,0.,-0.342020143325669));
#31156=DIRECTION('',(-0.633687274224669,-0.633687274224669,0.443712606279582));
#31157=DIRECTION('',(-0.939692620785908,0.,-0.342020143325669));
#31158=DIRECTION('',(0.633687274224669,0.633687274224671,-0.443712606279578));
#31159=DIRECTION('center_axis',(0.819152044289004,0.,-0.573576436351029));
#31160=DIRECTION('ref_axis',(-0.573576436351029,0.,-0.819152044289004));
#31161=DIRECTION('',(0.497542812164512,-0.497542812164512,0.710564775461646));
#31162=DIRECTION('',(0.,-1.,0.));
#31163=DIRECTION('',(-0.497542812164512,-0.497542812164512,-0.710564775461646));
#31164=DIRECTION('',(-0.497542812164499,0.497542812164549,-0.710564775461628));
#31165=DIRECTION('',(0.,1.,0.));
#31166=DIRECTION('',(0.4975428121645,0.497542812164547,0.710564775461629));
#31167=DIRECTION('center_axis',(0.24184476264798,0.707106781186535,-0.664463024388686));
#31168=DIRECTION('ref_axis',(-0.939692620785908,0.,-0.342020143325669));
#31169=DIRECTION('',(-0.939692620785908,0.,-0.342020143325669));
#31170=DIRECTION('',(-0.633687274224646,0.63368727422465,0.443712606279641));
#31171=DIRECTION('',(0.939692620785908,0.,0.342020143325669));
#31172=DIRECTION('',(0.633687274224649,-0.633687274224649,-0.443712606279638));
#31173=DIRECTION('center_axis',(-0.342020143325669,0.,0.939692620785908));
#31174=DIRECTION('ref_axis',(0.939692620785908,0.,0.342020143325669));
#31175=DIRECTION('',(0.939692620785908,0.,0.342020143325669));
#31176=DIRECTION('',(0.,1.,0.));
#31177=DIRECTION('center_axis',(0.24184476264798,-0.707106781186533,-0.664463024388688));
#31178=DIRECTION('ref_axis',(-0.939692620785908,0.,-0.342020143325669));
#31179=DIRECTION('',(-0.63368727422465,-0.63368727422465,0.443712606279635));
#31180=DIRECTION('',(-0.939692620785908,0.,-0.342020143325669));
#31181=DIRECTION('',(0.633687274224652,0.633687274224654,-0.443712606279627));
#31182=DIRECTION('center_axis',(0.819152044289004,0.,-0.573576436351029));
#31183=DIRECTION('ref_axis',(-0.573576436351029,0.,-0.819152044289004));
#31184=DIRECTION('',(0.497542812164512,-0.497542812164512,0.710564775461646));
#31185=DIRECTION('',(0.,-1.,0.));
#31186=DIRECTION('',(-0.497542812164512,-0.497542812164512,-0.710564775461646));
#31187=DIRECTION('',(-0.497542812164502,0.497542812164542,-0.710564775461631));
#31188=DIRECTION('',(0.,1.,0.));
#31189=DIRECTION('',(0.497542812164502,0.49754281216454,0.710564775461632));
#31190=DIRECTION('center_axis',(-0.342020143325678,0.,0.939692620785905));
#31191=DIRECTION('ref_axis',(0.939692620785905,0.,0.342020143325678));
#31192=DIRECTION('',(0.939692620785905,0.,0.342020143325678));
#31193=DIRECTION('',(0.,1.,0.));
#31194=DIRECTION('',(-0.939692620785905,0.,-0.342020143325678));
#31195=DIRECTION('center_axis',(0.241844762647986,-0.707106781186536,-0.664463024388684));
#31196=DIRECTION('ref_axis',(-0.939692620785905,0.,-0.342020143325678));
#31197=DIRECTION('',(-0.63368727422465,-0.63368727422465,0.443712606279636));
#31198=DIRECTION('',(-0.939692620785905,0.,-0.342020143325678));
#31199=DIRECTION('',(0.633687274224652,0.633687274224654,-0.443712606279627));
#31200=DIRECTION('center_axis',(0.707106781186548,-0.707106781186548,0.));
#31201=DIRECTION('ref_axis',(0.,0.,-1.));
#31202=DIRECTION('',(0.,0.,1.));
#31203=DIRECTION('',(0.497542812164512,0.497542812164512,-0.710564775461646));
#31204=DIRECTION('',(0.63368727422465,0.63368727422465,0.443712606279634));
#31205=DIRECTION('',(0.,0.,-1.));
#31206=DIRECTION('center_axis',(0.819152044289001,0.,-0.573576436351034));
#31207=DIRECTION('ref_axis',(-0.573576436351034,0.,-0.819152044289001));
#31208=DIRECTION('',(0.497542812164515,-0.497542812164515,0.710564775461641));
#31209=DIRECTION('',(0.,-1.,0.));
#31210=DIRECTION('',(-0.497542812164515,-0.497542812164515,-0.710564775461641));
#31211=DIRECTION('',(-0.497542812164508,0.497542812164537,-0.710564775461631));
#31212=DIRECTION('',(0.,1.,0.));
#31213=DIRECTION('',(0.49754281216452,0.497542812164499,0.710564775461649));
#31214=DIRECTION('center_axis',(0.241844762647973,0.707106781186573,-0.664463024388649));
#31215=DIRECTION('ref_axis',(-0.939692620785905,0.,-0.342020143325678));
#31216=DIRECTION('',(-0.939692620785905,0.,-0.342020143325678));
#31217=DIRECTION('',(-0.633687274224627,0.633687274224631,0.443712606279695));
#31218=DIRECTION('',(0.939692620785905,0.,0.342020143325678));
#31219=DIRECTION('',(0.63368727422463,-0.63368727422463,-0.443712606279693));
#31220=DIRECTION('center_axis',(-0.342020143325678,0.,0.939692620785905));
#31221=DIRECTION('ref_axis',(0.939692620785905,0.,0.342020143325678));
#31222=DIRECTION('',(0.939692620785905,0.,0.342020143325678));
#31223=DIRECTION('',(0.,1.,0.));
#31224=DIRECTION('center_axis',(0.241844762647985,-0.707106781186537,-0.664463024388682));
#31225=DIRECTION('ref_axis',(-0.939692620785905,0.,-0.342020143325678));
#31226=DIRECTION('',(-0.633687274224649,-0.633687274224649,0.443712606279638));
#31227=DIRECTION('',(-0.939692620785905,0.,-0.342020143325678));
#31228=DIRECTION('',(0.633687274224652,0.633687274224654,-0.443712606279627));
#31229=DIRECTION('center_axis',(0.819152044289004,0.,-0.573576436351029));
#31230=DIRECTION('ref_axis',(-0.573576436351029,0.,-0.819152044289004));
#31231=DIRECTION('',(0.497542812164512,-0.497542812164512,0.710564775461646));
#31232=DIRECTION('',(0.,-1.,0.));
#31233=DIRECTION('',(-0.497542812164512,-0.497542812164512,-0.710564775461646));
#31234=DIRECTION('',(-0.4975428121645,0.497542812164547,-0.710564775461629));
#31235=DIRECTION('',(0.,1.,0.));
#31236=DIRECTION('',(0.497542812164501,0.497542812164546,0.71056477546163));
#31237=DIRECTION('center_axis',(1.,0.,0.));
#31238=DIRECTION('ref_axis',(0.,1.,0.));
#31239=DIRECTION('',(0.,0.,-1.));
#31240=DIRECTION('',(0.,1.,0.));
#31241=DIRECTION('',(0.,0.,1.));
#31242=DIRECTION('center_axis',(0.707106781186548,0.707106781186548,0.));
#31243=DIRECTION('ref_axis',(0.,0.,-1.));
#31244=DIRECTION('',(0.633687274224648,-0.633687274224648,-0.443712606279641));
#31245=DIRECTION('',(0.,0.,1.));
#31246=DIRECTION('',(-0.633687274224686,0.633687274224686,-0.443712606279532));
#31247=DIRECTION('',(-0.497542812164537,0.497542812164537,0.71056477546161));
#31248=DIRECTION('center_axis',(0.241844762647979,0.707106781186536,-0.664463024388685));
#31249=DIRECTION('ref_axis',(-0.939692620785908,0.,-0.342020143325669));
#31250=DIRECTION('',(-0.939692620785908,0.,-0.342020143325669));
#31251=DIRECTION('',(-0.633687274224634,0.633687274224638,0.443712606279675));
#31252=DIRECTION('',(0.939692620785908,0.,0.342020143325669));
#31253=DIRECTION('center_axis',(0.819152044289002,0.,0.573576436351031));
#31254=DIRECTION('ref_axis',(0.573576436351031,0.,-0.819152044289002));
#31255=DIRECTION('',(0.497542812164513,0.497542812164513,-0.710564775461643));
#31256=DIRECTION('',(0.,1.,0.));
#31257=DIRECTION('',(-0.497542812164513,0.497542812164513,0.710564775461643));
#31258=DIRECTION('',(-0.497542812164503,-0.497542812164545,0.710564775461628));
#31259=DIRECTION('',(0.,-1.,0.));
#31260=DIRECTION('',(0.497542812164502,-0.497542812164547,-0.710564775461627));
#31261=DIRECTION('center_axis',(0.24184476264798,0.707106781186536,0.664463024388686));
#31262=DIRECTION('ref_axis',(0.939692620785908,0.,-0.342020143325669));
#31263=DIRECTION('',(-0.633687274224648,0.633687274224648,-0.44371260627964));
#31264=DIRECTION('',(-0.939692620785908,0.,0.342020143325669));
#31265=DIRECTION('',(-0.633687274224657,0.633687274224651,-0.443712606279624));
#31266=DIRECTION('',(0.939692620785908,0.,-0.342020143325669));
#31267=DIRECTION('center_axis',(0.707106781186548,0.707106781186548,0.));
#31268=DIRECTION('ref_axis',(0.,0.,-1.));
#31269=DIRECTION('',(0.,0.,-1.));
#31270=DIRECTION('',(0.497542812164488,-0.497542812164488,0.710564775461679));
#31271=DIRECTION('',(0.633687274224649,-0.633687274224649,-0.443712606279638));
#31272=DIRECTION('',(0.,0.,1.));
#31273=DIRECTION('center_axis',(1.,0.,0.));
#31274=DIRECTION('ref_axis',(0.,1.,0.));
#31275=DIRECTION('',(0.,0.,1.));
#31276=DIRECTION('',(0.,-1.,0.));
#31277=DIRECTION('center_axis',(0.81915204428903,0.,-0.573576436350992));
#31278=DIRECTION('ref_axis',(-0.573576436350992,0.,-0.81915204428903));
#31279=DIRECTION('',(-0.497542812164488,-0.497542812164488,-0.710564775461679));
#31280=DIRECTION('',(-0.497542812164461,0.49754281216457,-0.710564775461641));
#31281=DIRECTION('',(0.,1.,0.));
#31282=DIRECTION('',(0.49754281216446,0.497542812164572,0.71056477546164));
#31283=DIRECTION('center_axis',(0.24184476264798,0.707106781186534,-0.664463024388687));
#31284=DIRECTION('ref_axis',(-0.939692620785908,0.,-0.342020143325669));
#31285=DIRECTION('',(-0.939692620785908,0.,-0.342020143325669));
#31286=DIRECTION('',(-0.633687274224651,0.633687274224655,0.443712606279627));
#31287=DIRECTION('',(0.939692620785908,0.,0.342020143325669));
#31288=DIRECTION('center_axis',(0.819152044289004,0.,0.573576436351029));
#31289=DIRECTION('ref_axis',(0.573576436351029,0.,-0.819152044289004));
#31290=DIRECTION('',(0.497542812164512,0.497542812164512,-0.710564775461646));
#31291=DIRECTION('',(0.,1.,0.));
#31292=DIRECTION('',(-0.497542812164512,0.497542812164512,0.710564775461646));
#31293=DIRECTION('',(-0.4975428121645,-0.497542812164548,0.710564775461629));
#31294=DIRECTION('',(0.,-1.,0.));
#31295=DIRECTION('',(0.497542812164488,-0.497542812164584,-0.710564775461612));
#31296=DIRECTION('center_axis',(-0.342020143325669,0.,-0.939692620785908));
#31297=DIRECTION('ref_axis',(-0.939692620785908,0.,0.342020143325669));
#31298=DIRECTION('',(0.939692620785908,0.,-0.342020143325669));
#31299=DIRECTION('',(0.,1.,0.));
#31300=DIRECTION('',(-0.939692620785908,0.,0.342020143325669));
#31301=DIRECTION('center_axis',(0.24184476264798,0.707106781186534,0.664463024388687));
#31302=DIRECTION('ref_axis',(0.939692620785908,0.,-0.342020143325669));
#31303=DIRECTION('',(-0.633687274224649,0.633687274224649,-0.443712606279638));
#31304=DIRECTION('',(-0.939692620785908,0.,0.342020143325669));
#31305=DIRECTION('',(-0.633687274224654,0.633687274224652,-0.443712606279625));
#31306=DIRECTION('center_axis',(0.707106781186548,0.707106781186548,0.));
#31307=DIRECTION('ref_axis',(0.,0.,-1.));
#31308=DIRECTION('',(0.,0.,1.));
#31309=DIRECTION('',(0.,0.,-1.));
#31310=DIRECTION('center_axis',(0.819152044288976,0.,-0.573576436351068));
#31311=DIRECTION('ref_axis',(-0.573576436351068,0.,-0.819152044288976));
#31312=DIRECTION('',(0.497542812164537,-0.497542812164537,0.71056477546161));
#31313=DIRECTION('',(0.,-1.,0.));
#31314=DIRECTION('',(-0.497542812164537,-0.497542812164537,-0.71056477546161));
#31315=DIRECTION('',(-0.497542812164543,0.497542812164522,-0.710564775461617));
#31316=DIRECTION('',(0.,1.,0.));
#31317=DIRECTION('',(0.497542812164529,0.497542812164561,0.710564775461598));
#31318=DIRECTION('center_axis',(1.,0.,0.));
#31319=DIRECTION('ref_axis',(0.,1.,0.));
#31320=DIRECTION('',(0.,0.,-1.));
#31321=DIRECTION('',(0.,1.,0.));
#31322=DIRECTION('',(0.,0.,1.));
#31323=DIRECTION('center_axis',(0.707106781186548,0.707106781186548,0.));
#31324=DIRECTION('ref_axis',(0.,0.,-1.));
#31325=DIRECTION('',(0.633687274224669,-0.633687274224669,-0.443712606279581));
#31326=DIRECTION('',(0.,0.,1.));
#31327=DIRECTION('',(-0.633687274224648,0.633687274224648,-0.44371260627964));
#31328=DIRECTION('',(-0.497542812164512,0.497542812164512,0.710564775461646));
#31329=DIRECTION('center_axis',(0.241844762647993,0.707106781186498,-0.664463024388722));
#31330=DIRECTION('ref_axis',(-0.939692620785908,0.,-0.342020143325669));
#31331=DIRECTION('',(-0.939692620785908,0.,-0.342020143325669));
#31332=DIRECTION('',(-0.633687274224668,0.633687274224672,0.443712606279579));
#31333=DIRECTION('',(0.939692620785908,0.,0.342020143325669));
#31334=DIRECTION('center_axis',(0.819152044289004,0.,0.573576436351029));
#31335=DIRECTION('ref_axis',(0.573576436351029,0.,-0.819152044289004));
#31336=DIRECTION('',(0.497542812164512,0.497542812164512,-0.710564775461646));
#31337=DIRECTION('',(0.,1.,0.));
#31338=DIRECTION('',(-0.497542812164512,0.497542812164512,0.710564775461646));
#31339=DIRECTION('',(-0.4975428121645,-0.497542812164547,0.710564775461629));
#31340=DIRECTION('',(0.,-1.,0.));
#31341=DIRECTION('',(0.497542812164487,-0.497542812164587,-0.71056477546161));
#31342=DIRECTION('center_axis',(0.24184476264798,0.707106781186535,0.664463024388686));
#31343=DIRECTION('ref_axis',(0.939692620785908,0.,-0.342020143325669));
#31344=DIRECTION('',(-0.633687274224649,0.633687274224649,-0.443712606279638));
#31345=DIRECTION('',(-0.939692620785908,0.,0.342020143325669));
#31346=DIRECTION('',(-0.633687274224652,0.633687274224654,-0.443712606279627));
#31347=DIRECTION('',(0.939692620785908,0.,-0.342020143325669));
#31348=DIRECTION('center_axis',(0.707106781186548,0.707106781186548,0.));
#31349=DIRECTION('ref_axis',(0.,0.,-1.));
#31350=DIRECTION('',(0.,0.,-1.));
#31351=DIRECTION('',(0.497542812164512,-0.497542812164512,0.710564775461646));
#31352=DIRECTION('',(0.633687274224649,-0.633687274224649,-0.443712606279638));
#31353=DIRECTION('',(0.,0.,1.));
#31354=DIRECTION('center_axis',(1.,0.,0.));
#31355=DIRECTION('ref_axis',(0.,1.,0.));
#31356=DIRECTION('',(0.,0.,1.));
#31357=DIRECTION('',(0.,-1.,0.));
#31358=DIRECTION('center_axis',(0.819152044289004,0.,-0.573576436351029));
#31359=DIRECTION('ref_axis',(-0.573576436351029,0.,-0.819152044289004));
#31360=DIRECTION('',(-0.497542812164512,-0.497542812164512,-0.710564775461646));
#31361=DIRECTION('',(-0.497542812164501,0.497542812164546,-0.71056477546163));
#31362=DIRECTION('',(0.,1.,0.));
#31363=DIRECTION('',(0.4975428121645,0.497542812164548,0.710564775461629));
#31364=DIRECTION('center_axis',(0.24184476264798,0.707106781186535,-0.664463024388687));
#31365=DIRECTION('ref_axis',(-0.939692620785908,0.,-0.342020143325669));
#31366=DIRECTION('',(-0.939692620785908,0.,-0.342020143325669));
#31367=DIRECTION('',(-0.633687274224651,0.633687274224655,0.443712606279627));
#31368=DIRECTION('',(0.939692620785908,0.,0.342020143325669));
#31369=DIRECTION('center_axis',(0.819152044289004,0.,0.573576436351029));
#31370=DIRECTION('ref_axis',(0.573576436351029,0.,-0.819152044289004));
#31371=DIRECTION('',(0.497542812164512,0.497542812164512,-0.710564775461646));
#31372=DIRECTION('',(0.,1.,0.));
#31373=DIRECTION('',(-0.497542812164512,0.497542812164512,0.710564775461646));
#31374=DIRECTION('',(-0.4975428121645,-0.497542812164549,0.710564775461628));
#31375=DIRECTION('',(0.,-1.,0.));
#31376=DIRECTION('',(0.4975428121645,-0.497542812164546,-0.710564775461629));
#31377=DIRECTION('center_axis',(-0.342020143325669,0.,-0.939692620785908));
#31378=DIRECTION('ref_axis',(-0.939692620785908,0.,0.342020143325669));
#31379=DIRECTION('',(0.939692620785908,0.,-0.342020143325669));
#31380=DIRECTION('',(0.,1.,0.));
#31381=DIRECTION('',(-0.939692620785908,0.,0.342020143325669));
#31382=DIRECTION('center_axis',(0.24184476264798,0.707106781186534,0.664463024388688));
#31383=DIRECTION('ref_axis',(0.939692620785908,0.,-0.342020143325669));
#31384=DIRECTION('',(-0.63368727422465,0.63368727422465,-0.443712606279636));
#31385=DIRECTION('',(-0.939692620785908,0.,0.342020143325669));
#31386=DIRECTION('',(-0.63368727422465,0.633687274224655,-0.443712606279628));
#31387=DIRECTION('center_axis',(0.707106781186548,0.707106781186548,0.));
#31388=DIRECTION('ref_axis',(0.,0.,-1.));
#31389=DIRECTION('',(0.,0.,1.));
#31390=DIRECTION('',(0.,0.,-1.));
#31391=DIRECTION('center_axis',(0.819152044289004,0.,0.573576436351029));
#31392=DIRECTION('ref_axis',(0.573576436351029,0.,-0.819152044289004));
#31393=DIRECTION('',(0.497542812164512,0.497542812164512,-0.710564775461646));
#31394=DIRECTION('',(0.,1.,0.));
#31395=DIRECTION('',(-0.497542812164512,0.497542812164512,0.710564775461646));
#31396=DIRECTION('',(-0.4975428121645,-0.497542812164546,0.710564775461629));
#31397=DIRECTION('',(0.,-1.,0.));
#31398=DIRECTION('',(0.4975428121645,-0.497542812164548,-0.710564775461629));
#31399=DIRECTION('center_axis',(0.24184476264798,0.707106781186536,0.664463024388686));
#31400=DIRECTION('ref_axis',(0.939692620785908,0.,-0.342020143325669));
#31401=DIRECTION('',(-0.633687274224648,0.633687274224648,-0.44371260627964));
#31402=DIRECTION('',(-0.939692620785908,0.,0.342020143325669));
#31403=DIRECTION('',(-0.633687274224659,0.633687274224649,-0.443712606279623));
#31404=DIRECTION('',(0.939692620785908,0.,-0.342020143325669));
#31405=DIRECTION('center_axis',(0.707106781186548,0.707106781186548,0.));
#31406=DIRECTION('ref_axis',(0.,0.,-1.));
#31407=DIRECTION('',(0.,0.,-1.));
#31408=DIRECTION('',(0.497542812164537,-0.497542812164537,0.71056477546161));
#31409=DIRECTION('',(0.633687274224667,-0.633687274224667,-0.443712606279587));
#31410=DIRECTION('',(0.,0.,1.));
#31411=DIRECTION('center_axis',(1.,0.,0.));
#31412=DIRECTION('ref_axis',(0.,1.,0.));
#31413=DIRECTION('',(0.,0.,1.));
#31414=DIRECTION('',(0.,-1.,0.));
#31415=DIRECTION('center_axis',(0.819152044288976,0.,-0.573576436351068));
#31416=DIRECTION('ref_axis',(-0.573576436351068,0.,-0.819152044288976));
#31417=DIRECTION('',(-0.497542812164537,-0.497542812164537,-0.71056477546161));
#31418=DIRECTION('',(-0.49754281216453,0.497542812164559,-0.710564775461599));
#31419=DIRECTION('',(0.,1.,0.));
#31420=DIRECTION('',(0.497542812164531,0.497542812164557,0.7105647754616));
#31421=DIRECTION('center_axis',(0.241844762647991,0.707106781186501,-0.664463024388718));
#31422=DIRECTION('ref_axis',(-0.939692620785908,0.,-0.342020143325669));
#31423=DIRECTION('',(-0.939692620785908,0.,-0.342020143325669));
#31424=DIRECTION('',(-0.633687274224651,0.633687274224655,0.443712606279627));
#31425=DIRECTION('',(0.939692620785908,0.,0.342020143325669));
#31426=DIRECTION('center_axis',(0.819152044289004,0.,0.573576436351029));
#31427=DIRECTION('ref_axis',(0.573576436351029,0.,-0.819152044289004));
#31428=DIRECTION('',(0.497542812164512,0.497542812164512,-0.710564775461646));
#31429=DIRECTION('',(0.,1.,0.));
#31430=DIRECTION('',(-0.497542812164512,0.497542812164512,0.710564775461646));
#31431=DIRECTION('',(-0.4975428121645,-0.497542812164548,0.710564775461629));
#31432=DIRECTION('',(0.,-1.,0.));
#31433=DIRECTION('',(0.497542812164488,-0.497542812164583,-0.710564775461612));
#31434=DIRECTION('center_axis',(-0.342020143325669,0.,-0.939692620785908));
#31435=DIRECTION('ref_axis',(-0.939692620785908,0.,0.342020143325669));
#31436=DIRECTION('',(0.939692620785908,0.,-0.342020143325669));
#31437=DIRECTION('',(0.,1.,0.));
#31438=DIRECTION('',(-0.939692620785908,0.,0.342020143325669));
#31439=DIRECTION('center_axis',(0.24184476264798,0.707106781186534,0.664463024388687));
#31440=DIRECTION('ref_axis',(0.939692620785908,0.,-0.342020143325669));
#31441=DIRECTION('',(-0.633687274224649,0.633687274224649,-0.443712606279638));
#31442=DIRECTION('',(-0.939692620785908,0.,0.342020143325669));
#31443=DIRECTION('',(-0.633687274224652,0.633687274224654,-0.443712606279627));
#31444=DIRECTION('center_axis',(0.707106781186548,0.707106781186548,0.));
#31445=DIRECTION('ref_axis',(0.,0.,-1.));
#31446=DIRECTION('',(0.,0.,-1.));
#31447=DIRECTION('',(0.497542812164512,-0.497542812164512,0.710564775461646));
#31448=DIRECTION('',(0.633687274224649,-0.633687274224649,-0.443712606279638));
#31449=DIRECTION('',(0.,0.,1.));
#31450=DIRECTION('center_axis',(0.819152044289004,0.,-0.573576436351029));
#31451=DIRECTION('ref_axis',(-0.573576436351029,0.,-0.819152044289004));
#31452=DIRECTION('',(0.,-1.,0.));
#31453=DIRECTION('',(-0.497542812164512,-0.497542812164512,-0.710564775461646));
#31454=DIRECTION('',(-0.497542812164501,0.497542812164545,-0.71056477546163));
#31455=DIRECTION('',(0.,1.,0.));
#31456=DIRECTION('',(0.4975428121645,0.497542812164548,0.710564775461629));
#31457=DIRECTION('center_axis',(-0.342020143325669,0.,0.939692620785908));
#31458=DIRECTION('ref_axis',(0.939692620785908,0.,0.342020143325669));
#31459=DIRECTION('',(0.939692620785908,0.,0.342020143325669));
#31460=DIRECTION('',(0.,1.,0.));
#31461=DIRECTION('',(-0.939692620785908,0.,-0.342020143325669));
#31462=DIRECTION('center_axis',(0.241844762647979,-0.707106781186537,-0.664463024388685));
#31463=DIRECTION('ref_axis',(-0.939692620785908,0.,-0.342020143325669));
#31464=DIRECTION('',(-0.633687274224648,-0.633687274224648,0.443712606279641));
#31465=DIRECTION('',(-0.939692620785908,0.,-0.342020143325669));
#31466=DIRECTION('',(0.633687274224635,0.633687274224637,-0.443712606279675));
#31467=DIRECTION('center_axis',(0.707106781186548,-0.707106781186548,0.));
#31468=DIRECTION('ref_axis',(0.,0.,-1.));
#31469=DIRECTION('',(0.633687274224667,0.633687274224667,0.443712606279586));
#31470=DIRECTION('',(0.,0.,-1.));
#31471=DIRECTION('',(0.,0.,1.));
#31472=DIRECTION('center_axis',(0.819152044289004,0.,0.573576436351029));
#31473=DIRECTION('ref_axis',(0.573576436351029,0.,-0.819152044289004));
#31474=DIRECTION('',(0.497542812164512,0.497542812164512,-0.710564775461646));
#31475=DIRECTION('',(0.,1.,0.));
#31476=DIRECTION('',(-0.497542812164512,0.497542812164512,0.710564775461646));
#31477=DIRECTION('',(-0.4975428121645,-0.497542812164549,0.710564775461628));
#31478=DIRECTION('',(0.,-1.,0.));
#31479=DIRECTION('',(0.4975428121645,-0.497542812164546,-0.710564775461629));
#31480=DIRECTION('center_axis',(0.24184476264798,0.707106781186534,0.664463024388688));
#31481=DIRECTION('ref_axis',(0.939692620785908,0.,-0.342020143325669));
#31482=DIRECTION('',(-0.63368727422465,0.63368727422465,-0.443712606279636));
#31483=DIRECTION('',(-0.939692620785908,0.,0.342020143325669));
#31484=DIRECTION('',(-0.63368727422465,0.633687274224655,-0.443712606279628));
#31485=DIRECTION('',(0.939692620785908,0.,-0.342020143325669));
#31486=DIRECTION('center_axis',(0.707106781186548,0.707106781186548,0.));
#31487=DIRECTION('ref_axis',(0.,0.,-1.));
#31488=DIRECTION('',(0.,0.,-1.));
#31489=DIRECTION('',(0.497542812164512,-0.497542812164512,0.710564775461646));
#31490=DIRECTION('',(0.633687274224648,-0.633687274224648,-0.44371260627964));
#31491=DIRECTION('',(0.,0.,1.));
#31492=DIRECTION('center_axis',(1.,0.,0.));
#31493=DIRECTION('ref_axis',(0.,1.,0.));
#31494=DIRECTION('',(0.,0.,1.));
#31495=DIRECTION('',(0.,-1.,0.));
#31496=DIRECTION('center_axis',(0.819152044289004,0.,-0.573576436351029));
#31497=DIRECTION('ref_axis',(-0.573576436351029,0.,-0.819152044289004));
#31498=DIRECTION('',(-0.497542812164512,-0.497542812164512,-0.710564775461646));
#31499=DIRECTION('',(-0.497542812164512,0.49754281216451,-0.710564775461646));
#31500=DIRECTION('',(0.,1.,0.));
#31501=DIRECTION('',(0.4975428121645,0.497542812164546,0.710564775461629));
#31502=DIRECTION('center_axis',(0.241844762647979,0.707106781186536,-0.664463024388685));
#31503=DIRECTION('ref_axis',(-0.939692620785908,0.,-0.342020143325669));
#31504=DIRECTION('',(-0.939692620785908,0.,-0.342020143325669));
#31505=DIRECTION('',(-0.633687274224634,0.633687274224638,0.443712606279675));
#31506=DIRECTION('',(0.939692620785908,0.,0.342020143325669));
#31507=DIRECTION('center_axis',(0.819152044289004,0.,0.573576436351029));
#31508=DIRECTION('ref_axis',(0.573576436351029,0.,-0.819152044289004));
#31509=DIRECTION('',(0.497542812164512,0.497542812164512,-0.710564775461646));
#31510=DIRECTION('',(0.,1.,0.));
#31511=DIRECTION('',(-0.497542812164512,0.497542812164512,0.710564775461646));
#31512=DIRECTION('',(-0.4975428121645,-0.497542812164546,0.710564775461629));
#31513=DIRECTION('',(0.,-1.,0.));
#31514=DIRECTION('',(0.4975428121645,-0.497542812164549,-0.710564775461628));
#31515=DIRECTION('center_axis',(0.24184476264798,0.707106781186536,0.664463024388686));
#31516=DIRECTION('ref_axis',(0.939692620785908,0.,-0.342020143325669));
#31517=DIRECTION('',(-0.633687274224648,0.633687274224648,-0.44371260627964));
#31518=DIRECTION('',(-0.939692620785908,0.,0.342020143325669));
#31519=DIRECTION('',(-0.633687274224658,0.63368727422465,-0.443712606279624));
#31520=DIRECTION('',(0.939692620785908,0.,-0.342020143325669));
#31521=DIRECTION('center_axis',(0.707106781186548,0.707106781186548,0.));
#31522=DIRECTION('ref_axis',(0.,0.,-1.));
#31523=DIRECTION('',(0.,0.,-1.));
#31524=DIRECTION('',(0.497542812164537,-0.497542812164537,0.71056477546161));
#31525=DIRECTION('',(0.633687274224669,-0.633687274224669,-0.443712606279581));
#31526=DIRECTION('',(0.,0.,1.));
#31527=DIRECTION('center_axis',(1.,0.,0.));
#31528=DIRECTION('ref_axis',(0.,1.,0.));
#31529=DIRECTION('',(0.,0.,1.));
#31530=DIRECTION('',(0.,-1.,0.));
#31531=DIRECTION('center_axis',(0.819152044288976,0.,-0.573576436351068));
#31532=DIRECTION('ref_axis',(-0.573576436351068,0.,-0.819152044288976));
#31533=DIRECTION('',(-0.497542812164537,-0.497542812164537,-0.71056477546161));
#31534=DIRECTION('',(-0.49754281216453,0.497542812164559,-0.7105647754616));
#31535=DIRECTION('',(0.,1.,0.));
#31536=DIRECTION('',(0.49754281216453,0.497542812164561,0.710564775461598));
#31537=DIRECTION('center_axis',(0.241844762647993,0.707106781186498,-0.664463024388722));
#31538=DIRECTION('ref_axis',(-0.939692620785908,0.,-0.342020143325669));
#31539=DIRECTION('',(-0.939692620785908,0.,-0.342020143325669));
#31540=DIRECTION('',(-0.633687274224668,0.633687274224672,0.443712606279579));
#31541=DIRECTION('',(0.939692620785908,0.,0.342020143325669));
#31542=DIRECTION('center_axis',(0.819152044289004,0.,0.573576436351029));
#31543=DIRECTION('ref_axis',(0.573576436351029,0.,-0.819152044289004));
#31544=DIRECTION('',(0.497542812164512,0.497542812164512,-0.710564775461646));
#31545=DIRECTION('',(0.,1.,0.));
#31546=DIRECTION('',(-0.497542812164512,0.497542812164512,0.710564775461646));
#31547=DIRECTION('',(-0.4975428121645,-0.497542812164548,0.710564775461629));
#31548=DIRECTION('',(0.,-1.,0.));
#31549=DIRECTION('',(0.497542812164476,-0.497542812164621,-0.710564775461594));
#31550=DIRECTION('center_axis',(0.241844762648004,-0.707106781186466,0.664463024388752));
#31551=DIRECTION('ref_axis',(0.939692620785908,0.,-0.342020143325669));
#31552=DIRECTION('',(-0.939692620785908,0.,0.342020143325669));
#31553=DIRECTION('',(0.633687274224663,0.633687274224675,0.443712606279581));
#31554=DIRECTION('',(0.939692620785908,0.,-0.342020143325669));
#31555=DIRECTION('',(0.633687274224686,0.633687274224686,0.443712606279532));
#31556=DIRECTION('center_axis',(-0.342020143325669,0.,-0.939692620785908));
#31557=DIRECTION('ref_axis',(-0.939692620785908,0.,0.342020143325669));
#31558=DIRECTION('',(0.939692620785908,0.,-0.342020143325669));
#31559=DIRECTION('',(0.,1.,0.));
#31560=DIRECTION('center_axis',(0.24184476264798,0.707106781186534,0.664463024388687));
#31561=DIRECTION('ref_axis',(0.939692620785908,0.,-0.342020143325669));
#31562=DIRECTION('',(-0.633687274224649,0.633687274224649,-0.443712606279638));
#31563=DIRECTION('',(-0.939692620785908,0.,0.342020143325669));
#31564=DIRECTION('',(-0.633687274224652,0.633687274224654,-0.443712606279627));
#31565=DIRECTION('center_axis',(0.819152044289004,0.,0.573576436351029));
#31566=DIRECTION('ref_axis',(0.573576436351029,0.,-0.819152044289004));
#31567=DIRECTION('',(0.497542812164512,0.497542812164512,-0.710564775461646));
#31568=DIRECTION('',(0.,1.,0.));
#31569=DIRECTION('',(-0.497542812164512,0.497542812164512,0.710564775461646));
#31570=DIRECTION('',(-0.497542812164502,-0.497542812164542,0.710564775461631));
#31571=DIRECTION('',(0.,-1.,0.));
#31572=DIRECTION('',(0.497542812164501,-0.497542812164543,-0.710564775461631));
#31573=DIRECTION('center_axis',(0.241844762647986,0.707106781186536,0.664463024388684));
#31574=DIRECTION('ref_axis',(0.939692620785905,0.,-0.342020143325678));
#31575=DIRECTION('',(-0.63368727422465,0.63368727422465,-0.443712606279636));
#31576=DIRECTION('',(-0.939692620785905,0.,0.342020143325678));
#31577=DIRECTION('',(-0.633687274224657,0.633687274224651,-0.443712606279624));
#31578=DIRECTION('',(0.939692620785905,0.,-0.342020143325678));
#31579=DIRECTION('center_axis',(0.707106781186548,0.707106781186548,0.));
#31580=DIRECTION('ref_axis',(0.,0.,-1.));
#31581=DIRECTION('',(0.,0.,-1.));
#31582=DIRECTION('',(0.497542812164512,-0.497542812164512,0.710564775461646));
#31583=DIRECTION('',(0.633687274224648,-0.633687274224648,-0.44371260627964));
#31584=DIRECTION('',(0.,0.,1.));
#31585=DIRECTION('center_axis',(1.,0.,0.));
#31586=DIRECTION('ref_axis',(0.,1.,0.));
#31587=DIRECTION('',(0.,0.,1.));
#31588=DIRECTION('',(0.,-1.,0.));
#31589=DIRECTION('center_axis',(0.819152044289004,0.,-0.573576436351029));
#31590=DIRECTION('ref_axis',(-0.573576436351029,0.,-0.819152044289004));
#31591=DIRECTION('',(-0.497542812164512,-0.497542812164512,-0.710564775461646));
#31592=DIRECTION('',(-0.497542812164515,0.497542812164502,-0.71056477546165));
#31593=DIRECTION('',(0.,1.,0.));
#31594=DIRECTION('',(0.497542812164503,0.497542812164539,0.710564775461633));
#31595=DIRECTION('center_axis',(0.241844762647985,0.707106781186538,-0.664463024388682));
#31596=DIRECTION('ref_axis',(-0.939692620785905,0.,-0.342020143325678));
#31597=DIRECTION('',(-0.939692620785905,0.,-0.342020143325678));
#31598=DIRECTION('',(-0.633687274224634,0.633687274224638,0.443712606279675));
#31599=DIRECTION('',(0.939692620785905,0.,0.342020143325678));
#31600=DIRECTION('center_axis',(0.819152044289007,0.,0.573576436351024));
#31601=DIRECTION('ref_axis',(0.573576436351024,0.,-0.819152044289007));
#31602=DIRECTION('',(0.497542812164509,0.497542812164509,-0.71056477546165));
#31603=DIRECTION('',(0.,1.,0.));
#31604=DIRECTION('',(-0.497542812164509,0.497542812164509,0.71056477546165));
#31605=DIRECTION('',(-0.497542812164497,-0.497542812164545,0.710564775461633));
#31606=DIRECTION('',(0.,-1.,0.));
#31607=DIRECTION('',(0.497542812164509,-0.497542812164509,-0.71056477546165));
#31608=DIRECTION('center_axis',(0.241844762647986,0.707106781186536,0.664463024388684));
#31609=DIRECTION('ref_axis',(0.939692620785905,0.,-0.342020143325678));
#31610=DIRECTION('',(-0.63368727422465,0.63368727422465,-0.443712606279636));
#31611=DIRECTION('',(-0.939692620785905,0.,0.342020143325678));
#31612=DIRECTION('',(-0.633687274224657,0.633687274224651,-0.443712606279624));
#31613=DIRECTION('',(0.939692620785905,0.,-0.342020143325678));
#31614=DIRECTION('center_axis',(0.707106781186548,0.707106781186548,0.));
#31615=DIRECTION('ref_axis',(0.,0.,-1.));
#31616=DIRECTION('',(0.,0.,-1.));
#31617=DIRECTION('',(0.497542812164539,-0.497542812164539,0.710564775461607));
#31618=DIRECTION('',(0.63368727422465,-0.63368727422465,-0.443712606279635));
#31619=DIRECTION('',(0.,0.,1.));
#31620=DIRECTION('center_axis',(1.,0.,0.));
#31621=DIRECTION('ref_axis',(0.,1.,0.));
#31622=DIRECTION('',(0.,0.,1.));
#31623=DIRECTION('',(0.,-1.,0.));
#31624=DIRECTION('center_axis',(0.819152044288975,0.,-0.573576436351071));
#31625=DIRECTION('ref_axis',(-0.573576436351071,0.,-0.819152044288975));
#31626=DIRECTION('',(-0.497542812164539,-0.497542812164539,-0.710564775461607));
#31627=DIRECTION('',(-0.497542812164545,0.497542812164519,-0.710564775461617));
#31628=DIRECTION('',(0.,1.,0.));
#31629=DIRECTION('',(0.497542812164545,0.497542812164522,0.710564775461615));
#31630=DIRECTION('center_axis',(0.24184476264798,0.707106781186533,-0.664463024388688));
#31631=DIRECTION('ref_axis',(-0.939692620785908,0.,-0.342020143325669));
#31632=DIRECTION('',(-0.939692620785908,0.,-0.342020143325669));
#31633=DIRECTION('',(-0.633687274224651,0.633687274224655,0.443712606279627));
#31634=DIRECTION('',(0.939692620785908,0.,0.342020143325669));
#31635=DIRECTION('center_axis',(0.819152044289004,0.,0.573576436351029));
#31636=DIRECTION('ref_axis',(0.573576436351029,0.,-0.819152044289004));
#31637=DIRECTION('',(0.,1.,0.));
#31638=DIRECTION('',(-0.497542812164512,0.497542812164512,0.710564775461646));
#31639=DIRECTION('',(-0.497542812164502,-0.497542812164542,0.710564775461631));
#31640=DIRECTION('',(0.,-1.,0.));
#31641=DIRECTION('',(0.497542812164501,-0.497542812164543,-0.710564775461631));
#31642=DIRECTION('center_axis',(0.241844762647986,-0.707106781186534,0.664463024388685));
#31643=DIRECTION('ref_axis',(0.939692620785905,0.,-0.342020143325678));
#31644=DIRECTION('',(-0.939692620785905,0.,0.342020143325678));
#31645=DIRECTION('',(0.633687274224652,0.633687274224654,0.443712606279627));
#31646=DIRECTION('',(0.939692620785905,0.,-0.342020143325678));
#31647=DIRECTION('center_axis',(-0.342020143325678,0.,-0.939692620785905));
#31648=DIRECTION('ref_axis',(-0.939692620785905,0.,0.342020143325678));
#31649=DIRECTION('',(0.939692620785905,0.,-0.342020143325678));
#31650=DIRECTION('',(0.,1.,0.));
#31651=DIRECTION('center_axis',(0.241844762647986,0.707106781186536,0.664463024388684));
#31652=DIRECTION('ref_axis',(0.939692620785905,0.,-0.342020143325678));
#31653=DIRECTION('',(-0.63368727422465,0.63368727422465,-0.443712606279636));
#31654=DIRECTION('',(-0.939692620785905,0.,0.342020143325678));
#31655=DIRECTION('',(-0.633687274224657,0.633687274224651,-0.443712606279624));
#31656=DIRECTION('center_axis',(0.382683432365109,0.,-0.923879532511279));
#31657=DIRECTION('ref_axis',(-0.923879532511279,0.,-0.382683432365109));
#31658=DIRECTION('',(0.862856209461003,0.357406744336612,0.357406744336608));
#31659=DIRECTION('',(0.,-1.,0.));
#31660=DIRECTION('',(-0.862856209461003,0.357406744336612,-0.357406744336608));
#31661=DIRECTION('',(0.,1.,0.));
#31662=DIRECTION('center_axis',(0.,0.,1.));
#31663=DIRECTION('ref_axis',(1.,0.,0.));
#31664=DIRECTION('',(1.,0.,0.));
#31665=DIRECTION('',(0.,-1.,0.));
#31666=DIRECTION('',(-1.,0.,0.));
#31667=DIRECTION('center_axis',(0.,0.,-1.));
#31668=DIRECTION('ref_axis',(1.,0.,0.));
#31669=DIRECTION('center_axis',(0.,-0.707106781186544,-0.707106781186551));
#31670=DIRECTION('ref_axis',(-1.,0.,0.));
#31671=DIRECTION('',(0.577350269189628,-0.577350269189628,0.577350269189622));
#31672=DIRECTION('',(1.,0.,0.));
#31673=DIRECTION('',(-0.577350269189628,-0.577350269189628,0.577350269189622));
#31674=DIRECTION('',(-0.862856209461003,-0.357406744336612,0.357406744336608));
#31675=DIRECTION('center_axis',(-0.923879532511285,0.,-0.382683432365094));
#31676=DIRECTION('ref_axis',(-0.382683432365094,0.,0.923879532511285));
#31677=DIRECTION('',(0.357406744336596,-0.357406744336596,-0.862856209461014));
#31678=DIRECTION('',(0.,-1.,0.));
#31679=DIRECTION('',(-0.357406744336596,-0.357406744336596,0.862856209461014));
#31680=DIRECTION('',(-0.357406744336596,0.357406744336596,0.862856209461014));
#31681=DIRECTION('',(0.,1.,0.));
#31682=DIRECTION('',(0.357406744336596,0.357406744336596,-0.862856209461014));
#31683=DIRECTION('center_axis',(-0.707106781186544,0.,-0.707106781186551));
#31684=DIRECTION('ref_axis',(-0.707106781186551,0.,0.707106781186544));
#31685=DIRECTION('',(0.577350269189628,-0.577350269189628,-0.577350269189622));
#31686=DIRECTION('',(0.,1.,0.));
#31687=DIRECTION('center_axis',(0.,0.923879532511285,-0.382683432365094));
#31688=DIRECTION('ref_axis',(0.,0.382683432365094,0.923879532511285));
#31689=DIRECTION('',(0.357406744336596,0.357406744336596,0.862856209461014));
#31690=DIRECTION('',(1.,0.,0.));
#31691=DIRECTION('',(0.357406744336596,-0.357406744336596,-0.862856209461014));
#31692=DIRECTION('',(-0.67859834454585,-0.281084637714822,-0.678598344545844));
#31693=DIRECTION('',(-1.,0.,0.));
#31694=DIRECTION('center_axis',(-0.707106781186548,0.707106781186548,0.));
#31695=DIRECTION('ref_axis',(0.,0.,1.));
#31696=DIRECTION('',(0.,0.,1.));
#31697=DIRECTION('',(-0.357406744336592,-0.357406744336592,-0.862856209461018));
#31698=DIRECTION('',(-0.357406744336592,-0.357406744336592,0.862856209461018));
#31699=DIRECTION('',(0.,0.,-1.));
#31700=DIRECTION('center_axis',(-0.382683432365109,0.,-0.923879532511279));
#31701=DIRECTION('ref_axis',(-0.923879532511279,0.,0.382683432365109));
#31702=DIRECTION('',(0.862856209461003,-0.357406744336612,-0.357406744336608));
#31703=DIRECTION('center_axis',(0.923879532511288,0.,0.382683432365088));
#31704=DIRECTION('ref_axis',(0.382683432365088,0.,-0.923879532511288));
#31705=DIRECTION('',(-0.357406744336592,-0.357406744336592,0.862856209461018));
#31706=DIRECTION('',(0.,-1.,0.));
#31707=DIRECTION('',(0.357406744336592,-0.357406744336592,-0.862856209461018));
#31708=DIRECTION('',(0.357406744336592,0.357406744336592,-0.862856209461018));
#31709=DIRECTION('',(0.,1.,0.));
#31710=DIRECTION('',(-0.357406744336592,0.357406744336592,0.862856209461018));
#31711=DIRECTION('center_axis',(0.,0.923879532511288,0.382683432365088));
#31712=DIRECTION('ref_axis',(0.,-0.382683432365088,0.923879532511288));
#31713=DIRECTION('',(-0.357406744336592,0.357406744336592,-0.862856209461018));
#31714=DIRECTION('',(-1.,0.,0.));
#31715=DIRECTION('',(-0.357406744336592,0.357406744336592,-0.862856209461018));
#31716=DIRECTION('',(1.,0.,0.));
#31717=DIRECTION('center_axis',(0.707106781186548,0.707106781186548,0.));
#31718=DIRECTION('ref_axis',(0.,0.,-1.));
#31719=DIRECTION('',(0.,0.,-1.));
#31720=DIRECTION('',(0.497542812164509,-0.497542812164509,0.71056477546165));
#31721=DIRECTION('',(0.633687274224649,-0.633687274224649,-0.443712606279638));
#31722=DIRECTION('',(0.,0.,1.));
#31723=DIRECTION('center_axis',(1.,0.,0.));
#31724=DIRECTION('ref_axis',(0.,1.,0.));
#31725=DIRECTION('',(0.,0.,1.));
#31726=DIRECTION('',(0.,-1.,0.));
#31727=DIRECTION('center_axis',(0.819152044289009,0.,0.573576436351022));
#31728=DIRECTION('ref_axis',(0.573576436351022,0.,-0.819152044289009));
#31729=DIRECTION('',(0.497542812164507,0.497542812164507,-0.710564775461652));
#31730=DIRECTION('',(0.,1.,0.));
#31731=DIRECTION('',(-0.497542812164507,0.497542812164507,0.710564775461652));
#31732=DIRECTION('',(-0.497542812164506,-0.49754281216451,0.710564775461651));
#31733=DIRECTION('',(0.,-1.,0.));
#31734=DIRECTION('',(0.497542812164493,-0.497542812164548,-0.710564775461633));
#31735=DIRECTION('center_axis',(0.241844762647974,0.70710678118657,0.664463024388651));
#31736=DIRECTION('ref_axis',(0.939692620785905,0.,-0.342020143325678));
#31737=DIRECTION('',(-0.633687274224631,0.633687274224631,-0.443712606279689));
#31738=DIRECTION('',(-0.939692620785905,0.,0.342020143325678));
#31739=DIRECTION('',(-0.633687274224635,0.633687274224637,-0.443712606279675));
#31740=DIRECTION('',(0.939692620785905,0.,-0.342020143325678));
#31741=DIRECTION('center_axis',(0.707106781186548,0.707106781186548,0.));
#31742=DIRECTION('ref_axis',(0.,0.,-1.));
#31743=DIRECTION('',(0.,0.,-1.));
#31744=DIRECTION('',(0.497542812164534,-0.497542812164534,0.710564775461614));
#31745=DIRECTION('',(0.633687274224667,-0.633687274224667,-0.443712606279587));
#31746=DIRECTION('',(0.,0.,1.));
#31747=DIRECTION('center_axis',(1.,0.,0.));
#31748=DIRECTION('ref_axis',(0.,1.,0.));
#31749=DIRECTION('',(0.,0.,1.));
#31750=DIRECTION('',(0.,-1.,0.));
#31751=DIRECTION('center_axis',(0.81915204428898,0.,-0.573576436351063));
#31752=DIRECTION('ref_axis',(-0.573576436351063,0.,-0.81915204428898));
#31753=DIRECTION('',(-0.497542812164534,-0.497542812164534,-0.710564775461614));
#31754=DIRECTION('',(-0.497542812164537,0.497542812164526,-0.710564775461618));
#31755=DIRECTION('',(0.,1.,0.));
#31756=DIRECTION('',(0.497542812164526,0.49754281216456,0.710564775461602));
#31757=DIRECTION('center_axis',(0.241844762647991,0.707106781186501,-0.664463024388718));
#31758=DIRECTION('ref_axis',(-0.939692620785908,0.,-0.342020143325669));
#31759=DIRECTION('',(-0.939692620785908,0.,-0.342020143325669));
#31760=DIRECTION('',(-0.633687274224651,0.633687274224655,0.443712606279627));
#31761=DIRECTION('',(0.939692620785908,0.,0.342020143325669));
#31762=DIRECTION('center_axis',(0.819152044289004,0.,0.573576436351029));
#31763=DIRECTION('ref_axis',(0.573576436351029,0.,-0.819152044289004));
#31764=DIRECTION('',(0.497542812164512,0.497542812164512,-0.710564775461646));
#31765=DIRECTION('',(0.,1.,0.));
#31766=DIRECTION('',(-0.497542812164512,0.497542812164512,0.710564775461646));
#31767=DIRECTION('',(-0.497542812164501,-0.497542812164543,0.710564775461631));
#31768=DIRECTION('',(0.,-1.,0.));
#31769=DIRECTION('',(0.49754281216449,-0.497542812164577,-0.710564775461615));
#31770=DIRECTION('center_axis',(0.241844762647986,0.707106781186534,0.664463024388685));
#31771=DIRECTION('ref_axis',(0.939692620785905,0.,-0.342020143325678));
#31772=DIRECTION('',(-0.63368727422465,0.63368727422465,-0.443712606279634));
#31773=DIRECTION('',(-0.939692620785905,0.,0.342020143325678));
#31774=DIRECTION('',(-0.633687274224652,0.633687274224654,-0.443712606279627));
#31775=DIRECTION('',(0.939692620785905,0.,-0.342020143325678));
#31776=DIRECTION('center_axis',(0.707106781186548,0.707106781186548,0.));
#31777=DIRECTION('ref_axis',(0.,0.,-1.));
#31778=DIRECTION('',(0.,0.,-1.));
#31779=DIRECTION('',(0.497542812164509,-0.497542812164509,0.71056477546165));
#31780=DIRECTION('',(0.633687274224631,-0.633687274224631,-0.443712606279689));
#31781=DIRECTION('',(0.,0.,1.));
#31782=DIRECTION('center_axis',(1.,0.,0.));
#31783=DIRECTION('ref_axis',(0.,1.,0.));
#31784=DIRECTION('',(0.,0.,1.));
#31785=DIRECTION('',(0.,-1.,0.));
#31786=DIRECTION('center_axis',(0.819152044289007,0.,-0.573576436351024));
#31787=DIRECTION('ref_axis',(-0.573576436351024,0.,-0.819152044289007));
#31788=DIRECTION('',(-0.497542812164509,-0.497542812164509,-0.71056477546165));
#31789=DIRECTION('',(-0.497542812164497,0.497542812164543,-0.710564775461634));
#31790=DIRECTION('',(0.,1.,0.));
#31791=DIRECTION('',(0.497542812164509,0.497542812164509,0.71056477546165));
#31792=DIRECTION('center_axis',(0.241844762647974,0.70710678118657,-0.664463024388651));
#31793=DIRECTION('ref_axis',(-0.939692620785905,0.,-0.342020143325678));
#31794=DIRECTION('',(-0.939692620785905,0.,-0.342020143325678));
#31795=DIRECTION('',(-0.633687274224634,0.633687274224638,0.443712606279675));
#31796=DIRECTION('',(0.939692620785905,0.,0.342020143325678));
#31797=DIRECTION('center_axis',(0.819152044289007,0.,0.573576436351024));
#31798=DIRECTION('ref_axis',(0.573576436351024,0.,-0.819152044289007));
#31799=DIRECTION('',(0.497542812164509,0.497542812164509,-0.71056477546165));
#31800=DIRECTION('',(0.,1.,0.));
#31801=DIRECTION('',(-0.497542812164509,0.497542812164509,0.71056477546165));
#31802=DIRECTION('',(-0.497542812164497,-0.497542812164545,0.710564775461633));
#31803=DIRECTION('',(0.,-1.,0.));
#31804=DIRECTION('',(0.497542812164498,-0.497542812164542,-0.710564775461634));
#31805=DIRECTION('center_axis',(0.241844762647986,0.707106781186536,0.664463024388684));
#31806=DIRECTION('ref_axis',(0.939692620785905,0.,-0.342020143325678));
#31807=DIRECTION('',(-0.63368727422465,0.63368727422465,-0.443712606279636));
#31808=DIRECTION('',(-0.939692620785905,0.,0.342020143325678));
#31809=DIRECTION('',(-0.633687274224652,0.633687274224654,-0.443712606279627));
#31810=DIRECTION('',(0.939692620785905,0.,-0.342020143325678));
#31811=DIRECTION('center_axis',(0.707106781186548,0.707106781186548,0.));
#31812=DIRECTION('ref_axis',(0.,0.,-1.));
#31813=DIRECTION('',(0.,0.,-1.));
#31814=DIRECTION('',(0.497542812164515,-0.497542812164515,0.710564775461641));
#31815=DIRECTION('',(0.633687274224629,-0.633687274224629,-0.443712606279694));
#31816=DIRECTION('',(0.,0.,1.));
#31817=DIRECTION('center_axis',(1.,0.,0.));
#31818=DIRECTION('ref_axis',(0.,1.,0.));
#31819=DIRECTION('',(0.,0.,1.));
#31820=DIRECTION('',(0.,-1.,0.));
#31821=DIRECTION('center_axis',(0.819152044289001,0.,-0.573576436351034));
#31822=DIRECTION('ref_axis',(-0.573576436351034,0.,-0.819152044289001));
#31823=DIRECTION('',(-0.497542812164515,-0.497542812164515,-0.710564775461641));
#31824=DIRECTION('',(-0.49754281216452,0.497542812164499,-0.710564775461649));
#31825=DIRECTION('',(0.,1.,0.));
#31826=DIRECTION('',(0.49754281216452,0.497542812164498,0.710564775461649));
#31827=DIRECTION('center_axis',(0.241844762647973,0.707106781186574,-0.664463024388648));
#31828=DIRECTION('ref_axis',(-0.939692620785905,0.,-0.342020143325678));
#31829=DIRECTION('',(-0.939692620785905,0.,-0.342020143325678));
#31830=DIRECTION('',(-0.633687274224617,0.633687274224621,0.443712606279724));
#31831=DIRECTION('',(0.939692620785905,0.,0.342020143325678));
#31832=DIRECTION('center_axis',(0.819152044289033,0.,0.573576436350987));
#31833=DIRECTION('ref_axis',(0.573576436350987,0.,-0.819152044289033));
#31834=DIRECTION('',(0.497542812164485,0.497542812164485,-0.710564775461684));
#31835=DIRECTION('',(0.,1.,0.));
#31836=DIRECTION('',(-0.497542812164485,0.497542812164485,0.710564775461684));
#31837=DIRECTION('',(-0.497542812164469,-0.497542812164533,0.710564775461661));
#31838=DIRECTION('',(0.,-1.,0.));
#31839=DIRECTION('',(0.497542812164469,-0.497542812164533,-0.710564775461661));
#31840=DIRECTION('center_axis',(0.241844762647974,0.70710678118657,0.664463024388651));
#31841=DIRECTION('ref_axis',(0.939692620785905,0.,-0.342020143325678));
#31842=DIRECTION('',(-0.633687274224631,0.633687274224631,-0.443712606279689));
#31843=DIRECTION('',(-0.939692620785905,0.,0.342020143325678));
#31844=DIRECTION('',(-0.63368727422464,0.633687274224634,-0.443712606279673));
#31845=DIRECTION('',(0.939692620785905,0.,-0.342020143325678));
#31846=DIRECTION('center_axis',(0.707106781186548,0.707106781186548,0.));
#31847=DIRECTION('ref_axis',(0.,0.,-1.));
#31848=DIRECTION('',(0.,0.,-1.));
#31849=DIRECTION('',(0.497542812164539,-0.497542812164539,0.710564775461607));
#31850=DIRECTION('',(0.63368727422465,-0.63368727422465,-0.443712606279635));
#31851=DIRECTION('',(0.,0.,1.));
#31852=DIRECTION('center_axis',(1.,0.,0.));
#31853=DIRECTION('ref_axis',(0.,1.,0.));
#31854=DIRECTION('',(0.,0.,1.));
#31855=DIRECTION('',(0.,-1.,0.));
#31856=DIRECTION('center_axis',(0.819152044288975,0.,-0.573576436351071));
#31857=DIRECTION('ref_axis',(-0.573576436351071,0.,-0.819152044288975));
#31858=DIRECTION('',(-0.497542812164539,-0.497542812164539,-0.710564775461607));
#31859=DIRECTION('',(-0.497542812164545,0.497542812164521,-0.710564775461616));
#31860=DIRECTION('',(0.,1.,0.));
#31861=DIRECTION('',(0.497542812164545,0.497542812164522,0.710564775461615));
#31862=DIRECTION('center_axis',(0.24184476264798,0.707106781186533,-0.664463024388688));
#31863=DIRECTION('ref_axis',(-0.939692620785908,0.,-0.342020143325669));
#31864=DIRECTION('',(-0.939692620785908,0.,-0.342020143325669));
#31865=DIRECTION('',(-0.633687274224651,0.633687274224655,0.443712606279627));
#31866=DIRECTION('',(0.939692620785908,0.,0.342020143325669));
#31867=DIRECTION('center_axis',(0.819152044289007,0.,0.573576436351024));
#31868=DIRECTION('ref_axis',(0.573576436351024,0.,-0.819152044289007));
#31869=DIRECTION('',(0.497542812164509,0.497542812164509,-0.71056477546165));
#31870=DIRECTION('',(0.,1.,0.));
#31871=DIRECTION('',(-0.497542812164509,0.497542812164509,0.71056477546165));
#31872=DIRECTION('',(-0.497542812164497,-0.497542812164545,0.710564775461633));
#31873=DIRECTION('',(0.,-1.,0.));
#31874=DIRECTION('',(0.497542812164496,-0.497542812164546,-0.710564775461632));
#31875=DIRECTION('center_axis',(-0.342020143325678,0.,-0.939692620785905));
#31876=DIRECTION('ref_axis',(-0.939692620785905,0.,0.342020143325678));
#31877=DIRECTION('',(0.939692620785905,0.,-0.342020143325678));
#31878=DIRECTION('',(0.,1.,0.));
#31879=DIRECTION('',(-0.939692620785905,0.,0.342020143325678));
#31880=DIRECTION('center_axis',(0.241844762647986,0.707106781186536,0.664463024388684));
#31881=DIRECTION('ref_axis',(0.939692620785905,0.,-0.342020143325678));
#31882=DIRECTION('',(-0.63368727422465,0.63368727422465,-0.443712606279636));
#31883=DIRECTION('',(-0.939692620785905,0.,0.342020143325678));
#31884=DIRECTION('',(-0.633687274224652,0.633687274224654,-0.443712606279627));
#31885=DIRECTION('center_axis',(0.707106781186548,0.707106781186548,0.));
#31886=DIRECTION('ref_axis',(0.,0.,-1.));
#31887=DIRECTION('',(0.,0.,1.));
#31888=DIRECTION('',(0.,0.,-1.));
#31889=DIRECTION('center_axis',(0.70710678118655,0.707106781186545,0.));
#31890=DIRECTION('ref_axis',(0.,0.,-1.));
#31891=DIRECTION('',(0.,0.,1.));
#31892=DIRECTION('',(0.,0.,-1.));
#31893=DIRECTION('center_axis',(-1.,0.,0.));
#31894=DIRECTION('ref_axis',(0.,0.,1.));
#31895=DIRECTION('',(0.,1.,0.));
#31896=DIRECTION('',(0.,0.,1.));
#31897=DIRECTION('center_axis',(-0.342020143325669,0.,0.939692620785908));
#31898=DIRECTION('ref_axis',(0.939692620785908,0.,0.342020143325669));
#31899=DIRECTION('',(0.939692620785908,0.,0.342020143325669));
#31900=DIRECTION('center_axis',(0.70710678118655,0.707106781186545,0.));
#31901=DIRECTION('ref_axis',(0.,0.,-1.));
#31902=DIRECTION('',(0.,0.,1.));
#31903=DIRECTION('',(0.,0.,-1.));
#31904=DIRECTION('center_axis',(-0.342020143325678,0.,-0.939692620785905));
#31905=DIRECTION('ref_axis',(-0.939692620785905,0.,0.342020143325678));
#31906=DIRECTION('',(0.,1.,0.));
#31907=DIRECTION('',(-0.939692620785905,0.,0.342020143325678));
#31908=DIRECTION('center_axis',(-1.,0.,0.));
#31909=DIRECTION('ref_axis',(0.,0.,1.));
#31910=DIRECTION('',(0.,1.,0.));
#31911=DIRECTION('',(0.,0.,1.));
#31912=DIRECTION('center_axis',(-0.342020143325678,0.,0.939692620785905));
#31913=DIRECTION('ref_axis',(0.939692620785905,0.,0.342020143325678));
#31914=DIRECTION('',(0.939692620785905,0.,0.342020143325678));
#31915=DIRECTION('center_axis',(0.70710678118655,0.707106781186545,0.));
#31916=DIRECTION('ref_axis',(0.,0.,-1.));
#31917=DIRECTION('',(0.,0.,1.));
#31918=DIRECTION('',(0.,0.,-1.));
#31919=DIRECTION('center_axis',(-0.342020143325678,0.,-0.939692620785905));
#31920=DIRECTION('ref_axis',(-0.939692620785905,0.,0.342020143325678));
#31921=DIRECTION('',(0.,1.,0.));
#31922=DIRECTION('',(-0.939692620785905,0.,0.342020143325678));
#31923=DIRECTION('center_axis',(-1.,0.,0.));
#31924=DIRECTION('ref_axis',(0.,0.,1.));
#31925=DIRECTION('',(0.,0.,1.));
#31926=DIRECTION('center_axis',(0.,1.,0.));
#31927=DIRECTION('ref_axis',(-1.,0.,0.));
#31928=DIRECTION('',(0.,0.,1.));
#31929=DIRECTION('',(0.939692620785905,0.,0.342020143325678));
#31930=DIRECTION('',(0.,0.,1.));
#31931=DIRECTION('',(-0.939692620785905,0.,0.342020143325678));
#31932=DIRECTION('',(0.,0.,1.));
#31933=DIRECTION('',(0.939692620785905,0.,0.342020143325678));
#31934=DIRECTION('',(0.,0.,1.));
#31935=DIRECTION('',(-0.939692620785905,0.,0.342020143325678));
#31936=DIRECTION('',(0.,0.,1.));
#31937=DIRECTION('',(0.939692620785908,0.,0.342020143325669));
#31938=DIRECTION('',(0.,0.,1.));
#31939=DIRECTION('',(-0.939692620785905,0.,0.342020143325678));
#31940=DIRECTION('',(0.,0.,1.));
#31941=DIRECTION('',(0.939692620785905,0.,0.342020143325678));
#31942=DIRECTION('',(0.,0.,1.));
#31943=DIRECTION('',(-0.939692620785905,0.,0.342020143325678));
#31944=DIRECTION('',(0.,0.,1.));
#31945=DIRECTION('',(0.939692620785905,0.,0.342020143325678));
#31946=DIRECTION('',(0.,0.,1.));
#31947=DIRECTION('',(-0.939692620785905,0.,0.342020143325678));
#31948=DIRECTION('',(0.,0.,1.));
#31949=DIRECTION('',(0.939692620785905,0.,0.342020143325678));
#31950=DIRECTION('',(0.,0.,1.));
#31951=DIRECTION('',(-0.939692620785908,0.,0.342020143325669));
#31952=DIRECTION('',(0.,0.,1.));
#31953=DIRECTION('',(0.939692620785908,0.,0.342020143325669));
#31954=DIRECTION('',(0.,0.,1.));
#31955=DIRECTION('',(-0.939692620785908,0.,0.342020143325669));
#31956=DIRECTION('',(0.,0.,1.));
#31957=DIRECTION('',(0.,0.,1.));
#31958=DIRECTION('',(0.,0.,1.));
#31959=DIRECTION('',(-0.939692620785908,0.,0.342020143325669));
#31960=DIRECTION('',(0.,0.,1.));
#31961=DIRECTION('',(0.939692620785908,0.,0.342020143325669));
#31962=DIRECTION('',(0.,0.,1.));
#31963=DIRECTION('',(-0.939692620785908,0.,0.342020143325669));
#31964=DIRECTION('',(0.,0.,1.));
#31965=DIRECTION('',(0.939692620785908,0.,0.342020143325669));
#31966=DIRECTION('',(0.,0.,1.));
#31967=DIRECTION('',(-0.939692620785908,0.,0.342020143325669));
#31968=DIRECTION('',(0.,0.,1.));
#31969=DIRECTION('',(0.939692620785908,0.,0.342020143325669));
#31970=DIRECTION('',(0.,0.,1.));
#31971=DIRECTION('',(-0.939692620785908,0.,0.342020143325669));
#31972=DIRECTION('',(0.,0.,1.));
#31973=DIRECTION('',(0.939692620785908,0.,0.342020143325669));
#31974=DIRECTION('',(0.,0.,1.));
#31975=DIRECTION('',(-0.939692620785908,0.,0.342020143325669));
#31976=DIRECTION('',(0.,0.,1.));
#31977=DIRECTION('',(0.939692620785908,0.,0.342020143325669));
#31978=DIRECTION('',(0.,0.,1.));
#31979=DIRECTION('',(-0.939692620785908,0.,0.342020143325669));
#31980=DIRECTION('',(0.,0.,1.));
#31981=DIRECTION('',(0.939692620785908,0.,0.342020143325669));
#31982=DIRECTION('',(0.,0.,1.));
#31983=DIRECTION('',(-0.939692620785908,0.,0.342020143325669));
#31984=DIRECTION('',(0.,0.,1.));
#31985=DIRECTION('',(0.,0.,1.));
#31986=DIRECTION('',(0.,0.,1.));
#31987=DIRECTION('',(0.,0.,1.));
#31988=DIRECTION('',(0.939692620785908,0.,0.342020143325669));
#31989=DIRECTION('',(0.,0.,1.));
#31990=DIRECTION('',(0.,0.,1.));
#31991=DIRECTION('',(0.,0.,1.));
#31992=DIRECTION('',(0.,0.,1.));
#31993=DIRECTION('',(0.939692620785908,0.,0.342020143325669));
#31994=DIRECTION('',(0.,0.,1.));
#31995=DIRECTION('',(-0.939692620785908,0.,0.342020143325669));
#31996=DIRECTION('',(0.,0.,1.));
#31997=DIRECTION('',(0.939692620785905,0.,0.342020143325678));
#31998=DIRECTION('',(0.,0.,1.));
#31999=DIRECTION('',(0.,0.,1.));
#32000=DIRECTION('',(0.,0.,1.));
#32001=DIRECTION('',(0.,0.,1.));
#32002=DIRECTION('',(0.,0.,1.));
#32003=DIRECTION('center_axis',(0.70710678118655,0.707106781186545,0.));
#32004=DIRECTION('ref_axis',(0.,0.,-1.));
#32005=DIRECTION('',(0.,0.,-1.));
#32006=DIRECTION('center_axis',(-1.,0.,0.));
#32007=DIRECTION('ref_axis',(0.,0.,1.));
#32008=DIRECTION('',(0.,1.,0.));
#32009=DIRECTION('',(0.,0.,1.));
#32010=DIRECTION('center_axis',(-0.342020143325669,0.,0.939692620785908));
#32011=DIRECTION('ref_axis',(0.939692620785908,0.,0.342020143325669));
#32012=DIRECTION('',(0.939692620785908,0.,0.342020143325669));
#32013=DIRECTION('center_axis',(0.70710678118655,0.707106781186545,0.));
#32014=DIRECTION('ref_axis',(0.,0.,-1.));
#32015=DIRECTION('',(0.,0.,-1.));
#32016=DIRECTION('center_axis',(-0.342020143325678,0.,-0.939692620785905));
#32017=DIRECTION('ref_axis',(-0.939692620785905,0.,0.342020143325678));
#32018=DIRECTION('',(0.,1.,0.));
#32019=DIRECTION('',(-0.939692620785905,0.,0.342020143325678));
#32020=DIRECTION('center_axis',(-1.,0.,0.));
#32021=DIRECTION('ref_axis',(0.,0.,1.));
#32022=DIRECTION('',(0.,1.,0.));
#32023=DIRECTION('',(0.,0.,1.));
#32024=DIRECTION('center_axis',(-0.342020143325678,0.,0.939692620785905));
#32025=DIRECTION('ref_axis',(0.939692620785905,0.,0.342020143325678));
#32026=DIRECTION('',(0.939692620785905,0.,0.342020143325678));
#32027=DIRECTION('center_axis',(0.70710678118655,0.707106781186545,0.));
#32028=DIRECTION('ref_axis',(0.,0.,-1.));
#32029=DIRECTION('',(0.,0.,-1.));
#32030=DIRECTION('center_axis',(-0.342020143325678,0.,-0.939692620785905));
#32031=DIRECTION('ref_axis',(-0.939692620785905,0.,0.342020143325678));
#32032=DIRECTION('',(0.,1.,0.));
#32033=DIRECTION('',(-0.939692620785905,0.,0.342020143325678));
#32034=DIRECTION('center_axis',(-1.,0.,0.));
#32035=DIRECTION('ref_axis',(0.,0.,1.));
#32036=DIRECTION('',(0.,1.,0.));
#32037=DIRECTION('',(0.,0.,1.));
#32038=DIRECTION('center_axis',(-0.342020143325678,0.,0.939692620785905));
#32039=DIRECTION('ref_axis',(0.939692620785905,0.,0.342020143325678));
#32040=DIRECTION('',(0.939692620785905,0.,0.342020143325678));
#32041=DIRECTION('center_axis',(0.70710678118655,0.707106781186545,0.));
#32042=DIRECTION('ref_axis',(0.,0.,-1.));
#32043=DIRECTION('',(0.,0.,-1.));
#32044=DIRECTION('center_axis',(-0.342020143325678,0.,-0.939692620785905));
#32045=DIRECTION('ref_axis',(-0.939692620785905,0.,0.342020143325678));
#32046=DIRECTION('',(0.,1.,0.));
#32047=DIRECTION('',(-0.939692620785905,0.,0.342020143325678));
#32048=DIRECTION('center_axis',(-1.,0.,0.));
#32049=DIRECTION('ref_axis',(0.,0.,1.));
#32050=DIRECTION('',(0.,1.,0.));
#32051=DIRECTION('',(0.,0.,1.));
#32052=DIRECTION('center_axis',(-0.342020143325669,0.,0.939692620785908));
#32053=DIRECTION('ref_axis',(0.939692620785908,0.,0.342020143325669));
#32054=DIRECTION('',(0.939692620785908,0.,0.342020143325669));
#32055=DIRECTION('center_axis',(0.70710678118655,0.707106781186545,0.));
#32056=DIRECTION('ref_axis',(0.,0.,-1.));
#32057=DIRECTION('',(-0.633687274224609,0.633687274224613,0.443712606279746));
#32058=DIRECTION('',(0.,0.,-1.));
#32059=DIRECTION('center_axis',(-0.342020143325678,0.,-0.939692620785905));
#32060=DIRECTION('ref_axis',(-0.939692620785905,0.,0.342020143325678));
#32061=DIRECTION('',(0.,1.,0.));
#32062=DIRECTION('',(-0.939692620785905,0.,0.342020143325678));
#32063=DIRECTION('center_axis',(-1.,0.,0.));
#32064=DIRECTION('ref_axis',(0.,0.,1.));
#32065=DIRECTION('',(0.,1.,0.));
#32066=DIRECTION('',(0.,0.,1.));
#32067=DIRECTION('center_axis',(-0.382683432365118,0.,0.923879532511275));
#32068=DIRECTION('ref_axis',(0.923879532511275,0.,0.382683432365118));
#32069=DIRECTION('',(-0.862856209461002,0.357406744336604,-0.357406744336618));
#32070=DIRECTION('',(0.,-1.,0.));
#32071=DIRECTION('',(0.862856209461002,0.357406744336604,0.357406744336618));
#32072=DIRECTION('',(0.,1.,0.));
#32073=DIRECTION('center_axis',(0.,-0.707106781186561,0.707106781186534));
#32074=DIRECTION('ref_axis',(1.,0.,0.));
#32075=DIRECTION('',(-0.577350269189618,-0.577350269189618,-0.577350269189641));
#32076=DIRECTION('',(-1.,0.,0.));
#32077=DIRECTION('',(0.577350269189618,-0.577350269189618,-0.577350269189641));
#32078=DIRECTION('',(-1.,0.,0.));
#32079=DIRECTION('center_axis',(-0.707106781186561,0.,0.707106781186534));
#32080=DIRECTION('ref_axis',(0.707106781186534,0.,0.707106781186561));
#32081=DIRECTION('',(-0.577350269189618,0.577350269189618,-0.577350269189641));
#32082=DIRECTION('',(0.,1.,0.));
#32083=DIRECTION('center_axis',(-0.923879532511288,0.,0.382683432365088));
#32084=DIRECTION('ref_axis',(0.382683432365088,0.,0.923879532511288));
#32085=DIRECTION('',(0.357406744336592,0.357406744336592,0.862856209461018));
#32086=DIRECTION('',(0.,-1.,0.));
#32087=DIRECTION('',(0.357406744336592,-0.357406744336592,0.862856209461018));
#32088=DIRECTION('center_axis',(0.,-0.923879532511288,0.382683432365088));
#32089=DIRECTION('ref_axis',(0.,-0.382683432365088,-0.923879532511288));
#32090=DIRECTION('',(0.357406744336592,-0.357406744336592,-0.862856209461018));
#32091=DIRECTION('',(1.,0.,0.));
#32092=DIRECTION('',(0.357406744336592,0.357406744336592,0.862856209461018));
#32093=DIRECTION('center_axis',(-0.707106781186548,-0.707106781186548,0.));
#32094=DIRECTION('ref_axis',(0.,0.,1.));
#32095=DIRECTION('',(-0.357406744336596,0.357406744336596,-0.862856209461014));
#32096=DIRECTION('',(0.,0.,1.));
#32097=DIRECTION('',(0.,0.,-1.));
#32098=DIRECTION('center_axis',(0.819152044289007,0.,-0.573576436351024));
#32099=DIRECTION('ref_axis',(-0.573576436351024,0.,-0.819152044289007));
#32100=DIRECTION('',(-0.497542812164509,-0.497542812164509,-0.71056477546165));
#32101=DIRECTION('',(-0.49754281216452,0.497542812164474,-0.710564775461666));
#32102=DIRECTION('',(0.,1.,0.));
#32103=DIRECTION('',(0.497542812164495,0.497542812164551,0.71056477546163));
#32104=DIRECTION('center_axis',(0.24184476264798,0.707106781186534,-0.664463024388687));
#32105=DIRECTION('ref_axis',(-0.939692620785908,0.,-0.342020143325669));
#32106=DIRECTION('',(-0.939692620785908,0.,-0.342020143325669));
#32107=DIRECTION('',(-0.633687274224651,0.633687274224655,0.443712606279627));
#32108=DIRECTION('center_axis',(0.819152044289004,0.,0.573576436351029));
#32109=DIRECTION('ref_axis',(0.573576436351029,0.,-0.819152044289004));
#32110=DIRECTION('',(0.497542812164512,0.497542812164512,-0.710564775461646));
#32111=DIRECTION('',(0.,1.,0.));
#32112=DIRECTION('',(-0.497542812164512,0.497542812164512,0.710564775461646));
#32113=DIRECTION('',(-0.497542812164499,-0.497542812164549,0.710564775461628));
#32114=DIRECTION('',(0.,-1.,0.));
#32115=DIRECTION('',(0.497542812164488,-0.497542812164584,-0.710564775461611));
#32116=DIRECTION('center_axis',(0.24184476264798,0.707106781186533,0.664463024388688));
#32117=DIRECTION('ref_axis',(0.939692620785908,0.,-0.342020143325669));
#32118=DIRECTION('',(-0.63368727422465,0.63368727422465,-0.443712606279635));
#32119=DIRECTION('',(-0.633687274224657,0.633687274224651,-0.443712606279624));
#32120=DIRECTION('',(0.939692620785908,0.,-0.342020143325669));
#32121=DIRECTION('center_axis',(0.707106781186548,0.707106781186548,0.));
#32122=DIRECTION('ref_axis',(0.,0.,-1.));
#32123=DIRECTION('',(0.,0.,-1.));
#32124=DIRECTION('',(0.497542812164536,-0.497542812164536,0.710564775461612));
#32125=DIRECTION('',(0.633687274224612,-0.633687274224612,-0.443712606279744));
#32126=DIRECTION('center_axis',(1.,0.,0.));
#32127=DIRECTION('ref_axis',(0.,1.,0.));
#32128=DIRECTION('',(0.,0.,1.));
#32129=DIRECTION('',(0.,-1.,0.));
#32130=DIRECTION('center_axis',(0.819152044288978,0.,-0.573576436351066));
#32131=DIRECTION('ref_axis',(-0.573576436351066,0.,-0.819152044288978));
#32132=DIRECTION('',(-0.497542812164536,-0.497542812164536,-0.710564775461612));
#32133=DIRECTION('',(-0.497542812164555,0.497542812164478,-0.710564775461639));
#32134=DIRECTION('',(0.,1.,0.));
#32135=DIRECTION('',(0.497542812164566,0.497542812164443,0.710564775461655));
#32136=DIRECTION('center_axis',(0.241844762647962,0.707106781186606,-0.664463024388618));
#32137=DIRECTION('ref_axis',(-0.939692620785905,0.,-0.342020143325678));
#32138=DIRECTION('',(-0.939692620785905,0.,-0.342020143325678));
#32139=DIRECTION('center_axis',(-0.342020143325678,0.,0.939692620785905));
#32140=DIRECTION('ref_axis',(0.939692620785905,0.,0.342020143325678));
#32141=DIRECTION('',(0.939692620785905,0.,0.342020143325678));
#32142=DIRECTION('center_axis',(0.70710678118655,0.707106781186545,0.));
#32143=DIRECTION('ref_axis',(0.,0.,-1.));
#32144=DIRECTION('',(0.,0.,-1.));
#32145=DIRECTION('center_axis',(-0.342020143325669,0.,-0.939692620785908));
#32146=DIRECTION('ref_axis',(-0.939692620785908,0.,0.342020143325669));
#32147=DIRECTION('',(0.,1.,0.));
#32148=DIRECTION('',(-0.939692620785908,0.,0.342020143325669));
#32149=DIRECTION('center_axis',(-1.,0.,0.));
#32150=DIRECTION('ref_axis',(0.,0.,1.));
#32151=DIRECTION('',(0.,1.,0.));
#32152=DIRECTION('',(0.,0.,1.));
#32153=DIRECTION('center_axis',(-0.342020143325669,0.,0.939692620785908));
#32154=DIRECTION('ref_axis',(0.939692620785908,0.,0.342020143325669));
#32155=DIRECTION('',(0.939692620785908,0.,0.342020143325669));
#32156=DIRECTION('center_axis',(0.70710678118655,0.707106781186545,0.));
#32157=DIRECTION('ref_axis',(0.,0.,-1.));
#32158=DIRECTION('',(0.,0.,-1.));
#32159=DIRECTION('center_axis',(-1.,0.,0.));
#32160=DIRECTION('ref_axis',(0.,0.,1.));
#32161=DIRECTION('',(0.,1.,0.));
#32162=DIRECTION('',(0.,0.,1.));
#32163=DIRECTION('center_axis',(-0.342020143325669,0.,0.939692620785908));
#32164=DIRECTION('ref_axis',(0.939692620785908,0.,0.342020143325669));
#32165=DIRECTION('',(0.939692620785908,0.,0.342020143325669));
#32166=DIRECTION('center_axis',(0.70710678118655,0.707106781186545,0.));
#32167=DIRECTION('ref_axis',(0.,0.,-1.));
#32168=DIRECTION('',(0.,0.,-1.));
#32169=DIRECTION('center_axis',(-0.342020143325669,0.,-0.939692620785908));
#32170=DIRECTION('ref_axis',(-0.939692620785908,0.,0.342020143325669));
#32171=DIRECTION('',(0.,1.,0.));
#32172=DIRECTION('',(-0.939692620785908,0.,0.342020143325669));
#32173=DIRECTION('center_axis',(-1.,0.,0.));
#32174=DIRECTION('ref_axis',(0.,0.,1.));
#32175=DIRECTION('',(0.,1.,0.));
#32176=DIRECTION('',(0.,0.,1.));
#32177=DIRECTION('center_axis',(-0.342020143325669,0.,0.939692620785908));
#32178=DIRECTION('ref_axis',(0.939692620785908,0.,0.342020143325669));
#32179=DIRECTION('',(0.939692620785908,0.,0.342020143325669));
#32180=DIRECTION('center_axis',(0.24184476264798,0.707106781186535,-0.664463024388687));
#32181=DIRECTION('ref_axis',(-0.939692620785908,0.,-0.342020143325669));
#32182=DIRECTION('',(-0.633687274224651,0.633687274224655,0.443712606279627));
#32183=DIRECTION('center_axis',(0.70710678118655,0.707106781186545,0.));
#32184=DIRECTION('ref_axis',(0.,0.,-1.));
#32185=DIRECTION('',(0.,0.,-1.));
#32186=DIRECTION('center_axis',(-0.342020143325669,0.,-0.939692620785908));
#32187=DIRECTION('ref_axis',(-0.939692620785908,0.,0.342020143325669));
#32188=DIRECTION('',(0.,1.,0.));
#32189=DIRECTION('',(-0.939692620785908,0.,0.342020143325669));
#32190=DIRECTION('center_axis',(-1.,0.,0.));
#32191=DIRECTION('ref_axis',(0.,0.,1.));
#32192=DIRECTION('',(0.,0.,1.));
#32193=DIRECTION('center_axis',(0.70710678118655,0.707106781186545,0.));
#32194=DIRECTION('ref_axis',(0.,0.,-1.));
#32195=DIRECTION('',(0.,0.,-1.));
#32196=DIRECTION('center_axis',(-1.,0.,0.));
#32197=DIRECTION('ref_axis',(0.,0.,1.));
#32198=DIRECTION('',(0.,1.,0.));
#32199=DIRECTION('',(0.,0.,1.));
#32200=DIRECTION('center_axis',(-0.342020143325669,0.,0.939692620785908));
#32201=DIRECTION('ref_axis',(0.939692620785908,0.,0.342020143325669));
#32202=DIRECTION('',(0.939692620785908,0.,0.342020143325669));
#32203=DIRECTION('center_axis',(0.70710678118655,0.707106781186545,0.));
#32204=DIRECTION('ref_axis',(0.,0.,-1.));
#32205=DIRECTION('',(0.,0.,-1.));
#32206=DIRECTION('center_axis',(-0.342020143325669,0.,-0.939692620785908));
#32207=DIRECTION('ref_axis',(-0.939692620785908,0.,0.342020143325669));
#32208=DIRECTION('',(0.,1.,0.));
#32209=DIRECTION('',(-0.939692620785908,0.,0.342020143325669));
#32210=DIRECTION('center_axis',(-1.,0.,0.));
#32211=DIRECTION('ref_axis',(0.,0.,1.));
#32212=DIRECTION('',(0.,0.,1.));
#32213=DIRECTION('center_axis',(0.70710678118655,0.707106781186545,0.));
#32214=DIRECTION('ref_axis',(0.,0.,-1.));
#32215=DIRECTION('',(0.,0.,-1.));
#32216=DIRECTION('center_axis',(-1.,0.,0.));
#32217=DIRECTION('ref_axis',(0.,0.,1.));
#32218=DIRECTION('',(0.,1.,0.));
#32219=DIRECTION('',(0.,0.,1.));
#32220=DIRECTION('center_axis',(-0.342020143325669,0.,0.939692620785908));
#32221=DIRECTION('ref_axis',(0.939692620785908,0.,0.342020143325669));
#32222=DIRECTION('',(0.939692620785908,0.,0.342020143325669));
#32223=DIRECTION('center_axis',(0.70710678118655,0.707106781186545,0.));
#32224=DIRECTION('ref_axis',(0.,0.,-1.));
#32225=DIRECTION('',(0.,0.,-1.));
#32226=DIRECTION('center_axis',(-0.342020143325669,0.,-0.939692620785908));
#32227=DIRECTION('ref_axis',(-0.939692620785908,0.,0.342020143325669));
#32228=DIRECTION('',(0.,1.,0.));
#32229=DIRECTION('',(-0.939692620785908,0.,0.342020143325669));
#32230=DIRECTION('center_axis',(-1.,0.,0.));
#32231=DIRECTION('ref_axis',(0.,0.,1.));
#32232=DIRECTION('',(0.,1.,0.));
#32233=DIRECTION('',(0.,0.,1.));
#32234=DIRECTION('center_axis',(-0.342020143325669,0.,0.939692620785908));
#32235=DIRECTION('ref_axis',(0.939692620785908,0.,0.342020143325669));
#32236=DIRECTION('',(0.939692620785908,0.,0.342020143325669));
#32237=DIRECTION('center_axis',(0.819152044288976,0.,0.573576436351068));
#32238=DIRECTION('ref_axis',(0.573576436351068,0.,-0.819152044288976));
#32239=DIRECTION('',(0.497542812164537,0.497542812164537,-0.71056477546161));
#32240=DIRECTION('',(0.,1.,0.));
#32241=DIRECTION('',(-0.497542812164537,0.497542812164537,0.71056477546161));
#32242=DIRECTION('',(-0.49754281216453,-0.497542812164559,0.7105647754616));
#32243=DIRECTION('',(0.,-1.,0.));
#32244=DIRECTION('',(0.49754281216453,-0.49754281216456,-0.710564775461599));
#32245=DIRECTION('center_axis',(0.241844762647992,0.7071067811865,0.664463024388719));
#32246=DIRECTION('ref_axis',(0.939692620785908,0.,-0.342020143325669));
#32247=DIRECTION('',(-0.633687274224668,0.633687274224668,-0.443712606279585));
#32248=DIRECTION('',(-0.633687274224648,0.633687274224657,-0.443712606279629));
#32249=DIRECTION('',(0.939692620785908,0.,-0.342020143325669));
#32250=DIRECTION('center_axis',(0.707106781186548,0.707106781186548,0.));
#32251=DIRECTION('ref_axis',(0.,0.,-1.));
#32252=DIRECTION('',(0.,0.,-1.));
#32253=DIRECTION('',(0.497542812164537,-0.497542812164537,0.71056477546161));
#32254=DIRECTION('',(0.633687274224667,-0.633687274224667,-0.443712606279586));
#32255=DIRECTION('center_axis',(1.,0.,0.));
#32256=DIRECTION('ref_axis',(0.,1.,0.));
#32257=DIRECTION('',(0.,0.,1.));
#32258=DIRECTION('',(0.,-1.,0.));
#32259=DIRECTION('center_axis',(0.819152044288976,0.,-0.573576436351068));
#32260=DIRECTION('ref_axis',(-0.573576436351068,0.,-0.819152044288976));
#32261=DIRECTION('',(-0.497542812164537,-0.497542812164537,-0.71056477546161));
#32262=DIRECTION('',(-0.497542812164543,0.497542812164522,-0.710564775461617));
#32263=DIRECTION('',(0.,1.,0.));
#32264=DIRECTION('',(0.497542812164531,0.497542812164558,0.7105647754616));
#32265=DIRECTION('center_axis',(0.241844762647991,0.707106781186501,-0.664463024388718));
#32266=DIRECTION('ref_axis',(-0.939692620785908,0.,-0.342020143325669));
#32267=DIRECTION('',(-0.939692620785908,0.,-0.342020143325669));
#32268=DIRECTION('',(-0.633687274224651,0.633687274224655,0.443712606279627));
#32269=DIRECTION('center_axis',(0.819152044289004,0.,0.573576436351029));
#32270=DIRECTION('ref_axis',(0.573576436351029,0.,-0.819152044289004));
#32271=DIRECTION('',(0.497542812164512,0.497542812164512,-0.710564775461646));
#32272=DIRECTION('',(0.,1.,0.));
#32273=DIRECTION('',(-0.497542812164512,0.497542812164512,0.710564775461646));
#32274=DIRECTION('',(-0.4975428121645,-0.497542812164548,0.710564775461629));
#32275=DIRECTION('',(0.,-1.,0.));
#32276=DIRECTION('',(0.497542812164487,-0.497542812164587,-0.71056477546161));
#32277=DIRECTION('center_axis',(0.24184476264798,0.707106781186534,0.664463024388687));
#32278=DIRECTION('ref_axis',(0.939692620785908,0.,-0.342020143325669));
#32279=DIRECTION('',(-0.633687274224649,0.633687274224649,-0.443712606279638));
#32280=DIRECTION('',(-0.633687274224659,0.633687274224649,-0.443712606279623));
#32281=DIRECTION('',(0.939692620785908,0.,-0.342020143325669));
#32282=DIRECTION('center_axis',(0.707106781186548,0.707106781186548,0.));
#32283=DIRECTION('ref_axis',(0.,0.,-1.));
#32284=DIRECTION('',(0.,0.,-1.));
#32285=DIRECTION('',(0.497542812164486,-0.497542812164486,0.710564775461682));
#32286=DIRECTION('',(0.633687274224649,-0.633687274224649,-0.443712606279638));
#32287=DIRECTION('center_axis',(1.,0.,0.));
#32288=DIRECTION('ref_axis',(0.,1.,0.));
#32289=DIRECTION('',(0.,0.,1.));
#32290=DIRECTION('',(0.,-1.,0.));
#32291=DIRECTION('center_axis',(0.819152044289031,0.,-0.57357643635099));
#32292=DIRECTION('ref_axis',(-0.57357643635099,0.,-0.819152044289031));
#32293=DIRECTION('',(-0.497542812164486,-0.497542812164486,-0.710564775461682));
#32294=DIRECTION('',(-0.497542812164458,0.497542812164571,-0.710564775461641));
#32295=DIRECTION('',(0.,1.,0.));
#32296=DIRECTION('',(0.497542812164457,0.497542812164574,0.71056477546164));
#32297=DIRECTION('center_axis',(0.24184476264798,0.707106781186534,-0.664463024388687));
#32298=DIRECTION('ref_axis',(-0.939692620785908,0.,-0.342020143325669));
#32299=DIRECTION('',(-0.939692620785908,0.,-0.342020143325669));
#32300=DIRECTION('',(-0.633687274224651,0.633687274224655,0.443712606279627));
#32301=DIRECTION('center_axis',(0.819152044289031,0.,0.57357643635099));
#32302=DIRECTION('ref_axis',(0.57357643635099,0.,-0.819152044289031));
#32303=DIRECTION('',(0.497542812164486,0.497542812164486,-0.710564775461682));
#32304=DIRECTION('',(0.,1.,0.));
#32305=DIRECTION('',(-0.497542812164486,0.497542812164486,0.710564775461682));
#32306=DIRECTION('',(-0.497542812164457,-0.497542812164574,0.71056477546164));
#32307=DIRECTION('',(0.,-1.,0.));
#32308=DIRECTION('',(0.497542812164458,-0.497542812164572,-0.710564775461641));
#32309=DIRECTION('center_axis',(0.24184476264798,0.707106781186534,0.664463024388687));
#32310=DIRECTION('ref_axis',(0.939692620785908,0.,-0.342020143325669));
#32311=DIRECTION('',(-0.633687274224649,0.633687274224649,-0.443712606279638));
#32312=DIRECTION('',(-0.633687274224654,0.633687274224652,-0.443712606279625));
#32313=DIRECTION('',(0.939692620785908,0.,-0.342020143325669));
#32314=DIRECTION('center_axis',(0.707106781186548,0.707106781186548,0.));
#32315=DIRECTION('ref_axis',(0.,0.,-1.));
#32316=DIRECTION('',(0.,0.,-1.));
#32317=DIRECTION('',(0.497542812164512,-0.497542812164512,0.710564775461646));
#32318=DIRECTION('',(0.633687274224649,-0.633687274224649,-0.443712606279639));
#32319=DIRECTION('center_axis',(1.,0.,0.));
#32320=DIRECTION('ref_axis',(0.,1.,0.));
#32321=DIRECTION('',(0.,0.,1.));
#32322=DIRECTION('',(0.,-1.,0.));
#32323=DIRECTION('center_axis',(0.819152044289004,0.,-0.573576436351029));
#32324=DIRECTION('ref_axis',(-0.573576436351029,0.,-0.819152044289004));
#32325=DIRECTION('',(-0.497542812164512,-0.497542812164512,-0.710564775461646));
#32326=DIRECTION('',(-0.4975428121645,0.497542812164549,-0.710564775461628));
#32327=DIRECTION('',(0.,1.,0.));
#32328=DIRECTION('',(0.4975428121645,0.497542812164547,0.710564775461629));
#32329=DIRECTION('center_axis',(0.24184476264798,0.707106781186535,-0.664463024388686));
#32330=DIRECTION('ref_axis',(-0.939692620785908,0.,-0.342020143325669));
#32331=DIRECTION('',(-0.939692620785908,0.,-0.342020143325669));
#32332=DIRECTION('',(-0.633687274224651,0.633687274224655,0.443712606279627));
#32333=DIRECTION('center_axis',(0.819152044289004,0.,0.573576436351029));
#32334=DIRECTION('ref_axis',(0.573576436351029,0.,-0.819152044289004));
#32335=DIRECTION('',(0.497542812164512,0.497542812164512,-0.710564775461646));
#32336=DIRECTION('',(0.,1.,0.));
#32337=DIRECTION('',(-0.497542812164512,0.497542812164512,0.710564775461646));
#32338=DIRECTION('',(-0.4975428121645,-0.497542812164546,0.710564775461629));
#32339=DIRECTION('',(0.,-1.,0.));
#32340=DIRECTION('',(0.4975428121645,-0.497542812164548,-0.710564775461629));
#32341=DIRECTION('center_axis',(-0.342020143325669,0.,-0.939692620785908));
#32342=DIRECTION('ref_axis',(-0.939692620785908,0.,0.342020143325669));
#32343=DIRECTION('',(0.939692620785908,0.,-0.342020143325669));
#32344=DIRECTION('',(0.,1.,0.));
#32345=DIRECTION('',(-0.939692620785908,0.,0.342020143325669));
#32346=DIRECTION('center_axis',(0.24184476264798,0.707106781186536,0.664463024388686));
#32347=DIRECTION('ref_axis',(0.939692620785908,0.,-0.342020143325669));
#32348=DIRECTION('',(-0.633687274224648,0.633687274224648,-0.44371260627964));
#32349=DIRECTION('',(-0.633687274224633,0.633687274224639,-0.443712606279676));
#32350=DIRECTION('center_axis',(0.707106781186548,0.707106781186548,0.));
#32351=DIRECTION('ref_axis',(0.,0.,-1.));
#32352=DIRECTION('',(0.,0.,-1.));
#32353=DIRECTION('',(0.497542812164537,-0.497542812164537,0.71056477546161));
#32354=DIRECTION('',(0.633687274224667,-0.633687274224667,-0.443712606279586));
#32355=DIRECTION('center_axis',(0.819152044288976,0.,-0.573576436351068));
#32356=DIRECTION('ref_axis',(-0.573576436351068,0.,-0.819152044288976));
#32357=DIRECTION('',(0.,-1.,0.));
#32358=DIRECTION('',(-0.497542812164537,-0.497542812164537,-0.71056477546161));
#32359=DIRECTION('',(-0.49754281216453,0.49754281216456,-0.710564775461599));
#32360=DIRECTION('',(0.,1.,0.));
#32361=DIRECTION('',(0.497542812164531,0.497542812164558,0.7105647754616));
#32362=DIRECTION('center_axis',(-0.342020143325669,0.,0.939692620785908));
#32363=DIRECTION('ref_axis',(0.939692620785908,0.,0.342020143325669));
#32364=DIRECTION('',(0.939692620785908,0.,0.342020143325669));
#32365=DIRECTION('',(0.,1.,0.));
#32366=DIRECTION('',(-0.939692620785908,0.,-0.342020143325669));
#32367=DIRECTION('center_axis',(0.241844762647992,-0.707106781186499,-0.66446302438872));
#32368=DIRECTION('ref_axis',(-0.939692620785908,0.,-0.342020143325669));
#32369=DIRECTION('',(-0.633687274224668,-0.633687274224668,0.443712606279584));
#32370=DIRECTION('',(-0.939692620785908,0.,-0.342020143325669));
#32371=DIRECTION('',(0.633687274224669,0.633687274224671,-0.443712606279578));
#32372=DIRECTION('center_axis',(0.707106781186548,-0.707106781186548,0.));
#32373=DIRECTION('ref_axis',(0.,0.,-1.));
#32374=DIRECTION('',(0.633687274224649,0.633687274224649,0.443712606279638));
#32375=DIRECTION('',(0.,0.,-1.));
#32376=DIRECTION('',(0.,0.,1.));
#32377=DIRECTION('center_axis',(0.819152044289004,0.,0.573576436351029));
#32378=DIRECTION('ref_axis',(0.573576436351029,0.,-0.819152044289004));
#32379=DIRECTION('',(0.497542812164512,0.497542812164512,-0.710564775461646));
#32380=DIRECTION('',(0.,1.,0.));
#32381=DIRECTION('',(-0.497542812164512,0.497542812164512,0.710564775461646));
#32382=DIRECTION('',(-0.4975428121645,-0.497542812164548,0.710564775461629));
#32383=DIRECTION('',(0.,-1.,0.));
#32384=DIRECTION('',(0.497542812164487,-0.497542812164587,-0.71056477546161));
#32385=DIRECTION('center_axis',(0.24184476264798,0.707106781186534,0.664463024388687));
#32386=DIRECTION('ref_axis',(0.939692620785908,0.,-0.342020143325669));
#32387=DIRECTION('',(-0.633687274224649,0.633687274224649,-0.443712606279638));
#32388=DIRECTION('',(-0.633687274224657,0.633687274224651,-0.443712606279624));
#32389=DIRECTION('',(0.939692620785908,0.,-0.342020143325669));
#32390=DIRECTION('center_axis',(0.707106781186548,0.707106781186548,0.));
#32391=DIRECTION('ref_axis',(0.,0.,-1.));
#32392=DIRECTION('',(0.,0.,-1.));
#32393=DIRECTION('',(0.497542812164486,-0.497542812164486,0.710564775461682));
#32394=DIRECTION('',(0.633687274224649,-0.633687274224649,-0.443712606279638));
#32395=DIRECTION('center_axis',(1.,0.,0.));
#32396=DIRECTION('ref_axis',(0.,1.,0.));
#32397=DIRECTION('',(0.,0.,1.));
#32398=DIRECTION('',(0.,-1.,0.));
#32399=DIRECTION('center_axis',(0.819152044289031,0.,-0.57357643635099));
#32400=DIRECTION('ref_axis',(-0.57357643635099,0.,-0.819152044289031));
#32401=DIRECTION('',(-0.497542812164486,-0.497542812164486,-0.710564775461682));
#32402=DIRECTION('',(-0.497542812164458,0.497542812164571,-0.710564775461641));
#32403=DIRECTION('',(0.,1.,0.));
#32404=DIRECTION('',(0.497542812164457,0.497542812164574,0.71056477546164));
#32405=DIRECTION('center_axis',(0.24184476264798,0.707106781186534,-0.664463024388687));
#32406=DIRECTION('ref_axis',(-0.939692620785908,0.,-0.342020143325669));
#32407=DIRECTION('',(-0.939692620785908,0.,-0.342020143325669));
#32408=DIRECTION('',(-0.633687274224651,0.633687274224655,0.443712606279627));
#32409=DIRECTION('center_axis',(0.819152044289004,0.,0.573576436351029));
#32410=DIRECTION('ref_axis',(0.573576436351029,0.,-0.819152044289004));
#32411=DIRECTION('',(0.497542812164512,0.497542812164512,-0.710564775461646));
#32412=DIRECTION('',(0.,1.,0.));
#32413=DIRECTION('',(-0.497542812164512,0.497542812164512,0.710564775461646));
#32414=DIRECTION('',(-0.4975428121645,-0.497542812164548,0.710564775461629));
#32415=DIRECTION('',(0.,-1.,0.));
#32416=DIRECTION('',(0.4975428121645,-0.497542812164546,-0.710564775461629));
#32417=DIRECTION('center_axis',(0.24184476264798,0.707106781186534,0.664463024388687));
#32418=DIRECTION('ref_axis',(0.939692620785908,0.,-0.342020143325669));
#32419=DIRECTION('',(-0.633687274224649,0.633687274224649,-0.443712606279638));
#32420=DIRECTION('',(-0.633687274224654,0.633687274224652,-0.443712606279625));
#32421=DIRECTION('',(0.939692620785908,0.,-0.342020143325669));
#32422=DIRECTION('center_axis',(0.707106781186548,0.707106781186548,0.));
#32423=DIRECTION('ref_axis',(0.,0.,-1.));
#32424=DIRECTION('',(0.,0.,-1.));
#32425=DIRECTION('',(0.497542812164512,-0.497542812164512,0.710564775461646));
#32426=DIRECTION('',(0.633687274224649,-0.633687274224649,-0.443712606279639));
#32427=DIRECTION('center_axis',(1.,0.,0.));
#32428=DIRECTION('ref_axis',(0.,1.,0.));
#32429=DIRECTION('',(0.,0.,1.));
#32430=DIRECTION('',(0.,-1.,0.));
#32431=DIRECTION('center_axis',(0.819152044289004,0.,-0.573576436351029));
#32432=DIRECTION('ref_axis',(-0.573576436351029,0.,-0.819152044289004));
#32433=DIRECTION('',(-0.497542812164512,-0.497542812164512,-0.710564775461646));
#32434=DIRECTION('',(-0.497542812164487,0.497542812164587,-0.71056477546161));
#32435=DIRECTION('',(0.,1.,0.));
#32436=DIRECTION('',(0.4975428121645,0.497542812164547,0.710564775461629));
#32437=DIRECTION('center_axis',(0.24184476264798,0.707106781186536,-0.664463024388686));
#32438=DIRECTION('ref_axis',(-0.939692620785908,0.,-0.342020143325669));
#32439=DIRECTION('',(-0.939692620785908,0.,-0.342020143325669));
#32440=DIRECTION('',(-0.633687274224651,0.633687274224655,0.443712606279627));
#32441=DIRECTION('center_axis',(0.819152044289004,0.,0.573576436351029));
#32442=DIRECTION('ref_axis',(0.573576436351029,0.,-0.819152044289004));
#32443=DIRECTION('',(0.497542812164512,0.497542812164512,-0.710564775461646));
#32444=DIRECTION('',(-0.4975428121645,-0.497542812164546,0.710564775461629));
#32445=DIRECTION('',(0.,-1.,0.));
#32446=DIRECTION('',(0.4975428121645,-0.497542812164548,-0.710564775461629));
#32447=DIRECTION('center_axis',(0.24184476264798,-0.707106781186534,0.664463024388687));
#32448=DIRECTION('ref_axis',(0.939692620785908,0.,-0.342020143325669));
#32449=DIRECTION('',(-0.939692620785908,0.,0.342020143325669));
#32450=DIRECTION('',(0.633687274224654,0.633687274224652,0.443712606279625));
#32451=DIRECTION('',(0.939692620785908,0.,-0.342020143325669));
#32452=DIRECTION('',(0.633687274224649,0.633687274224649,0.443712606279638));
#32453=DIRECTION('center_axis',(-0.342020143325669,0.,-0.939692620785908));
#32454=DIRECTION('ref_axis',(-0.939692620785908,0.,0.342020143325669));
#32455=DIRECTION('',(0.939692620785908,0.,-0.342020143325669));
#32456=DIRECTION('',(0.,1.,0.));
#32457=DIRECTION('center_axis',(0.24184476264798,0.707106781186536,0.664463024388686));
#32458=DIRECTION('ref_axis',(0.939692620785908,0.,-0.342020143325669));
#32459=DIRECTION('',(-0.633687274224633,0.633687274224639,-0.443712606279676));
#32460=DIRECTION('center_axis',(0.70710678118655,0.707106781186545,0.));
#32461=DIRECTION('ref_axis',(0.,0.,-1.));
#32462=DIRECTION('',(0.,0.,-1.));
#32463=DIRECTION('center_axis',(-1.,0.,0.));
#32464=DIRECTION('ref_axis',(0.,0.,1.));
#32465=DIRECTION('',(0.,1.,0.));
#32466=DIRECTION('',(0.,0.,1.));
#32467=DIRECTION('center_axis',(-0.342020143325669,0.,0.939692620785908));
#32468=DIRECTION('ref_axis',(0.939692620785908,0.,0.342020143325669));
#32469=DIRECTION('',(0.939692620785908,0.,0.342020143325669));
#32470=DIRECTION('center_axis',(0.70710678118655,0.707106781186545,0.));
#32471=DIRECTION('ref_axis',(0.,0.,-1.));
#32472=DIRECTION('',(0.,0.,-1.));
#32473=DIRECTION('center_axis',(-0.342020143325669,0.,-0.939692620785908));
#32474=DIRECTION('ref_axis',(-0.939692620785908,0.,0.342020143325669));
#32475=DIRECTION('',(0.,1.,0.));
#32476=DIRECTION('',(-0.939692620785908,0.,0.342020143325669));
#32477=DIRECTION('center_axis',(-1.,0.,0.));
#32478=DIRECTION('ref_axis',(0.,0.,1.));
#32479=DIRECTION('',(0.,1.,0.));
#32480=DIRECTION('',(0.,0.,1.));
#32481=DIRECTION('center_axis',(-0.342020143325669,0.,0.939692620785908));
#32482=DIRECTION('ref_axis',(0.939692620785908,0.,0.342020143325669));
#32483=DIRECTION('',(0.939692620785908,0.,0.342020143325669));
#32484=DIRECTION('center_axis',(0.241844762647991,0.707106781186501,-0.664463024388718));
#32485=DIRECTION('ref_axis',(-0.939692620785908,0.,-0.342020143325669));
#32486=DIRECTION('',(-0.633687274224651,0.633687274224655,0.443712606279627));
#32487=DIRECTION('center_axis',(0.70710678118655,0.707106781186545,0.));
#32488=DIRECTION('ref_axis',(0.,0.,-1.));
#32489=DIRECTION('',(0.,0.,-1.));
#32490=DIRECTION('center_axis',(-0.342020143325669,0.,-0.939692620785908));
#32491=DIRECTION('ref_axis',(-0.939692620785908,0.,0.342020143325669));
#32492=DIRECTION('',(0.,1.,0.));
#32493=DIRECTION('',(-0.939692620785908,0.,0.342020143325669));
#32494=DIRECTION('center_axis',(-1.,0.,0.));
#32495=DIRECTION('ref_axis',(0.,0.,1.));
#32496=DIRECTION('',(0.,0.,1.));
#32497=DIRECTION('center_axis',(0.70710678118655,0.707106781186545,0.));
#32498=DIRECTION('ref_axis',(0.,0.,-1.));
#32499=DIRECTION('',(0.,0.,-1.));
#32500=DIRECTION('center_axis',(-1.,0.,0.));
#32501=DIRECTION('ref_axis',(0.,0.,1.));
#32502=DIRECTION('',(0.,1.,0.));
#32503=DIRECTION('',(0.,0.,1.));
#32504=DIRECTION('center_axis',(-0.342020143325669,0.,0.939692620785908));
#32505=DIRECTION('ref_axis',(0.939692620785908,0.,0.342020143325669));
#32506=DIRECTION('',(0.939692620785908,0.,0.342020143325669));
#32507=DIRECTION('center_axis',(0.70710678118655,0.707106781186545,0.));
#32508=DIRECTION('ref_axis',(0.,0.,-1.));
#32509=DIRECTION('',(0.,0.,-1.));
#32510=DIRECTION('center_axis',(-0.342020143325669,0.,-0.939692620785908));
#32511=DIRECTION('ref_axis',(-0.939692620785908,0.,0.342020143325669));
#32512=DIRECTION('',(0.,1.,0.));
#32513=DIRECTION('',(-0.939692620785908,0.,0.342020143325669));
#32514=DIRECTION('center_axis',(-1.,0.,0.));
#32515=DIRECTION('ref_axis',(0.,0.,1.));
#32516=DIRECTION('',(0.,1.,0.));
#32517=DIRECTION('',(0.,0.,1.));
#32518=DIRECTION('center_axis',(-0.342020143325669,0.,0.939692620785908));
#32519=DIRECTION('ref_axis',(0.939692620785908,0.,0.342020143325669));
#32520=DIRECTION('',(0.939692620785908,0.,0.342020143325669));
#32521=DIRECTION('center_axis',(0.70710678118655,0.707106781186545,0.));
#32522=DIRECTION('ref_axis',(0.,0.,-1.));
#32523=DIRECTION('',(0.,0.,-1.));
#32524=DIRECTION('center_axis',(-0.342020143325669,0.,-0.939692620785908));
#32525=DIRECTION('ref_axis',(-0.939692620785908,0.,0.342020143325669));
#32526=DIRECTION('',(0.,1.,0.));
#32527=DIRECTION('',(-0.939692620785908,0.,0.342020143325669));
#32528=DIRECTION('center_axis',(-1.,0.,0.));
#32529=DIRECTION('ref_axis',(0.,0.,1.));
#32530=DIRECTION('',(0.,1.,0.));
#32531=DIRECTION('',(0.,0.,1.));
#32532=DIRECTION('center_axis',(-0.342020143325669,0.,0.939692620785908));
#32533=DIRECTION('ref_axis',(0.939692620785908,0.,0.342020143325669));
#32534=DIRECTION('',(0.939692620785908,0.,0.342020143325669));
#32535=DIRECTION('center_axis',(0.70710678118655,0.707106781186545,0.));
#32536=DIRECTION('ref_axis',(0.,0.,-1.));
#32537=DIRECTION('',(0.,0.,-1.));
#32538=DIRECTION('center_axis',(-0.342020143325669,0.,-0.939692620785908));
#32539=DIRECTION('ref_axis',(-0.939692620785908,0.,0.342020143325669));
#32540=DIRECTION('',(0.,1.,0.));
#32541=DIRECTION('',(-0.939692620785908,0.,0.342020143325669));
#32542=DIRECTION('center_axis',(-1.,0.,0.));
#32543=DIRECTION('ref_axis',(0.,0.,1.));
#32544=DIRECTION('',(0.,0.,1.));
#32545=DIRECTION('center_axis',(0.70710678118655,0.707106781186545,0.));
#32546=DIRECTION('ref_axis',(0.,0.,-1.));
#32547=DIRECTION('',(0.,0.,-1.));
#32548=DIRECTION('center_axis',(-1.,0.,0.));
#32549=DIRECTION('ref_axis',(0.,0.,1.));
#32550=DIRECTION('',(0.,1.,0.));
#32551=DIRECTION('',(0.,0.,1.));
#32552=DIRECTION('center_axis',(-0.342020143325669,0.,0.939692620785908));
#32553=DIRECTION('ref_axis',(0.939692620785908,0.,0.342020143325669));
#32554=DIRECTION('',(0.939692620785908,0.,0.342020143325669));
#32555=DIRECTION('center_axis',(0.70710678118655,0.707106781186545,0.));
#32556=DIRECTION('ref_axis',(0.,0.,-1.));
#32557=DIRECTION('',(0.,0.,-1.));
#32558=DIRECTION('center_axis',(-0.342020143325669,0.,-0.939692620785908));
#32559=DIRECTION('ref_axis',(-0.939692620785908,0.,0.342020143325669));
#32560=DIRECTION('',(0.,1.,0.));
#32561=DIRECTION('',(-0.939692620785908,0.,0.342020143325669));
#32562=DIRECTION('center_axis',(-1.,0.,0.));
#32563=DIRECTION('ref_axis',(0.,0.,1.));
#32564=DIRECTION('',(0.,1.,0.));
#32565=DIRECTION('',(0.,0.,1.));
#32566=DIRECTION('center_axis',(-0.342020143325669,0.,0.939692620785908));
#32567=DIRECTION('ref_axis',(0.939692620785908,0.,0.342020143325669));
#32568=DIRECTION('',(0.939692620785908,0.,0.342020143325669));
#32569=DIRECTION('center_axis',(0.819152044289004,0.,0.573576436351029));
#32570=DIRECTION('ref_axis',(0.573576436351029,0.,-0.819152044289004));
#32571=DIRECTION('',(0.497542812164512,0.497542812164512,-0.710564775461646));
#32572=DIRECTION('',(0.,1.,0.));
#32573=DIRECTION('',(-0.497542812164512,0.497542812164512,0.710564775461646));
#32574=DIRECTION('',(-0.497542812164502,-0.497542812164542,0.710564775461631));
#32575=DIRECTION('',(0.,-1.,0.));
#32576=DIRECTION('',(0.497542812164502,-0.497542812164542,-0.710564775461631));
#32577=DIRECTION('center_axis',(0.241844762647986,0.707106781186536,0.664463024388684));
#32578=DIRECTION('ref_axis',(0.939692620785905,0.,-0.342020143325678));
#32579=DIRECTION('',(-0.63368727422465,0.63368727422465,-0.443712606279636));
#32580=DIRECTION('',(-0.633687274224657,0.633687274224651,-0.443712606279624));
#32581=DIRECTION('',(0.939692620785905,0.,-0.342020143325678));
#32582=DIRECTION('center_axis',(0.707106781186548,0.707106781186548,0.));
#32583=DIRECTION('ref_axis',(0.,0.,-1.));
#32584=DIRECTION('',(0.,0.,-1.));
#32585=DIRECTION('',(0.497542812164483,-0.497542812164483,0.710564775461686));
#32586=DIRECTION('',(0.63368727422463,-0.63368727422463,-0.443712606279693));
#32587=DIRECTION('center_axis',(1.,0.,0.));
#32588=DIRECTION('ref_axis',(0.,1.,0.));
#32589=DIRECTION('',(0.,0.,1.));
#32590=DIRECTION('',(0.,-1.,0.));
#32591=DIRECTION('center_axis',(0.819152044289035,0.,-0.573576436350985));
#32592=DIRECTION('ref_axis',(-0.573576436350985,0.,-0.819152044289035));
#32593=DIRECTION('',(-0.497542812164483,-0.497542812164483,-0.710564775461686));
#32594=DIRECTION('',(-0.497542812164467,0.497542812164533,-0.710564775461663));
#32595=DIRECTION('',(0.,1.,0.));
#32596=DIRECTION('',(0.497542812164467,0.497542812164531,0.710564775461663));
#32597=DIRECTION('center_axis',(0.241844762647973,0.707106781186573,-0.664463024388649));
#32598=DIRECTION('ref_axis',(-0.939692620785905,0.,-0.342020143325678));
#32599=DIRECTION('',(-0.939692620785905,0.,-0.342020143325678));
#32600=DIRECTION('',(-0.633687274224617,0.633687274224621,0.443712606279724));
#32601=DIRECTION('center_axis',(0.819152044289007,0.,0.573576436351024));
#32602=DIRECTION('ref_axis',(0.573576436351024,0.,-0.819152044289007));
#32603=DIRECTION('',(0.497542812164509,0.497542812164509,-0.71056477546165));
#32604=DIRECTION('',(0.,1.,0.));
#32605=DIRECTION('',(-0.497542812164509,0.497542812164509,0.71056477546165));
#32606=DIRECTION('',(-0.497542812164497,-0.497542812164545,0.710564775461633));
#32607=DIRECTION('',(0.,-1.,0.));
#32608=DIRECTION('',(0.497542812164509,-0.497542812164509,-0.71056477546165));
#32609=DIRECTION('center_axis',(0.241844762647986,0.707106781186536,0.664463024388684));
#32610=DIRECTION('ref_axis',(0.939692620785905,0.,-0.342020143325678));
#32611=DIRECTION('',(-0.63368727422465,0.63368727422465,-0.443712606279636));
#32612=DIRECTION('',(-0.633687274224657,0.633687274224651,-0.443712606279624));
#32613=DIRECTION('',(0.939692620785905,0.,-0.342020143325678));
#32614=DIRECTION('center_axis',(0.707106781186548,0.707106781186548,0.));
#32615=DIRECTION('ref_axis',(0.,0.,-1.));
#32616=DIRECTION('',(0.,0.,-1.));
#32617=DIRECTION('',(0.497542812164536,-0.497542812164536,0.710564775461612));
#32618=DIRECTION('',(0.63368727422465,-0.63368727422465,-0.443712606279635));
#32619=DIRECTION('center_axis',(1.,0.,0.));
#32620=DIRECTION('ref_axis',(0.,1.,0.));
#32621=DIRECTION('',(0.,0.,1.));
#32622=DIRECTION('',(0.,-1.,0.));
#32623=DIRECTION('center_axis',(0.819152044288978,0.,-0.573576436351066));
#32624=DIRECTION('ref_axis',(-0.573576436351066,0.,-0.819152044288978));
#32625=DIRECTION('',(-0.497542812164536,-0.497542812164536,-0.710564775461612));
#32626=DIRECTION('',(-0.497542812164528,0.49754281216456,-0.7105647754616));
#32627=DIRECTION('',(0.,1.,0.));
#32628=DIRECTION('',(0.497542812164539,0.497542812164525,0.710564775461617));
#32629=DIRECTION('center_axis',(0.24184476264798,0.707106781186533,-0.664463024388688));
#32630=DIRECTION('ref_axis',(-0.939692620785908,0.,-0.342020143325669));
#32631=DIRECTION('',(-0.939692620785908,0.,-0.342020143325669));
#32632=DIRECTION('',(-0.633687274224651,0.633687274224655,0.443712606279627));
#32633=DIRECTION('center_axis',(0.81915204428898,0.,0.573576436351063));
#32634=DIRECTION('ref_axis',(0.573576436351063,0.,-0.81915204428898));
#32635=DIRECTION('',(0.497542812164534,0.497542812164534,-0.710564775461614));
#32636=DIRECTION('',(0.,1.,0.));
#32637=DIRECTION('',(-0.497542812164534,0.497542812164534,0.710564775461614));
#32638=DIRECTION('',(-0.497542812164527,-0.497542812164557,0.710564775461603));
#32639=DIRECTION('',(0.,-1.,0.));
#32640=DIRECTION('',(0.497542812164539,-0.497542812164519,-0.710564775461621));
#32641=DIRECTION('center_axis',(0.241844762647998,0.7071067811865,0.664463024388717));
#32642=DIRECTION('ref_axis',(0.939692620785905,0.,-0.342020143325678));
#32643=DIRECTION('',(-0.633687274224669,0.633687274224669,-0.443712606279581));
#32644=DIRECTION('',(-0.633687274224674,0.633687274224668,-0.443712606279576));
#32645=DIRECTION('',(0.939692620785905,0.,-0.342020143325678));
#32646=DIRECTION('center_axis',(0.707106781186548,0.707106781186548,0.));
#32647=DIRECTION('ref_axis',(0.,0.,-1.));
#32648=DIRECTION('',(0.,0.,-1.));
#32649=DIRECTION('',(0.497542812164512,-0.497542812164512,0.710564775461646));
#32650=DIRECTION('',(0.633687274224649,-0.633687274224649,-0.443712606279638));
#32651=DIRECTION('center_axis',(1.,0.,0.));
#32652=DIRECTION('ref_axis',(0.,1.,0.));
#32653=DIRECTION('',(0.,0.,1.));
#32654=DIRECTION('',(0.,-1.,0.));
#32655=DIRECTION('center_axis',(0.819152044289004,0.,-0.573576436351029));
#32656=DIRECTION('ref_axis',(-0.573576436351029,0.,-0.819152044289004));
#32657=DIRECTION('',(-0.497542812164512,-0.497542812164512,-0.710564775461646));
#32658=DIRECTION('',(-0.497542812164502,0.497542812164542,-0.710564775461631));
#32659=DIRECTION('',(0.,1.,0.));
#32660=DIRECTION('',(0.497542812164502,0.497542812164541,0.710564775461632));
#32661=DIRECTION('center_axis',(0.241844762647985,0.707106781186537,-0.664463024388683));
#32662=DIRECTION('ref_axis',(-0.939692620785905,0.,-0.342020143325678));
#32663=DIRECTION('',(-0.939692620785905,0.,-0.342020143325678));
#32664=DIRECTION('',(-0.633687274224651,0.633687274224655,0.443712606279627));
#32665=DIRECTION('center_axis',(0.819152044289007,0.,0.573576436351024));
#32666=DIRECTION('ref_axis',(0.573576436351024,0.,-0.819152044289007));
#32667=DIRECTION('',(0.497542812164509,0.497542812164509,-0.71056477546165));
#32668=DIRECTION('',(0.,1.,0.));
#32669=DIRECTION('',(-0.497542812164509,0.497542812164509,0.71056477546165));
#32670=DIRECTION('',(-0.497542812164497,-0.497542812164545,0.710564775461633));
#32671=DIRECTION('',(0.,-1.,0.));
#32672=DIRECTION('',(0.497542812164497,-0.497542812164545,-0.710564775461633));
#32673=DIRECTION('center_axis',(0.241844762647986,0.707106781186536,0.664463024388684));
#32674=DIRECTION('ref_axis',(0.939692620785905,0.,-0.342020143325678));
#32675=DIRECTION('',(-0.63368727422465,0.63368727422465,-0.443712606279636));
#32676=DIRECTION('',(-0.633687274224652,0.633687274224654,-0.443712606279627));
#32677=DIRECTION('',(0.939692620785905,0.,-0.342020143325678));
#32678=DIRECTION('center_axis',(0.707106781186548,0.707106781186548,0.));
#32679=DIRECTION('ref_axis',(0.,0.,-1.));
#32680=DIRECTION('',(0.,0.,-1.));
#32681=DIRECTION('',(0.497542812164483,-0.497542812164483,0.710564775461686));
#32682=DIRECTION('',(0.63368727422463,-0.63368727422463,-0.443712606279692));
#32683=DIRECTION('center_axis',(1.,0.,0.));
#32684=DIRECTION('ref_axis',(0.,1.,0.));
#32685=DIRECTION('',(0.,0.,1.));
#32686=DIRECTION('',(0.,-1.,0.));
#32687=DIRECTION('center_axis',(0.819152044289035,0.,-0.573576436350985));
#32688=DIRECTION('ref_axis',(-0.573576436350985,0.,-0.819152044289035));
#32689=DIRECTION('',(-0.497542812164483,-0.497542812164483,-0.710564775461686));
#32690=DIRECTION('',(-0.497542812164467,0.497542812164533,-0.710564775461663));
#32691=DIRECTION('',(0.,1.,0.));
#32692=DIRECTION('',(0.497542812164467,0.497542812164532,0.710564775461663));
#32693=DIRECTION('center_axis',(0.241844762647973,0.707106781186572,-0.664463024388649));
#32694=DIRECTION('ref_axis',(-0.939692620785905,0.,-0.342020143325678));
#32695=DIRECTION('',(-0.939692620785905,0.,-0.342020143325678));
#32696=DIRECTION('',(-0.633687274224617,0.633687274224621,0.443712606279724));
#32697=DIRECTION('center_axis',(0.819152044289007,0.,0.573576436351024));
#32698=DIRECTION('ref_axis',(0.573576436351024,0.,-0.819152044289007));
#32699=DIRECTION('',(0.497542812164509,0.497542812164509,-0.71056477546165));
#32700=DIRECTION('',(0.,1.,0.));
#32701=DIRECTION('',(-0.497542812164509,0.497542812164509,0.71056477546165));
#32702=DIRECTION('',(-0.497542812164497,-0.497542812164543,0.710564775461634));
#32703=DIRECTION('',(0.,-1.,0.));
#32704=DIRECTION('',(0.497542812164497,-0.497542812164545,-0.710564775461633));
#32705=DIRECTION('center_axis',(0.241844762647985,0.707106781186537,0.664463024388682));
#32706=DIRECTION('ref_axis',(0.939692620785905,0.,-0.342020143325678));
#32707=DIRECTION('',(-0.633687274224649,0.633687274224649,-0.443712606279638));
#32708=DIRECTION('',(-0.633687274224657,0.633687274224651,-0.443712606279624));
#32709=DIRECTION('',(0.939692620785905,0.,-0.342020143325678));
#32710=DIRECTION('center_axis',(0.707106781186548,0.707106781186548,0.));
#32711=DIRECTION('ref_axis',(0.,0.,-1.));
#32712=DIRECTION('',(0.,0.,-1.));
#32713=DIRECTION('',(0.497542812164512,-0.497542812164512,0.710564775461646));
#32714=DIRECTION('',(0.633687274224649,-0.633687274224649,-0.443712606279637));
#32715=DIRECTION('center_axis',(1.,0.,0.));
#32716=DIRECTION('ref_axis',(0.,1.,0.));
#32717=DIRECTION('',(0.,0.,1.));
#32718=DIRECTION('',(0.,-1.,0.));
#32719=DIRECTION('center_axis',(0.819152044289004,0.,-0.573576436351029));
#32720=DIRECTION('ref_axis',(-0.573576436351029,0.,-0.819152044289004));
#32721=DIRECTION('',(-0.497542812164512,-0.497542812164512,-0.710564775461646));
#32722=DIRECTION('',(-0.497542812164502,0.497542812164542,-0.710564775461631));
#32723=DIRECTION('',(0.,1.,0.));
#32724=DIRECTION('',(0.497542812164502,0.497542812164541,0.710564775461632));
#32725=DIRECTION('center_axis',(0.241844762647985,0.707106781186537,-0.664463024388683));
#32726=DIRECTION('ref_axis',(-0.939692620785905,0.,-0.342020143325678));
#32727=DIRECTION('',(-0.939692620785905,0.,-0.342020143325678));
#32728=DIRECTION('',(-0.633687274224651,0.633687274224655,0.443712606279627));
#32729=DIRECTION('center_axis',(0.819152044289002,0.,0.573576436351031));
#32730=DIRECTION('ref_axis',(0.573576436351031,0.,-0.819152044289002));
#32731=DIRECTION('',(0.497542812164513,0.497542812164513,-0.710564775461643));
#32732=DIRECTION('',(0.,1.,0.));
#32733=DIRECTION('',(-0.497542812164513,0.497542812164513,0.710564775461643));
#32734=DIRECTION('',(-0.497542812164502,-0.497542812164546,0.710564775461628));
#32735=DIRECTION('',(0.,-1.,0.));
#32736=DIRECTION('',(0.497542812164503,-0.497542812164544,-0.710564775461629));
#32737=DIRECTION('center_axis',(0.24184476264798,0.707106781186534,0.664463024388687));
#32738=DIRECTION('ref_axis',(0.939692620785908,0.,-0.342020143325669));
#32739=DIRECTION('',(-0.633687274224649,0.633687274224649,-0.443712606279638));
#32740=DIRECTION('',(-0.633687274224652,0.633687274224654,-0.443712606279627));
#32741=DIRECTION('',(0.939692620785908,0.,-0.342020143325669));
#32742=DIRECTION('center_axis',(0.707106781186548,0.707106781186548,0.));
#32743=DIRECTION('ref_axis',(0.,0.,-1.));
#32744=DIRECTION('',(0.,0.,-1.));
#32745=DIRECTION('',(0.497542812164513,-0.497542812164513,0.710564775461643));
#32746=DIRECTION('',(0.633687274224649,-0.633687274224649,-0.443712606279638));
#32747=DIRECTION('center_axis',(1.,0.,0.));
#32748=DIRECTION('ref_axis',(0.,1.,0.));
#32749=DIRECTION('',(0.,0.,1.));
#32750=DIRECTION('',(0.,-1.,0.));
#32751=DIRECTION('center_axis',(0.819152044289002,0.,-0.573576436351031));
#32752=DIRECTION('ref_axis',(-0.573576436351031,0.,-0.819152044289002));
#32753=DIRECTION('',(-0.497542812164513,-0.497542812164513,-0.710564775461643));
#32754=DIRECTION('',(-0.497542812164502,0.497542812164548,-0.710564775461627));
#32755=DIRECTION('',(0.,1.,0.));
#32756=DIRECTION('',(0.497542812164503,0.497542812164546,0.710564775461628));
#32757=DIRECTION('center_axis',(0.24184476264798,0.707106781186535,-0.664463024388686));
#32758=DIRECTION('ref_axis',(-0.939692620785908,0.,-0.342020143325669));
#32759=DIRECTION('',(-0.939692620785908,0.,-0.342020143325669));
#32760=DIRECTION('',(-0.633687274224651,0.633687274224655,0.443712606279627));
#32761=DIRECTION('center_axis',(0.819152044288976,0.,0.573576436351068));
#32762=DIRECTION('ref_axis',(0.573576436351068,0.,-0.819152044288976));
#32763=DIRECTION('',(0.497542812164537,0.497542812164537,-0.71056477546161));
#32764=DIRECTION('',(-0.497542812164518,-0.497542812164595,0.710564775461582));
#32765=DIRECTION('',(0.,-1.,0.));
#32766=DIRECTION('',(0.49754281216453,-0.49754281216456,-0.710564775461599));
#32767=DIRECTION('center_axis',(0.241844762647992,-0.707106781186499,0.66446302438872));
#32768=DIRECTION('ref_axis',(0.939692620785908,0.,-0.342020143325669));
#32769=DIRECTION('',(-0.939692620785908,0.,0.342020143325669));
#32770=DIRECTION('',(0.633687274224669,0.633687274224671,0.443712606279578));
#32771=DIRECTION('',(0.939692620785908,0.,-0.342020143325669));
#32772=DIRECTION('',(0.633687274224668,0.633687274224668,0.443712606279584));
#32773=DIRECTION('center_axis',(-0.342020143325669,0.,-0.939692620785908));
#32774=DIRECTION('ref_axis',(-0.939692620785908,0.,0.342020143325669));
#32775=DIRECTION('',(0.939692620785908,0.,-0.342020143325669));
#32776=DIRECTION('',(0.,1.,0.));
#32777=DIRECTION('center_axis',(0.241844762648004,0.707106781186466,0.664463024388752));
#32778=DIRECTION('ref_axis',(0.939692620785908,0.,-0.342020143325669));
#32779=DIRECTION('',(-0.633687274224695,0.633687274224682,-0.443712606279526));
#32780=DIRECTION('center_axis',(0.70710678118655,0.707106781186545,0.));
#32781=DIRECTION('ref_axis',(0.,0.,-1.));
#32782=DIRECTION('',(0.,0.,-1.));
#32783=DIRECTION('center_axis',(-1.,0.,0.));
#32784=DIRECTION('ref_axis',(0.,0.,1.));
#32785=DIRECTION('',(0.,1.,0.));
#32786=DIRECTION('',(0.,0.,1.));
#32787=DIRECTION('center_axis',(-0.342020143325669,0.,0.939692620785908));
#32788=DIRECTION('ref_axis',(0.939692620785908,0.,0.342020143325669));
#32789=DIRECTION('',(0.939692620785908,0.,0.342020143325669));
#32790=DIRECTION('center_axis',(0.70710678118655,0.707106781186545,0.));
#32791=DIRECTION('ref_axis',(0.,0.,-1.));
#32792=DIRECTION('',(0.,0.,-1.));
#32793=DIRECTION('center_axis',(-0.342020143325669,0.,-0.939692620785908));
#32794=DIRECTION('ref_axis',(-0.939692620785908,0.,0.342020143325669));
#32795=DIRECTION('',(0.,1.,0.));
#32796=DIRECTION('',(-0.939692620785908,0.,0.342020143325669));
#32797=DIRECTION('center_axis',(-1.,0.,0.));
#32798=DIRECTION('ref_axis',(0.,0.,1.));
#32799=DIRECTION('',(0.,1.,0.));
#32800=DIRECTION('',(0.,0.,1.));
#32801=DIRECTION('center_axis',(-0.342020143325678,0.,0.939692620785905));
#32802=DIRECTION('ref_axis',(0.939692620785905,0.,0.342020143325678));
#32803=DIRECTION('',(0.939692620785905,0.,0.342020143325678));
#32804=DIRECTION('center_axis',(0.70710678118655,0.707106781186545,0.));
#32805=DIRECTION('ref_axis',(0.,0.,-1.));
#32806=DIRECTION('',(0.,0.,-1.));
#32807=DIRECTION('center_axis',(-0.342020143325678,0.,-0.939692620785905));
#32808=DIRECTION('ref_axis',(-0.939692620785905,0.,0.342020143325678));
#32809=DIRECTION('',(0.,1.,0.));
#32810=DIRECTION('',(-0.939692620785905,0.,0.342020143325678));
#32811=DIRECTION('center_axis',(-1.,0.,0.));
#32812=DIRECTION('ref_axis',(0.,0.,1.));
#32813=DIRECTION('',(0.,1.,0.));
#32814=DIRECTION('',(0.,0.,1.));
#32815=DIRECTION('center_axis',(-0.342020143325678,0.,0.939692620785905));
#32816=DIRECTION('ref_axis',(0.939692620785905,0.,0.342020143325678));
#32817=DIRECTION('',(0.939692620785905,0.,0.342020143325678));
#32818=DIRECTION('center_axis',(0.70710678118655,0.707106781186545,0.));
#32819=DIRECTION('ref_axis',(0.,0.,-1.));
#32820=DIRECTION('',(0.,0.,-1.));
#32821=DIRECTION('center_axis',(-0.342020143325678,0.,-0.939692620785905));
#32822=DIRECTION('ref_axis',(-0.939692620785905,0.,0.342020143325678));
#32823=DIRECTION('',(0.,1.,0.));
#32824=DIRECTION('',(-0.939692620785905,0.,0.342020143325678));
#32825=DIRECTION('center_axis',(-1.,0.,0.));
#32826=DIRECTION('ref_axis',(0.,0.,1.));
#32827=DIRECTION('',(0.,1.,0.));
#32828=DIRECTION('',(0.,0.,1.));
#32829=DIRECTION('center_axis',(-0.342020143325678,0.,0.939692620785905));
#32830=DIRECTION('ref_axis',(0.939692620785905,0.,0.342020143325678));
#32831=DIRECTION('',(0.939692620785905,0.,0.342020143325678));
#32832=DIRECTION('center_axis',(0.70710678118655,0.707106781186545,0.));
#32833=DIRECTION('ref_axis',(0.,0.,-1.));
#32834=DIRECTION('',(0.,0.,-1.));
#32835=DIRECTION('center_axis',(-0.342020143325678,0.,-0.939692620785905));
#32836=DIRECTION('ref_axis',(-0.939692620785905,0.,0.342020143325678));
#32837=DIRECTION('',(0.,1.,0.));
#32838=DIRECTION('',(-0.939692620785905,0.,0.342020143325678));
#32839=DIRECTION('center_axis',(-1.,0.,0.));
#32840=DIRECTION('ref_axis',(0.,0.,1.));
#32841=DIRECTION('',(0.,1.,0.));
#32842=DIRECTION('',(0.,0.,1.));
#32843=DIRECTION('center_axis',(-0.342020143325669,0.,0.939692620785908));
#32844=DIRECTION('ref_axis',(0.939692620785908,0.,0.342020143325669));
#32845=DIRECTION('',(0.939692620785908,0.,0.342020143325669));
#32846=DIRECTION('center_axis',(0.70710678118655,0.707106781186545,0.));
#32847=DIRECTION('ref_axis',(0.,0.,-1.));
#32848=DIRECTION('',(0.,0.,-1.));
#32849=DIRECTION('center_axis',(-0.342020143325678,0.,-0.939692620785905));
#32850=DIRECTION('ref_axis',(-0.939692620785905,0.,0.342020143325678));
#32851=DIRECTION('',(0.,1.,0.));
#32852=DIRECTION('',(-0.939692620785905,0.,0.342020143325678));
#32853=DIRECTION('center_axis',(-1.,0.,0.));
#32854=DIRECTION('ref_axis',(0.,0.,1.));
#32855=DIRECTION('',(0.,1.,0.));
#32856=DIRECTION('',(0.,0.,1.));
#32857=DIRECTION('center_axis',(-0.342020143325678,0.,0.939692620785905));
#32858=DIRECTION('ref_axis',(0.939692620785905,0.,0.342020143325678));
#32859=DIRECTION('',(0.939692620785905,0.,0.342020143325678));
#32860=DIRECTION('center_axis',(0.70710678118655,0.707106781186545,0.));
#32861=DIRECTION('ref_axis',(0.,0.,-1.));
#32862=DIRECTION('',(-0.633687274224646,0.63368727422465,0.443712606279641));
#32863=DIRECTION('',(0.,0.,-1.));
#32864=DIRECTION('center_axis',(-0.342020143325678,0.,-0.939692620785905));
#32865=DIRECTION('ref_axis',(-0.939692620785905,0.,0.342020143325678));
#32866=DIRECTION('',(0.,1.,0.));
#32867=DIRECTION('',(-0.939692620785905,0.,0.342020143325678));
#32868=DIRECTION('center_axis',(-1.,0.,0.));
#32869=DIRECTION('ref_axis',(0.,0.,1.));
#32870=DIRECTION('',(0.,0.,1.));
#32871=DIRECTION('center_axis',(0.241844762647985,0.707106781186537,-0.664463024388682));
#32872=DIRECTION('ref_axis',(-0.939692620785905,0.,-0.342020143325678));
#32873=DIRECTION('',(0.633687274224649,-0.633687274224649,-0.443712606279638));
#32874=DIRECTION('center_axis',(0.24184476264798,-0.707106781186534,-0.664463024388687));
#32875=DIRECTION('ref_axis',(-0.939692620785908,0.,-0.342020143325669));
#32876=DIRECTION('',(-0.633687274224649,-0.633687274224649,0.443712606279638));
#32877=DIRECTION('',(-0.939692620785908,0.,-0.342020143325669));
#32878=DIRECTION('',(0.633687274224652,0.633687274224654,-0.443712606279627));
#32879=DIRECTION('center_axis',(0.707106781186549,-0.707106781186546,0.));
#32880=DIRECTION('ref_axis',(0.,0.,-1.));
#32881=DIRECTION('',(0.,0.,-1.));
#32882=DIRECTION('',(0.633687274224661,0.633687274224648,0.443712606279622));
#32883=DIRECTION('center_axis',(0.241844762647997,-0.707106781186503,0.664463024388715));
#32884=DIRECTION('ref_axis',(0.939692620785905,0.,-0.342020143325678));
#32885=DIRECTION('',(0.939692620785905,0.,-0.342020143325678));
#32886=DIRECTION('',(0.633687274224667,0.633687274224667,0.443712606279586));
#32887=DIRECTION('center_axis',(0.,-1.,0.));
#32888=DIRECTION('ref_axis',(1.,0.,0.));
#32889=DIRECTION('',(0.,0.,-1.));
#32890=DIRECTION('',(0.939692620785905,0.,-0.342020143325678));
#32891=DIRECTION('',(0.,0.,-1.));
#32892=DIRECTION('',(-0.939692620785905,0.,-0.342020143325678));
#32893=DIRECTION('',(0.,0.,-1.));
#32894=DIRECTION('',(0.939692620785908,0.,-0.342020143325669));
#32895=DIRECTION('',(0.,0.,-1.));
#32896=DIRECTION('',(-0.939692620785908,0.,-0.342020143325669));
#32897=DIRECTION('',(0.,0.,-1.));
#32898=DIRECTION('',(-1.,0.,0.));
#32899=DIRECTION('',(0.,0.,-1.));
#32900=DIRECTION('',(0.,0.,-1.));
#32901=DIRECTION('',(-0.939692620785908,0.,-0.342020143325669));
#32902=DIRECTION('',(0.,0.,-1.));
#32903=DIRECTION('',(0.939692620785908,0.,-0.342020143325669));
#32904=DIRECTION('',(0.,0.,-1.));
#32905=DIRECTION('',(-0.939692620785908,0.,-0.342020143325669));
#32906=DIRECTION('',(0.,0.,-1.));
#32907=DIRECTION('',(0.939692620785908,0.,-0.342020143325669));
#32908=DIRECTION('',(0.,0.,-1.));
#32909=DIRECTION('',(0.939692620785908,0.,-0.342020143325669));
#32910=DIRECTION('',(0.,0.,-1.));
#32911=DIRECTION('',(-0.939692620785908,0.,-0.342020143325669));
#32912=DIRECTION('',(0.,0.,-1.));
#32913=DIRECTION('',(0.939692620785908,0.,-0.342020143325669));
#32914=DIRECTION('',(0.,0.,-1.));
#32915=DIRECTION('',(0.,0.,-1.));
#32916=DIRECTION('',(0.939692620785908,0.,-0.342020143325669));
#32917=DIRECTION('',(0.,0.,-1.));
#32918=DIRECTION('',(-0.939692620785908,0.,-0.342020143325669));
#32919=DIRECTION('',(0.,0.,-1.));
#32920=DIRECTION('',(0.939692620785908,0.,-0.342020143325669));
#32921=DIRECTION('',(0.,0.,-1.));
#32922=DIRECTION('',(-0.939692620785908,0.,-0.342020143325669));
#32923=DIRECTION('',(0.,0.,-1.));
#32924=DIRECTION('',(0.,0.,-1.));
#32925=DIRECTION('',(-0.939692620785908,0.,-0.342020143325669));
#32926=DIRECTION('',(0.,0.,-1.));
#32927=DIRECTION('',(0.939692620785908,0.,-0.342020143325669));
#32928=DIRECTION('',(0.,0.,-1.));
#32929=DIRECTION('',(-0.939692620785908,0.,-0.342020143325669));
#32930=DIRECTION('',(0.,0.,-1.));
#32931=DIRECTION('',(0.939692620785908,0.,-0.342020143325669));
#32932=DIRECTION('',(0.,0.,-1.));
#32933=DIRECTION('',(0.939692620785908,0.,-0.342020143325669));
#32934=DIRECTION('',(0.,0.,-1.));
#32935=DIRECTION('',(-0.939692620785908,0.,-0.342020143325669));
#32936=DIRECTION('',(0.,0.,-1.));
#32937=DIRECTION('',(0.939692620785908,0.,-0.342020143325669));
#32938=DIRECTION('',(0.,0.,-1.));
#32939=DIRECTION('',(-0.939692620785908,0.,-0.342020143325669));
#32940=DIRECTION('',(0.,0.,-1.));
#32941=DIRECTION('',(0.939692620785908,0.,-0.342020143325669));
#32942=DIRECTION('',(0.,0.,-1.));
#32943=DIRECTION('',(-0.939692620785908,0.,-0.342020143325669));
#32944=DIRECTION('',(0.,0.,-1.));
#32945=DIRECTION('',(0.939692620785908,0.,-0.342020143325669));
#32946=DIRECTION('',(0.,0.,-1.));
#32947=DIRECTION('',(0.,0.,-1.));
#32948=DIRECTION('',(0.939692620785908,0.,-0.342020143325669));
#32949=DIRECTION('',(0.,0.,-1.));
#32950=DIRECTION('',(-0.939692620785908,0.,-0.342020143325669));
#32951=DIRECTION('',(0.,0.,-1.));
#32952=DIRECTION('',(0.939692620785908,0.,-0.342020143325669));
#32953=DIRECTION('',(0.,0.,-1.));
#32954=DIRECTION('',(-0.939692620785908,0.,-0.342020143325669));
#32955=DIRECTION('',(0.,0.,-1.));
#32956=DIRECTION('',(0.,0.,-1.));
#32957=DIRECTION('',(-0.939692620785908,0.,-0.342020143325669));
#32958=DIRECTION('',(0.,0.,-1.));
#32959=DIRECTION('',(0.939692620785908,0.,-0.342020143325669));
#32960=DIRECTION('',(0.,0.,-1.));
#32961=DIRECTION('',(-0.939692620785905,0.,-0.342020143325678));
#32962=DIRECTION('',(0.,0.,-1.));
#32963=DIRECTION('',(0.939692620785905,0.,-0.342020143325678));
#32964=DIRECTION('',(0.,0.,-1.));
#32965=DIRECTION('',(-0.939692620785905,0.,-0.342020143325678));
#32966=DIRECTION('',(0.,0.,-1.));
#32967=DIRECTION('',(0.939692620785905,0.,-0.342020143325678));
#32968=DIRECTION('',(0.,0.,-1.));
#32969=DIRECTION('',(-0.939692620785905,0.,-0.342020143325678));
#32970=DIRECTION('',(0.,0.,-1.));
#32971=DIRECTION('',(0.939692620785905,0.,-0.342020143325678));
#32972=DIRECTION('',(0.,0.,-1.));
#32973=DIRECTION('',(-0.939692620785908,0.,-0.342020143325669));
#32974=DIRECTION('',(0.,0.,-1.));
#32975=DIRECTION('',(0.939692620785905,0.,-0.342020143325678));
#32976=DIRECTION('',(0.,0.,-1.));
#32977=DIRECTION('',(-0.939692620785905,0.,-0.342020143325678));
#32978=DIRECTION('',(0.,0.,-1.));
#32979=DIRECTION('',(0.939692620785905,0.,-0.342020143325678));
#32980=DIRECTION('',(0.,0.,-1.));
#32981=DIRECTION('',(0.,0.,-1.));
#32982=DIRECTION('',(-0.939692620785908,0.,-0.342020143325669));
#32983=DIRECTION('',(0.,0.,-1.));
#32984=DIRECTION('',(0.939692620785905,0.,-0.342020143325678));
#32985=DIRECTION('',(0.,0.,-1.));
#32986=DIRECTION('',(-0.939692620785905,0.,-0.342020143325678));
#32987=DIRECTION('',(0.,0.,-1.));
#32988=DIRECTION('',(0.939692620785905,0.,-0.342020143325678));
#32989=DIRECTION('',(0.,0.,-1.));
#32990=DIRECTION('',(0.,0.,-1.));
#32991=DIRECTION('',(0.939692620785905,0.,-0.342020143325678));
#32992=DIRECTION('',(0.,0.,-1.));
#32993=DIRECTION('',(-0.939692620785908,0.,-0.342020143325669));
#32994=DIRECTION('',(0.,0.,-1.));
#32995=DIRECTION('',(0.939692620785905,0.,-0.342020143325678));
#32996=DIRECTION('',(0.,0.,-1.));
#32997=DIRECTION('',(-0.939692620785905,0.,-0.342020143325678));
#32998=DIRECTION('',(0.,0.,-1.));
#32999=DIRECTION('',(0.939692620785905,0.,-0.342020143325678));
#33000=DIRECTION('',(0.,0.,-1.));
#33001=DIRECTION('',(-0.939692620785905,0.,-0.342020143325678));
#33002=DIRECTION('',(0.,0.,-1.));
#33003=DIRECTION('center_axis',(0.,-1.,0.));
#33004=DIRECTION('ref_axis',(0.,0.,1.));
#33005=DIRECTION('center_axis',(0.707106781186548,-0.707106781186548,0.));
#33006=DIRECTION('ref_axis',(0.,0.,-1.));
#33007=DIRECTION('',(0.63368727422465,0.63368727422465,0.443712606279634));
#33008=DIRECTION('center_axis',(0.241844762647985,-0.707106781186537,-0.664463024388682));
#33009=DIRECTION('ref_axis',(-0.939692620785905,0.,-0.342020143325678));
#33010=DIRECTION('',(-0.633687274224649,-0.633687274224649,0.443712606279638));
#33011=DIRECTION('',(0.633687274224635,0.633687274224637,-0.443712606279675));
#33012=DIRECTION('center_axis',(0.707106781186549,-0.707106781186546,0.));
#33013=DIRECTION('ref_axis',(0.,0.,-1.));
#33014=DIRECTION('',(0.633687274224642,0.633687274224633,0.443712606279672));
#33015=DIRECTION('center_axis',(0.241844762647985,-0.707106781186539,0.664463024388681));
#33016=DIRECTION('ref_axis',(0.939692620785905,0.,-0.342020143325678));
#33017=DIRECTION('',(0.633687274224648,0.633687274224648,0.443712606279641));
#33018=DIRECTION('center_axis',(0.707106781186548,-0.707106781186548,0.));
#33019=DIRECTION('ref_axis',(0.,0.,-1.));
#33020=DIRECTION('center_axis',(0.241844762647973,-0.707106781186573,-0.664463024388649));
#33021=DIRECTION('ref_axis',(-0.939692620785905,0.,-0.342020143325678));
#33022=DIRECTION('',(-0.63368727422463,-0.63368727422463,0.443712606279693));
#33023=DIRECTION('',(0.633687274224618,0.63368727422462,-0.443712606279723));
#33024=DIRECTION('center_axis',(0.707106781186549,-0.707106781186546,0.));
#33025=DIRECTION('ref_axis',(0.,0.,-1.));
#33026=DIRECTION('',(0.633687274224635,0.633687274224637,0.443712606279675));
#33027=DIRECTION('center_axis',(0.241844762647974,-0.70710678118657,0.664463024388651));
#33028=DIRECTION('ref_axis',(0.939692620785905,0.,-0.342020143325678));
#33029=DIRECTION('',(0.633687274224631,0.633687274224631,0.443712606279689));
#33030=DIRECTION('center_axis',(0.707106781186548,-0.707106781186548,0.));
#33031=DIRECTION('ref_axis',(0.,0.,-1.));
#33032=DIRECTION('center_axis',(0.24184476264798,-0.707106781186534,-0.664463024388687));
#33033=DIRECTION('ref_axis',(-0.939692620785908,0.,-0.342020143325669));
#33034=DIRECTION('',(-0.633687274224649,-0.633687274224649,0.443712606279638));
#33035=DIRECTION('',(0.633687274224652,0.633687274224654,-0.443712606279627));
#33036=DIRECTION('center_axis',(0.707106781186549,-0.707106781186546,0.));
#33037=DIRECTION('ref_axis',(0.,0.,-1.));
#33038=DIRECTION('',(0.63368727422465,0.633687274224655,0.443712606279628));
#33039=DIRECTION('center_axis',(0.241844762647986,-0.707106781186534,0.664463024388685));
#33040=DIRECTION('ref_axis',(0.939692620785905,0.,-0.342020143325678));
#33041=DIRECTION('',(0.63368727422465,0.63368727422465,0.443712606279634));
#33042=DIRECTION('center_axis',(0.707106781186548,-0.707106781186548,0.));
#33043=DIRECTION('ref_axis',(0.,0.,-1.));
#33044=DIRECTION('center_axis',(0.707106781186549,-0.707106781186546,0.));
#33045=DIRECTION('ref_axis',(0.,0.,-1.));
#33046=DIRECTION('',(0.633687274224652,0.633687274224654,0.443712606279627));
#33047=DIRECTION('center_axis',(0.241844762647986,-0.707106781186534,0.664463024388685));
#33048=DIRECTION('ref_axis',(0.939692620785905,0.,-0.342020143325678));
#33049=DIRECTION('',(0.63368727422465,0.63368727422465,0.443712606279634));
#33050=DIRECTION('center_axis',(0.707106781186548,-0.707106781186548,0.));
#33051=DIRECTION('ref_axis',(0.,0.,-1.));
#33052=DIRECTION('',(0.,0.,1.));
#33053=DIRECTION('center_axis',(0.241844762647973,-0.707106781186573,-0.664463024388649));
#33054=DIRECTION('ref_axis',(-0.939692620785905,0.,-0.342020143325678));
#33055=DIRECTION('',(-0.63368727422463,-0.63368727422463,0.443712606279693));
#33056=DIRECTION('',(0.633687274224635,0.633687274224637,-0.443712606279675));
#33057=DIRECTION('center_axis',(0.707106781186549,-0.707106781186546,0.));
#33058=DIRECTION('ref_axis',(0.,0.,-1.));
#33059=DIRECTION('',(0.633687274224635,0.633687274224637,0.443712606279675));
#33060=DIRECTION('center_axis',(0.241844762647974,-0.70710678118657,0.664463024388651));
#33061=DIRECTION('ref_axis',(0.939692620785905,0.,-0.342020143325678));
#33062=DIRECTION('',(0.633687274224631,0.633687274224631,0.443712606279689));
#33063=DIRECTION('center_axis',(0.707106781186548,-0.707106781186548,0.));
#33064=DIRECTION('ref_axis',(0.,0.,-1.));
#33065=DIRECTION('center_axis',(0.24184476264798,-0.707106781186536,-0.664463024388686));
#33066=DIRECTION('ref_axis',(-0.939692620785908,0.,-0.342020143325669));
#33067=DIRECTION('',(-0.633687274224648,-0.633687274224648,0.44371260627964));
#33068=DIRECTION('',(-0.633687274224647,-0.633687274224649,0.443712606279641));
#33069=DIRECTION('center_axis',(0.707106781186549,-0.707106781186546,0.));
#33070=DIRECTION('ref_axis',(0.,0.,-1.));
#33071=DIRECTION('center_axis',(0.707106781186549,-0.707106781186546,0.));
#33072=DIRECTION('ref_axis',(0.,0.,-1.));
#33073=DIRECTION('',(0.633687274224652,0.633687274224654,0.443712606279627));
#33074=DIRECTION('center_axis',(0.241844762647986,-0.707106781186536,0.664463024388684));
#33075=DIRECTION('ref_axis',(0.939692620785905,0.,-0.342020143325678));
#33076=DIRECTION('',(0.63368727422465,0.63368727422465,0.443712606279636));
#33077=DIRECTION('center_axis',(0.241844762647973,-0.707106781186572,-0.66446302438865));
#33078=DIRECTION('ref_axis',(-0.939692620785905,0.,-0.342020143325678));
#33079=DIRECTION('',(-0.63368727422463,-0.63368727422463,0.443712606279691));
#33080=DIRECTION('',(0.633687274224635,0.633687274224637,-0.443712606279675));
#33081=DIRECTION('center_axis',(0.707106781186549,-0.707106781186546,0.));
#33082=DIRECTION('ref_axis',(0.,0.,-1.));
#33083=DIRECTION('',(0.633687274224637,0.633687274224636,0.443712606279674));
#33084=DIRECTION('center_axis',(0.241844762647974,-0.70710678118657,0.664463024388651));
#33085=DIRECTION('ref_axis',(0.939692620785905,0.,-0.342020143325678));
#33086=DIRECTION('',(0.633687274224631,0.633687274224631,0.443712606279689));
#33087=DIRECTION('center_axis',(0.707106781186548,-0.707106781186548,0.));
#33088=DIRECTION('ref_axis',(0.,0.,-1.));
#33089=DIRECTION('center_axis',(0.241844762647992,-0.7071067811865,-0.664463024388719));
#33090=DIRECTION('ref_axis',(-0.939692620785908,0.,-0.342020143325669));
#33091=DIRECTION('',(-0.633687274224668,-0.633687274224668,0.443712606279585));
#33092=DIRECTION('',(0.633687274224669,0.633687274224671,-0.443712606279578));
#33093=DIRECTION('center_axis',(0.707106781186549,-0.707106781186546,0.));
#33094=DIRECTION('ref_axis',(0.,0.,-1.));
#33095=DIRECTION('',(0.633687274224652,0.633687274224654,0.443712606279627));
#33096=DIRECTION('center_axis',(0.241844762647986,-0.707106781186536,0.664463024388684));
#33097=DIRECTION('ref_axis',(0.939692620785905,0.,-0.342020143325678));
#33098=DIRECTION('',(0.63368727422465,0.63368727422465,0.443712606279636));
#33099=DIRECTION('center_axis',(0.707106781186548,-0.707106781186548,0.));
#33100=DIRECTION('ref_axis',(0.,0.,-1.));
#33101=DIRECTION('center_axis',(0.241844762647986,-0.707106781186536,-0.664463024388684));
#33102=DIRECTION('ref_axis',(-0.939692620785905,0.,-0.342020143325678));
#33103=DIRECTION('',(-0.63368727422465,-0.63368727422465,0.443712606279636));
#33104=DIRECTION('',(0.633687274224652,0.633687274224654,-0.443712606279627));
#33105=DIRECTION('center_axis',(0.707106781186549,-0.707106781186546,0.));
#33106=DIRECTION('ref_axis',(0.,0.,-1.));
#33107=DIRECTION('',(0.633687274224654,0.633687274224652,0.443712606279625));
#33108=DIRECTION('center_axis',(0.241844762647986,-0.707106781186536,0.664463024388684));
#33109=DIRECTION('ref_axis',(0.939692620785905,0.,-0.342020143325678));
#33110=DIRECTION('',(0.63368727422465,0.63368727422465,0.443712606279636));
#33111=DIRECTION('center_axis',(0.707106781186548,-0.707106781186548,0.));
#33112=DIRECTION('ref_axis',(0.,0.,-1.));
#33113=DIRECTION('center_axis',(0.241844762647973,-0.707106781186572,-0.66446302438865));
#33114=DIRECTION('ref_axis',(-0.939692620785905,0.,-0.342020143325678));
#33115=DIRECTION('',(-0.63368727422463,-0.63368727422463,0.443712606279691));
#33116=DIRECTION('',(0.633687274224635,0.633687274224637,-0.443712606279675));
#33117=DIRECTION('center_axis',(0.707106781186549,-0.707106781186546,0.));
#33118=DIRECTION('ref_axis',(0.,0.,-1.));
#33119=DIRECTION('',(0.633687274224643,0.63368727422466,0.443712606279631));
#33120=DIRECTION('center_axis',(0.241844762647986,-0.707106781186536,0.664463024388684));
#33121=DIRECTION('ref_axis',(0.939692620785905,0.,-0.342020143325678));
#33122=DIRECTION('',(0.63368727422465,0.63368727422465,0.443712606279636));
#33123=DIRECTION('center_axis',(0.707106781186548,-0.707106781186548,0.));
#33124=DIRECTION('ref_axis',(0.,0.,-1.));
#33125=DIRECTION('center_axis',(0.241844762647986,-0.707106781186536,-0.664463024388684));
#33126=DIRECTION('ref_axis',(-0.939692620785905,0.,-0.342020143325678));
#33127=DIRECTION('',(-0.63368727422465,-0.63368727422465,0.443712606279636));
#33128=DIRECTION('',(0.633687274224652,0.633687274224654,-0.443712606279627));
#33129=DIRECTION('center_axis',(0.707106781186549,-0.707106781186546,0.));
#33130=DIRECTION('ref_axis',(0.,0.,-1.));
#33131=DIRECTION('',(0.633687274224642,0.633687274224633,0.443712606279672));
#33132=DIRECTION('center_axis',(0.241844762647979,-0.707106781186536,0.664463024388685));
#33133=DIRECTION('ref_axis',(0.939692620785908,0.,-0.342020143325669));
#33134=DIRECTION('',(0.633687274224648,0.633687274224648,0.443712606279641));
#33135=DIRECTION('center_axis',(0.707106781186548,-0.707106781186548,0.));
#33136=DIRECTION('ref_axis',(0.,0.,-1.));
#33137=DIRECTION('center_axis',(0.24184476264798,-0.707106781186533,-0.664463024388688));
#33138=DIRECTION('ref_axis',(-0.939692620785908,0.,-0.342020143325669));
#33139=DIRECTION('',(-0.63368727422465,-0.63368727422465,0.443712606279635));
#33140=DIRECTION('',(0.633687274224652,0.633687274224654,-0.443712606279627));
#33141=DIRECTION('center_axis',(0.707106781186549,-0.707106781186546,0.));
#33142=DIRECTION('ref_axis',(0.,0.,-1.));
#33143=DIRECTION('center_axis',(0.707106781186548,-0.707106781186548,0.));
#33144=DIRECTION('ref_axis',(0.,0.,-1.));
#33145=DIRECTION('center_axis',(0.24184476264798,-0.707106781186535,-0.664463024388686));
#33146=DIRECTION('ref_axis',(-0.939692620785908,0.,-0.342020143325669));
#33147=DIRECTION('',(-0.633687274224649,-0.633687274224649,0.443712606279638));
#33148=DIRECTION('',(0.633687274224652,0.633687274224654,-0.443712606279627));
#33149=DIRECTION('center_axis',(0.707106781186549,-0.707106781186546,0.));
#33150=DIRECTION('ref_axis',(0.,0.,-1.));
#33151=DIRECTION('',(0.633687274224654,0.633687274224652,0.443712606279625));
#33152=DIRECTION('center_axis',(0.24184476264798,-0.707106781186534,0.664463024388688));
#33153=DIRECTION('ref_axis',(0.939692620785908,0.,-0.342020143325669));
#33154=DIRECTION('',(0.63368727422465,0.63368727422465,0.443712606279636));
#33155=DIRECTION('center_axis',(0.707106781186548,-0.707106781186548,0.));
#33156=DIRECTION('ref_axis',(0.,0.,-1.));
#33157=DIRECTION('center_axis',(0.241844762647979,-0.707106781186536,-0.664463024388685));
#33158=DIRECTION('ref_axis',(-0.939692620785908,0.,-0.342020143325669));
#33159=DIRECTION('',(-0.633687274224648,-0.633687274224648,0.443712606279641));
#33160=DIRECTION('',(0.633687274224635,0.633687274224637,-0.443712606279675));
#33161=DIRECTION('center_axis',(0.707106781186549,-0.707106781186546,0.));
#33162=DIRECTION('ref_axis',(0.,0.,-1.));
#33163=DIRECTION('',(0.633687274224676,0.633687274224666,0.443712606279575));
#33164=DIRECTION('center_axis',(0.241844762647992,-0.707106781186501,0.664463024388719));
#33165=DIRECTION('ref_axis',(0.939692620785908,0.,-0.342020143325669));
#33166=DIRECTION('',(0.633687274224667,0.633687274224667,0.443712606279586));
#33167=DIRECTION('center_axis',(0.707106781186548,-0.707106781186548,0.));
#33168=DIRECTION('ref_axis',(0.,0.,-1.));
#33169=DIRECTION('center_axis',(0.707106781186549,-0.707106781186546,0.));
#33170=DIRECTION('ref_axis',(0.,0.,-1.));
#33171=DIRECTION('',(0.63368727422467,0.63368727422467,0.443712606279578));
#33172=DIRECTION('center_axis',(0.241844762647992,-0.707106781186499,0.66446302438872));
#33173=DIRECTION('ref_axis',(0.939692620785908,0.,-0.342020143325669));
#33174=DIRECTION('',(0.633687274224668,0.633687274224668,0.443712606279584));
#33175=DIRECTION('center_axis',(0.707106781186548,-0.707106781186548,0.));
#33176=DIRECTION('ref_axis',(0.,0.,-1.));
#33177=DIRECTION('',(0.,0.,1.));
#33178=DIRECTION('center_axis',(0.24184476264798,-0.707106781186535,-0.664463024388686));
#33179=DIRECTION('ref_axis',(-0.939692620785908,0.,-0.342020143325669));
#33180=DIRECTION('',(-0.633687274224649,-0.633687274224649,0.443712606279638));
#33181=DIRECTION('',(0.633687274224652,0.633687274224654,-0.443712606279627));
#33182=DIRECTION('center_axis',(0.707106781186549,-0.707106781186546,0.));
#33183=DIRECTION('ref_axis',(0.,0.,-1.));
#33184=DIRECTION('',(0.633687274224666,0.633687274224673,0.44371260627958));
#33185=DIRECTION('center_axis',(0.241844762647993,-0.707106781186497,0.664463024388722));
#33186=DIRECTION('ref_axis',(0.939692620785908,0.,-0.342020143325669));
#33187=DIRECTION('',(0.633687274224669,0.633687274224669,0.44371260627958));
#33188=DIRECTION('center_axis',(0.707106781186548,-0.707106781186548,0.));
#33189=DIRECTION('ref_axis',(0.,0.,-1.));
#33190=DIRECTION('center_axis',(0.241844762647979,-0.707106781186536,-0.664463024388685));
#33191=DIRECTION('ref_axis',(-0.939692620785908,0.,-0.342020143325669));
#33192=DIRECTION('',(-0.633687274224648,-0.633687274224648,0.443712606279641));
#33193=DIRECTION('',(0.633687274224635,0.633687274224637,-0.443712606279675));
#33194=DIRECTION('center_axis',(0.707106781186549,-0.707106781186546,0.));
#33195=DIRECTION('ref_axis',(0.,0.,-1.));
#33196=DIRECTION('',(0.63368727422466,0.633687274224649,0.443712606279623));
#33197=DIRECTION('center_axis',(0.24184476264798,-0.707106781186536,0.664463024388686));
#33198=DIRECTION('ref_axis',(0.939692620785908,0.,-0.342020143325669));
#33199=DIRECTION('',(0.633687274224648,0.633687274224648,0.44371260627964));
#33200=DIRECTION('center_axis',(0.707106781186548,-0.707106781186548,0.));
#33201=DIRECTION('ref_axis',(0.,0.,-1.));
#33202=DIRECTION('center_axis',(0.24184476264798,-0.707106781186534,-0.664463024388688));
#33203=DIRECTION('ref_axis',(-0.939692620785908,0.,-0.342020143325669));
#33204=DIRECTION('',(-0.63368727422465,-0.63368727422465,0.443712606279636));
#33205=DIRECTION('',(0.633687274224652,0.633687274224654,-0.443712606279627));
#33206=DIRECTION('center_axis',(0.707106781186549,-0.707106781186546,0.));
#33207=DIRECTION('ref_axis',(0.,0.,-1.));
#33208=DIRECTION('',(-0.633687274224648,-0.63368727422465,-0.443712606279639));
#33209=DIRECTION('center_axis',(0.24184476264798,-0.707106781186534,0.664463024388687));
#33210=DIRECTION('ref_axis',(0.939692620785908,0.,-0.342020143325669));
#33211=DIRECTION('center_axis',(0.707106781186549,-0.707106781186546,0.));
#33212=DIRECTION('ref_axis',(0.,0.,-1.));
#33213=DIRECTION('',(0.633687274224664,0.633687274224674,0.44371260627958));
#33214=DIRECTION('center_axis',(0.241844762647993,-0.707106781186497,0.664463024388722));
#33215=DIRECTION('ref_axis',(0.939692620785908,0.,-0.342020143325669));
#33216=DIRECTION('',(0.633687274224669,0.633687274224669,0.44371260627958));
#33217=DIRECTION('center_axis',(0.241844762647979,-0.707106781186536,-0.664463024388685));
#33218=DIRECTION('ref_axis',(-0.939692620785908,0.,-0.342020143325669));
#33219=DIRECTION('',(-0.633687274224648,-0.633687274224648,0.443712606279641));
#33220=DIRECTION('',(0.633687274224635,0.633687274224637,-0.443712606279675));
#33221=DIRECTION('center_axis',(0.707106781186549,-0.707106781186546,0.));
#33222=DIRECTION('ref_axis',(0.,0.,-1.));
#33223=DIRECTION('',(0.633687274224658,0.63368727422465,0.443712606279624));
#33224=DIRECTION('center_axis',(0.24184476264798,-0.707106781186536,0.664463024388686));
#33225=DIRECTION('ref_axis',(0.939692620785908,0.,-0.342020143325669));
#33226=DIRECTION('',(0.633687274224648,0.633687274224648,0.44371260627964));
#33227=DIRECTION('center_axis',(0.707106781186548,-0.707106781186548,0.));
#33228=DIRECTION('ref_axis',(0.,0.,-1.));
#33229=DIRECTION('center_axis',(0.241844762647993,-0.707106781186498,-0.664463024388721));
#33230=DIRECTION('ref_axis',(-0.939692620785908,0.,-0.342020143325669));
#33231=DIRECTION('',(-0.633687274224669,-0.633687274224669,0.443712606279582));
#33232=DIRECTION('',(0.633687274224669,0.633687274224671,-0.443712606279578));
#33233=DIRECTION('center_axis',(0.707106781186549,-0.707106781186546,0.));
#33234=DIRECTION('ref_axis',(0.,0.,-1.));
#33235=DIRECTION('center_axis',(0.707106781186548,-0.707106781186548,0.));
#33236=DIRECTION('ref_axis',(0.,0.,-1.));
#33237=DIRECTION('center_axis',(0.24184476264798,-0.707106781186535,-0.664463024388686));
#33238=DIRECTION('ref_axis',(-0.939692620785908,0.,-0.342020143325669));
#33239=DIRECTION('',(-0.633687274224649,-0.633687274224649,0.443712606279638));
#33240=DIRECTION('',(0.633687274224652,0.633687274224654,-0.443712606279627));
#33241=DIRECTION('center_axis',(0.707106781186549,-0.707106781186546,0.));
#33242=DIRECTION('ref_axis',(0.,0.,-1.));
#33243=DIRECTION('',(0.633687274224664,0.633687274224674,0.44371260627958));
#33244=DIRECTION('center_axis',(0.241844762647993,-0.707106781186497,0.664463024388722));
#33245=DIRECTION('ref_axis',(0.939692620785908,0.,-0.342020143325669));
#33246=DIRECTION('',(0.633687274224669,0.633687274224669,0.44371260627958));
#33247=DIRECTION('center_axis',(0.707106781186548,-0.707106781186548,0.));
#33248=DIRECTION('ref_axis',(0.,0.,-1.));
#33249=DIRECTION('center_axis',(0.241844762647979,-0.707106781186536,-0.664463024388685));
#33250=DIRECTION('ref_axis',(-0.939692620785908,0.,-0.342020143325669));
#33251=DIRECTION('',(-0.633687274224648,-0.633687274224648,0.443712606279641));
#33252=DIRECTION('',(0.633687274224635,0.633687274224637,-0.443712606279675));
#33253=DIRECTION('center_axis',(0.707106781186549,-0.707106781186546,0.));
#33254=DIRECTION('ref_axis',(0.,0.,-1.));
#33255=DIRECTION('',(0.633687274224658,0.63368727422465,0.443712606279624));
#33256=DIRECTION('center_axis',(0.24184476264798,-0.707106781186536,0.664463024388686));
#33257=DIRECTION('ref_axis',(0.939692620785908,0.,-0.342020143325669));
#33258=DIRECTION('',(0.633687274224648,0.633687274224648,0.44371260627964));
#33259=DIRECTION('center_axis',(0.707106781186548,-0.707106781186548,0.));
#33260=DIRECTION('ref_axis',(0.,0.,-1.));
#33261=DIRECTION('center_axis',(0.707106781186549,-0.707106781186546,0.));
#33262=DIRECTION('ref_axis',(0.,0.,-1.));
#33263=DIRECTION('',(0.633687274224653,0.633687274224653,0.443712606279626));
#33264=DIRECTION('center_axis',(0.24184476264798,-0.707106781186534,0.664463024388687));
#33265=DIRECTION('ref_axis',(0.939692620785908,0.,-0.342020143325669));
#33266=DIRECTION('',(0.633687274224649,0.633687274224649,0.443712606279638));
#33267=DIRECTION('center_axis',(0.707106781186548,-0.707106781186548,0.));
#33268=DIRECTION('ref_axis',(0.,0.,-1.));
#33269=DIRECTION('',(0.,0.,1.));
#33270=DIRECTION('center_axis',(0.241844762647992,-0.7071067811865,-0.66446302438872));
#33271=DIRECTION('ref_axis',(-0.939692620785908,0.,-0.342020143325669));
#33272=DIRECTION('',(-0.633687274224668,-0.633687274224668,0.443712606279584));
#33273=DIRECTION('',(-0.633687274224667,-0.633687274224668,0.443712606279585));
#33274=DIRECTION('center_axis',(0.707106781186549,-0.707106781186546,0.));
#33275=DIRECTION('ref_axis',(0.,0.,-1.));
#33276=DIRECTION('',(0.633687274224648,0.633687274224657,0.443712606279629));
#33277=DIRECTION('center_axis',(0.241844762647991,-0.707106781186501,0.664463024388718));
#33278=DIRECTION('ref_axis',(0.939692620785908,0.,-0.342020143325669));
#33279=DIRECTION('center_axis',(0.707106781186549,-0.707106781186546,0.));
#33280=DIRECTION('ref_axis',(0.,0.,-1.));
#33281=DIRECTION('',(0.633687274224658,0.63368727422465,0.443712606279624));
#33282=DIRECTION('center_axis',(0.24184476264798,-0.707106781186536,0.664463024388686));
#33283=DIRECTION('ref_axis',(0.939692620785908,0.,-0.342020143325669));
#33284=DIRECTION('',(0.633687274224648,0.633687274224648,0.44371260627964));
#33285=DIRECTION('center_axis',(0.241844762647968,-0.70710678118657,-0.664463024388653));
#33286=DIRECTION('ref_axis',(-0.939692620785908,0.,-0.342020143325669));
#33287=DIRECTION('',(-0.63368727422463,-0.63368727422463,0.443712606279692));
#33288=DIRECTION('',(0.633687274224635,0.633687274224637,-0.443712606279675));
#33289=DIRECTION('center_axis',(0.707106781186549,-0.707106781186546,0.));
#33290=DIRECTION('ref_axis',(0.,0.,-1.));
#33291=DIRECTION('',(0.633687274224652,0.633687274224654,0.443712606279627));
#33292=DIRECTION('center_axis',(0.24184476264798,-0.707106781186534,0.664463024388687));
#33293=DIRECTION('ref_axis',(0.939692620785908,0.,-0.342020143325669));
#33294=DIRECTION('',(0.633687274224649,0.633687274224649,0.443712606279637));
#33295=DIRECTION('center_axis',(0.707106781186548,-0.707106781186548,0.));
#33296=DIRECTION('ref_axis',(0.,0.,-1.));
#33297=DIRECTION('center_axis',(0.241844762647992,-0.7071067811865,-0.664463024388719));
#33298=DIRECTION('ref_axis',(-0.939692620785908,0.,-0.342020143325669));
#33299=DIRECTION('',(-0.633687274224668,-0.633687274224668,0.443712606279585));
#33300=DIRECTION('',(0.633687274224669,0.633687274224671,-0.443712606279578));
#33301=DIRECTION('center_axis',(0.707106781186549,-0.707106781186546,0.));
#33302=DIRECTION('ref_axis',(0.,0.,-1.));
#33303=DIRECTION('center_axis',(0.707106781186548,-0.707106781186548,0.));
#33304=DIRECTION('ref_axis',(0.,0.,-1.));
#33305=DIRECTION('center_axis',(0.,-0.923879532511285,-0.382683432365094));
#33306=DIRECTION('ref_axis',(0.,0.382683432365094,-0.923879532511285));
#33307=DIRECTION('',(0.67859834454585,-0.281084637714822,0.678598344545844));
#33308=DIRECTION('',(-0.357406744336596,-0.357406744336596,0.862856209461014));
#33309=DIRECTION('center_axis',(0.241844762647955,-0.707106781186607,-0.664463024388618));
#33310=DIRECTION('ref_axis',(-0.939692620785908,0.,-0.342020143325669));
#33311=DIRECTION('',(-0.63368727422461,-0.63368727422461,0.443712606279749));
#33312=DIRECTION('',(0.633687274224618,0.63368727422462,-0.443712606279723));
#33313=DIRECTION('center_axis',(0.707106781186549,-0.707106781186546,0.));
#33314=DIRECTION('ref_axis',(0.,0.,-1.));
#33315=DIRECTION('',(0.63368727422467,0.633687274224642,0.443712606279618));
#33316=DIRECTION('center_axis',(0.241844762647992,-0.7071067811865,0.664463024388719));
#33317=DIRECTION('ref_axis',(0.939692620785908,0.,-0.342020143325669));
#33318=DIRECTION('',(0.633687274224668,0.633687274224668,0.443712606279585));
#33319=DIRECTION('center_axis',(0.707106781186548,-0.707106781186548,0.));
#33320=DIRECTION('ref_axis',(0.,0.,-1.));
#33321=DIRECTION('center_axis',(0.241844762647973,-0.707106781186573,-0.664463024388649));
#33322=DIRECTION('ref_axis',(-0.939692620785905,0.,-0.342020143325678));
#33323=DIRECTION('',(-0.63368727422463,-0.63368727422463,0.443712606279693));
#33324=DIRECTION('',(0.633687274224618,0.63368727422462,-0.443712606279723));
#33325=DIRECTION('center_axis',(0.707106781186549,-0.707106781186546,0.));
#33326=DIRECTION('ref_axis',(0.,0.,-1.));
#33327=DIRECTION('',(0.633687274224648,0.633687274224657,0.443712606279629));
#33328=DIRECTION('center_axis',(0.241844762647986,-0.707106781186534,0.664463024388685));
#33329=DIRECTION('ref_axis',(0.939692620785905,0.,-0.342020143325678));
#33330=DIRECTION('center_axis',(0.707106781186548,-0.707106781186548,0.));
#33331=DIRECTION('ref_axis',(0.,0.,-1.));
#33332=DIRECTION('',(0.501874170540788,-0.864940643595846,-2.73831019897557E-14));
#33333=DIRECTION('center_axis',(0.,1.,0.));
#33334=DIRECTION('ref_axis',(0.,0.,1.));
#33335=DIRECTION('center_axis',(0.,1.,0.));
#33336=DIRECTION('ref_axis',(0.,0.,1.));
#33337=DIRECTION('',(0.,1.,0.));
#33338=DIRECTION('center_axis',(0.,0.,1.));
#33339=DIRECTION('ref_axis',(1.,0.,0.));
#33340=DIRECTION('center_axis',(0.,0.,1.));
#33341=DIRECTION('ref_axis',(1.,0.,0.));
#33342=DIRECTION('',(0.,0.,1.));
#33343=DIRECTION('center_axis',(0.,0.,1.));
#33344=DIRECTION('ref_axis',(1.,0.,0.));
#33345=DIRECTION('center_axis',(0.,-1.,0.));
#33346=DIRECTION('ref_axis',(0.,0.,1.));
#33347=DIRECTION('',(-8.65956056235501E-17,0.707106781186541,0.707106781186554));
#33348=DIRECTION('center_axis',(0.,0.,-1.));
#33349=DIRECTION('ref_axis',(1.,0.,0.));
#33350=DIRECTION('',(0.707106781186551,-8.65956056235498E-17,0.707106781186544));
#33351=DIRECTION('center_axis',(0.,0.,-1.));
#33352=DIRECTION('ref_axis',(1.,0.,0.));
#33353=DIRECTION('',(0.857167300702111,1.04972719113862E-16,0.515038074910056));
#33354=DIRECTION('center_axis',(0.707106781186548,0.707106781186548,0.));
#33355=DIRECTION('ref_axis',(0.,0.,-1.));
#33356=DIRECTION('',(0.,0.,-1.));
#33357=DIRECTION('',(-0.577350269189628,0.577350269189628,-0.577350269189622));
#33358=DIRECTION('center_axis',(0.707106781186548,0.707106781186548,0.));
#33359=DIRECTION('ref_axis',(0.,0.,-1.));
#33360=DIRECTION('',(0.,0.,-1.));
#33361=DIRECTION('center_axis',(1.,0.,0.));
#33362=DIRECTION('ref_axis',(0.,1.,0.));
#33363=DIRECTION('',(0.,0.,1.));
#33364=DIRECTION('',(0.,-1.,0.));
#33365=DIRECTION('center_axis',(1.,0.,0.));
#33366=DIRECTION('ref_axis',(0.,1.,0.));
#33367=DIRECTION('center_axis',(1.,0.,0.));
#33368=DIRECTION('ref_axis',(0.,1.,0.));
#33369=DIRECTION('center_axis',(1.,0.,0.));
#33370=DIRECTION('ref_axis',(0.,1.,0.));
#33371=DIRECTION('center_axis',(1.,0.,0.));
#33372=DIRECTION('ref_axis',(0.,1.,0.));
#33373=DIRECTION('center_axis',(1.,0.,0.));
#33374=DIRECTION('ref_axis',(0.,1.,0.));
#33375=DIRECTION('center_axis',(1.,0.,0.));
#33376=DIRECTION('ref_axis',(0.,1.,0.));
#33377=DIRECTION('center_axis',(0.707106781186548,-0.707106781186548,0.));
#33378=DIRECTION('ref_axis',(0.,0.,-1.));
#33379=DIRECTION('',(0.577350269189628,0.577350269189628,0.577350269189622));
#33380=DIRECTION('center_axis',(0.707106781186548,-0.707106781186548,0.));
#33381=DIRECTION('ref_axis',(0.,0.,-1.));
#33382=DIRECTION('center_axis',(0.707106781186548,-0.707106781186548,0.));
#33383=DIRECTION('ref_axis',(0.,0.,-1.));
#33384=DIRECTION('center_axis',(0.707106781186548,-0.707106781186548,0.));
#33385=DIRECTION('ref_axis',(0.,0.,-1.));
#33386=DIRECTION('center_axis',(0.,0.707106781186561,0.707106781186534));
#33387=DIRECTION('ref_axis',(1.,0.,0.));
#33388=DIRECTION('',(1.,0.,0.));
#33389=DIRECTION('',(0.577350269189618,0.577350269189618,-0.577350269189641));
#33390=DIRECTION('center_axis',(0.707106781186544,0.,-0.707106781186551));
#33391=DIRECTION('ref_axis',(-0.707106781186551,0.,-0.707106781186544));
#33392=DIRECTION('',(0.577350269189628,0.577350269189628,0.577350269189622));
#33393=DIRECTION('center_axis',(0.707106781186561,0.,0.707106781186534));
#33394=DIRECTION('ref_axis',(0.707106781186534,0.,-0.707106781186561));
#33395=DIRECTION('',(0.,-1.,0.));
#33396=DIRECTION('center_axis',(0.,0.707106781186544,-0.707106781186551));
#33397=DIRECTION('ref_axis',(-1.,0.,0.));
#33398=DIRECTION('center_axis',(0.,0.,1.));
#33399=DIRECTION('ref_axis',(1.,0.,0.));
#33400=DIRECTION('center_axis',(-1.,0.,0.));
#33401=DIRECTION('ref_axis',(0.,-1.,0.));
#33402=DIRECTION('axis',(0.,0.,1.));
#33403=DIRECTION('refdir',(1.,0.,0.));
#33404=DIRECTION('center_axis',(0.942522113366887,-0.334143780152224,0.));
#33405=DIRECTION('ref_axis',(0.,0.,-1.));
#33406=DIRECTION('',(-0.334143780152224,-0.942522113366887,0.));
#33407=DIRECTION('',(0.,0.,1.));
#33408=DIRECTION('',(0.334143780152224,0.942522113366887,0.));
#33409=DIRECTION('',(0.,0.,-1.));
#33410=DIRECTION('center_axis',(0.,0.,1.));
#33411=DIRECTION('ref_axis',(1.,0.,0.));
#33412=DIRECTION('center_axis',(0.,0.,1.));
#33413=DIRECTION('ref_axis',(1.,0.,0.));
#33414=DIRECTION('',(0.,0.,-1.));
#33415=DIRECTION('center_axis',(0.,0.,1.));
#33416=DIRECTION('ref_axis',(1.,0.,0.));
#33417=DIRECTION('center_axis',(0.334143780152225,-0.942522113366886,0.));
#33418=DIRECTION('ref_axis',(0.,0.,-1.));
#33419=DIRECTION('',(0.942522113366886,0.334143780152225,0.));
#33420=DIRECTION('',(-0.942522113366886,-0.334143780152225,0.));
#33421=DIRECTION('',(0.,0.,1.));
#33422=DIRECTION('center_axis',(-0.942522113366889,-0.334143780152217,0.));
#33423=DIRECTION('ref_axis',(0.,0.,1.));
#33424=DIRECTION('',(0.334143780152217,-0.942522113366889,0.));
#33425=DIRECTION('',(0.,0.,-1.));
#33426=DIRECTION('',(-0.334143780152217,0.942522113366889,0.));
#33427=DIRECTION('',(0.,0.,1.));
#33428=DIRECTION('center_axis',(0.,0.,1.));
#33429=DIRECTION('ref_axis',(1.,0.,0.));
#33430=DIRECTION('center_axis',(0.,0.,1.));
#33431=DIRECTION('ref_axis',(1.,0.,0.));
#33432=DIRECTION('',(0.,0.,1.));
#33433=DIRECTION('center_axis',(0.,0.,1.));
#33434=DIRECTION('ref_axis',(1.,0.,0.));
#33435=DIRECTION('center_axis',(-0.334143780152224,-0.942522113366887,0.));
#33436=DIRECTION('ref_axis',(0.,0.,-1.));
#33437=DIRECTION('',(-0.942522113366887,0.334143780152224,0.));
#33438=DIRECTION('',(0.942522113366887,-0.334143780152224,0.));
#33439=DIRECTION('',(0.,0.,-1.));
#33440=DIRECTION('center_axis',(0.902739110616947,0.430188444943055,0.));
#33441=DIRECTION('ref_axis',(0.,0.,-1.));
#33442=DIRECTION('',(0.430188444943055,-0.902739110616947,0.));
#33443=DIRECTION('',(0.,0.,1.));
#33444=DIRECTION('',(-0.430188444943055,0.902739110616947,0.));
#33445=DIRECTION('',(0.,0.,-1.));
#33446=DIRECTION('center_axis',(0.,0.,1.));
#33447=DIRECTION('ref_axis',(-1.,-1.22464679914735E-16,0.));
#33448=DIRECTION('center_axis',(0.,0.,1.));
#33449=DIRECTION('ref_axis',(1.,0.,0.));
#33450=DIRECTION('',(0.,0.,-1.));
#33451=DIRECTION('center_axis',(0.,0.,1.));
#33452=DIRECTION('ref_axis',(1.,0.,0.));
#33453=DIRECTION('center_axis',(0.902739110616947,-0.430188444943055,0.));
#33454=DIRECTION('ref_axis',(0.,0.,-1.));
#33455=DIRECTION('',(0.430188444943055,0.902739110616947,0.));
#33456=DIRECTION('',(-0.430188444943055,-0.902739110616947,0.));
#33457=DIRECTION('',(0.,0.,1.));
#33458=DIRECTION('center_axis',(0.430188444943055,0.902739110616947,0.));
#33459=DIRECTION('ref_axis',(0.,0.,1.));
#33460=DIRECTION('',(-0.902739110616947,0.430188444943055,0.));
#33461=DIRECTION('',(0.,0.,-1.));
#33462=DIRECTION('',(0.902739110616947,-0.430188444943055,0.));
#33463=DIRECTION('',(0.,0.,1.));
#33464=DIRECTION('center_axis',(0.,0.,1.));
#33465=DIRECTION('ref_axis',(1.,0.,0.));
#33466=DIRECTION('center_axis',(0.,0.,1.));
#33467=DIRECTION('ref_axis',(1.,0.,0.));
#33468=DIRECTION('',(0.,0.,1.));
#33469=DIRECTION('center_axis',(0.,0.,1.));
#33470=DIRECTION('ref_axis',(1.,0.,0.));
#33471=DIRECTION('center_axis',(-0.430188444943055,0.902739110616947,0.));
#33472=DIRECTION('ref_axis',(0.,0.,1.));
#33473=DIRECTION('',(0.902739110616947,0.430188444943055,0.));
#33474=DIRECTION('',(-0.902739110616947,-0.430188444943055,0.));
#33475=DIRECTION('',(0.,0.,-1.));
#33476=DIRECTION('center_axis',(0.334143780152223,0.942522113366887,0.));
#33477=DIRECTION('ref_axis',(0.,0.,1.));
#33478=DIRECTION('',(0.942522113366887,-0.334143780152223,0.));
#33479=DIRECTION('',(0.,0.,1.));
#33480=DIRECTION('',(-0.942522113366887,0.334143780152223,0.));
#33481=DIRECTION('',(0.,0.,-1.));
#33482=DIRECTION('center_axis',(0.,0.,1.));
#33483=DIRECTION('ref_axis',(1.,0.,0.));
#33484=DIRECTION('center_axis',(0.,0.,1.));
#33485=DIRECTION('ref_axis',(1.,0.,0.));
#33486=DIRECTION('',(0.,0.,-1.));
#33487=DIRECTION('center_axis',(0.,0.,1.));
#33488=DIRECTION('ref_axis',(1.,0.,0.));
#33489=DIRECTION('center_axis',(0.942522113366887,0.334143780152223,0.));
#33490=DIRECTION('ref_axis',(0.,0.,-1.));
#33491=DIRECTION('',(-0.334143780152223,0.942522113366887,0.));
#33492=DIRECTION('',(0.334143780152223,-0.942522113366887,0.));
#33493=DIRECTION('',(0.,0.,1.));
#33494=DIRECTION('center_axis',(-0.334143780152223,0.942522113366887,0.));
#33495=DIRECTION('ref_axis',(0.,0.,1.));
#33496=DIRECTION('',(-0.942522113366887,-0.334143780152223,0.));
#33497=DIRECTION('',(0.,0.,-1.));
#33498=DIRECTION('',(0.942522113366887,0.334143780152223,0.));
#33499=DIRECTION('',(0.,0.,1.));
#33500=DIRECTION('center_axis',(0.,0.,1.));
#33501=DIRECTION('ref_axis',(1.,0.,0.));
#33502=DIRECTION('center_axis',(0.,0.,1.));
#33503=DIRECTION('ref_axis',(1.,0.,0.));
#33504=DIRECTION('',(0.,0.,1.));
#33505=DIRECTION('center_axis',(0.,0.,1.));
#33506=DIRECTION('ref_axis',(1.,0.,0.));
#33507=DIRECTION('center_axis',(-0.942522113366887,0.334143780152223,0.));
#33508=DIRECTION('ref_axis',(0.,0.,1.));
#33509=DIRECTION('',(0.334143780152223,0.942522113366887,0.));
#33510=DIRECTION('',(-0.334143780152223,-0.942522113366887,0.));
#33511=DIRECTION('',(0.,0.,-1.));
#33512=DIRECTION('center_axis',(-0.902739110616947,0.430188444943055,0.));
#33513=DIRECTION('ref_axis',(0.,0.,1.));
#33514=DIRECTION('',(-0.430188444943055,-0.902739110616947,0.));
#33515=DIRECTION('',(0.,0.,-1.));
#33516=DIRECTION('',(0.430188444943055,0.902739110616947,0.));
#33517=DIRECTION('',(0.,0.,1.));
#33518=DIRECTION('center_axis',(0.,0.,1.));
#33519=DIRECTION('ref_axis',(1.,0.,0.));
#33520=DIRECTION('center_axis',(0.,0.,1.));
#33521=DIRECTION('ref_axis',(1.,0.,0.));
#33522=DIRECTION('',(0.,0.,1.));
#33523=DIRECTION('center_axis',(0.,0.,1.));
#33524=DIRECTION('ref_axis',(1.,0.,0.));
#33525=DIRECTION('center_axis',(-0.902739110616947,-0.430188444943055,0.));
#33526=DIRECTION('ref_axis',(0.,0.,1.));
#33527=DIRECTION('',(-0.430188444943055,0.902739110616947,0.));
#33528=DIRECTION('',(0.430188444943055,-0.902739110616947,0.));
#33529=DIRECTION('',(0.,0.,-1.));
#33530=DIRECTION('center_axis',(-0.430188444943055,-0.902739110616947,0.));
#33531=DIRECTION('ref_axis',(0.,0.,-1.));
#33532=DIRECTION('',(0.902739110616947,-0.430188444943055,0.));
#33533=DIRECTION('',(0.,0.,-1.));
#33534=DIRECTION('',(-0.902739110616947,0.430188444943055,0.));
#33535=DIRECTION('',(0.,0.,1.));
#33536=DIRECTION('center_axis',(0.,0.,1.));
#33537=DIRECTION('ref_axis',(1.,0.,0.));
#33538=DIRECTION('center_axis',(0.,0.,1.));
#33539=DIRECTION('ref_axis',(1.,0.,0.));
#33540=DIRECTION('',(0.,0.,1.));
#33541=DIRECTION('center_axis',(0.,0.,1.));
#33542=DIRECTION('ref_axis',(1.,0.,0.));
#33543=DIRECTION('center_axis',(0.430188444943055,-0.902739110616947,0.));
#33544=DIRECTION('ref_axis',(0.,0.,-1.));
#33545=DIRECTION('',(-0.902739110616947,-0.430188444943055,0.));
#33546=DIRECTION('',(0.902739110616947,0.430188444943055,0.));
#33547=DIRECTION('',(0.,0.,-1.));
#33548=DIRECTION('center_axis',(0.,0.,1.));
#33549=DIRECTION('ref_axis',(1.,0.,0.));
#33550=DIRECTION('center_axis',(0.,0.,1.));
#33551=DIRECTION('ref_axis',(1.,0.,0.));
#33552=DIRECTION('center_axis',(0.,0.,1.));
#33553=DIRECTION('ref_axis',(1.,0.,0.));
#33554=DIRECTION('center_axis',(0.,0.,-1.));
#33555=DIRECTION('ref_axis',(1.,0.,0.));
#33556=DIRECTION('center_axis',(0.,0.,1.));
#33557=DIRECTION('ref_axis',(1.,0.,0.));
#33558=DIRECTION('center_axis',(0.,0.,1.));
#33559=DIRECTION('ref_axis',(1.,0.,0.));
#33560=DIRECTION('center_axis',(0.,0.,1.));
#33561=DIRECTION('ref_axis',(1.,0.,0.));
#33562=DIRECTION('center_axis',(0.,0.,1.));
#33563=DIRECTION('ref_axis',(1.,0.,0.));
#33564=DIRECTION('center_axis',(0.,0.,-1.));
#33565=DIRECTION('ref_axis',(1.,0.,0.));
#33566=DIRECTION('center_axis',(0.,0.,-1.));
#33567=DIRECTION('ref_axis',(1.,0.,0.));
#33568=DIRECTION('center_axis',(0.,0.,1.));
#33569=DIRECTION('ref_axis',(1.,0.,0.));
#33570=DIRECTION('center_axis',(0.,0.,1.));
#33571=DIRECTION('ref_axis',(1.,0.,0.));
#33572=DIRECTION('center_axis',(0.,0.,1.));
#33573=DIRECTION('ref_axis',(1.,0.,0.));
#33574=DIRECTION('center_axis',(0.,0.,-1.));
#33575=DIRECTION('ref_axis',(1.,0.,0.));
#33576=DIRECTION('center_axis',(0.,0.,1.));
#33577=DIRECTION('ref_axis',(1.,0.,0.));
#33578=DIRECTION('center_axis',(0.,0.,-1.));
#33579=DIRECTION('ref_axis',(1.,0.,0.));
#33580=DIRECTION('center_axis',(0.,0.,1.));
#33581=DIRECTION('ref_axis',(1.,0.,0.));
#33582=DIRECTION('center_axis',(0.,0.,1.));
#33583=DIRECTION('ref_axis',(1.,0.,0.));
#33584=DIRECTION('center_axis',(0.,0.,1.));
#33585=DIRECTION('ref_axis',(1.,0.,0.));
#33586=DIRECTION('center_axis',(0.,0.,1.));
#33587=DIRECTION('ref_axis',(1.,0.,0.));
#33588=DIRECTION('center_axis',(0.,0.,1.));
#33589=DIRECTION('ref_axis',(1.,0.,0.));
#33590=DIRECTION('center_axis',(0.,0.,-1.));
#33591=DIRECTION('ref_axis',(1.,0.,0.));
#33592=DIRECTION('center_axis',(0.,0.,1.));
#33593=DIRECTION('ref_axis',(1.,0.,0.));
#33594=DIRECTION('center_axis',(0.,0.,-1.));
#33595=DIRECTION('ref_axis',(1.,0.,0.));
#33596=DIRECTION('center_axis',(0.,0.,1.));
#33597=DIRECTION('ref_axis',(1.,0.,0.));
#33598=DIRECTION('center_axis',(0.,0.,1.));
#33599=DIRECTION('ref_axis',(1.,0.,0.));
#33600=DIRECTION('center_axis',(0.,0.,1.));
#33601=DIRECTION('ref_axis',(1.,0.,0.));
#33602=DIRECTION('center_axis',(0.,0.,1.));
#33603=DIRECTION('ref_axis',(1.,0.,0.));
#33604=DIRECTION('center_axis',(0.,0.,1.));
#33605=DIRECTION('ref_axis',(1.,0.,0.));
#33606=DIRECTION('center_axis',(0.,0.,-1.));
#33607=DIRECTION('ref_axis',(1.,0.,0.));
#33608=DIRECTION('center_axis',(0.,0.,1.));
#33609=DIRECTION('ref_axis',(1.,0.,0.));
#33610=DIRECTION('center_axis',(0.,0.,-1.));
#33611=DIRECTION('ref_axis',(1.,0.,0.));
#33612=DIRECTION('center_axis',(0.,0.,1.));
#33613=DIRECTION('ref_axis',(1.,0.,0.));
#33614=DIRECTION('center_axis',(0.,0.,1.));
#33615=DIRECTION('ref_axis',(1.,0.,0.));
#33616=DIRECTION('center_axis',(0.,0.,1.));
#33617=DIRECTION('ref_axis',(1.,0.,0.));
#33618=DIRECTION('center_axis',(0.,0.,1.));
#33619=DIRECTION('ref_axis',(1.,0.,0.));
#33620=DIRECTION('',(0.,0.,1.));
#33621=DIRECTION('center_axis',(0.,0.,1.));
#33622=DIRECTION('ref_axis',(1.,0.,0.));
#33623=DIRECTION('center_axis',(0.,0.,1.));
#33624=DIRECTION('ref_axis',(1.,0.,0.));
#33625=DIRECTION('center_axis',(0.,0.,1.));
#33626=DIRECTION('ref_axis',(1.,0.,0.));
#33627=DIRECTION('center_axis',(0.,0.,1.));
#33628=DIRECTION('ref_axis',(1.,0.,0.));
#33629=DIRECTION('',(0.,0.,1.));
#33630=DIRECTION('center_axis',(0.,0.,1.));
#33631=DIRECTION('ref_axis',(1.,0.,0.));
#33632=DIRECTION('center_axis',(0.,0.,-1.));
#33633=DIRECTION('ref_axis',(1.,0.,0.));
#33634=DIRECTION('',(0.857167300702114,1.04972719113862E-16,0.515038074910052));
#33635=DIRECTION('center_axis',(0.,0.,-1.));
#33636=DIRECTION('ref_axis',(-1.,0.,0.));
#33637=DIRECTION('center_axis',(0.,0.,1.));
#33638=DIRECTION('ref_axis',(1.,0.,0.));
#33639=DIRECTION('center_axis',(0.,0.,1.));
#33640=DIRECTION('ref_axis',(1.,0.,0.));
#33641=DIRECTION('center_axis',(0.,0.,1.));
#33642=DIRECTION('ref_axis',(1.,0.,0.));
#33643=DIRECTION('',(0.707106781186543,8.65956056235488E-17,-0.707106781186552));
#33644=DIRECTION('center_axis',(0.,0.,1.));
#33645=DIRECTION('ref_axis',(1.,0.,0.));
#33646=DIRECTION('center_axis',(0.,0.,1.));
#33647=DIRECTION('ref_axis',(1.,0.,0.));
#33648=DIRECTION('',(0.,0.,-1.));
#33649=DIRECTION('',(0.,0.,-1.));
#33650=DIRECTION('center_axis',(6.12323399573677E-17,0.,1.));
#33651=DIRECTION('ref_axis',(1.,0.,0.));
#33652=DIRECTION('center_axis',(1.22464679914735E-16,-1.,0.));
#33653=DIRECTION('ref_axis',(-1.,-1.22464679914735E-16,0.));
#33654=DIRECTION('axis',(0.,0.,1.));
#33655=DIRECTION('refdir',(1.,0.,0.));
#33656=DIRECTION('center_axis',(0.,-1.,0.));
#33657=DIRECTION('ref_axis',(0.,0.,-1.));
#33658=DIRECTION('center_axis',(0.,1.,0.));
#33659=DIRECTION('ref_axis',(-1.,0.,0.));
#33660=DIRECTION('center_axis',(0.,1.,0.));
#33661=DIRECTION('ref_axis',(-1.,0.,0.));
#33662=DIRECTION('center_axis',(0.,-1.,0.));
#33663=DIRECTION('ref_axis',(-1.,0.,0.));
#33664=DIRECTION('center_axis',(0.,1.,0.));
#33665=DIRECTION('ref_axis',(-0.396879513944558,0.,-0.917870716065793));
#33666=DIRECTION('',(0.,1.,0.));
#33667=DIRECTION('center_axis',(0.,-1.,0.));
#33668=DIRECTION('ref_axis',(-0.396879513944558,0.,-0.917870716065793));
#33669=DIRECTION('',(0.,-1.,0.));
#33670=DIRECTION('center_axis',(0.,1.,0.));
#33671=DIRECTION('ref_axis',(-0.396879513944558,0.,-0.917870716065793));
#33672=DIRECTION('center_axis',(0.,-1.,0.));
#33673=DIRECTION('ref_axis',(-0.396879513944558,0.,0.917870716065793));
#33674=DIRECTION('',(0.,1.,0.));
#33675=DIRECTION('center_axis',(0.,-1.,0.));
#33676=DIRECTION('ref_axis',(-0.396879513944558,0.,0.917870716065793));
#33677=DIRECTION('',(0.,-1.,0.));
#33678=DIRECTION('center_axis',(0.,1.,0.));
#33679=DIRECTION('ref_axis',(-0.396879513944558,0.,0.917870716065793));
#33680=DIRECTION('center_axis',(0.,1.,0.));
#33681=DIRECTION('ref_axis',(0.,0.,1.));
#33682=DIRECTION('center_axis',(0.,-1.,0.));
#33683=DIRECTION('ref_axis',(-1.,0.,0.));
#33684=DIRECTION('center_axis',(0.,-1.,0.));
#33685=DIRECTION('ref_axis',(-1.,0.,0.));
#33686=DIRECTION('center_axis',(0.,1.,0.));
#33687=DIRECTION('ref_axis',(-1.,0.,0.));
#33688=DIRECTION('center_axis',(1.,0.,0.));
#33689=DIRECTION('ref_axis',(0.,1.,0.));
#33690=DIRECTION('',(0.,0.,1.));
#33691=DIRECTION('',(0.,1.,0.));
#33692=DIRECTION('',(0.,0.,1.));
#33693=DIRECTION('center_axis',(0.,1.,0.));
#33694=DIRECTION('ref_axis',(-1.,0.,0.));
#33695=DIRECTION('',(0.,0.,1.));
#33696=DIRECTION('',(1.,0.,0.));
#33697=DIRECTION('',(0.,0.,1.));
#33698=DIRECTION('center_axis',(0.,1.,0.));
#33699=DIRECTION('ref_axis',(0.66778348591556,0.,-0.744355570905776));
#33700=DIRECTION('',(-1.,0.,0.));
#33701=DIRECTION('center_axis',(0.,1.,0.));
#33702=DIRECTION('ref_axis',(1.,0.,0.));
#33703=DIRECTION('center_axis',(0.,1.,0.));
#33704=DIRECTION('ref_axis',(1.,0.,0.));
#33705=DIRECTION('',(0.,1.,0.));
#33706=DIRECTION('',(0.,1.,0.));
#33707=DIRECTION('center_axis',(0.,-1.,0.));
#33708=DIRECTION('ref_axis',(1.,0.,0.));
#33709=DIRECTION('center_axis',(0.,0.,-1.));
#33710=DIRECTION('ref_axis',(-0.70710678118655,0.707106781186545,0.));
#33711=DIRECTION('center_axis',(0.707106781186546,0.,0.707106781186549));
#33712=DIRECTION('ref_axis',(-0.707106781186549,1.96261557335472E-16,0.707106781186546));
#33713=DIRECTION('',(0.,0.,1.));
#33714=DIRECTION('center_axis',(0.70710678118655,0.,-0.707106781186545));
#33715=DIRECTION('ref_axis',(-0.707106781186545,-6.54205191118238E-17,-0.70710678118655));
#33716=DIRECTION('',(0.,0.,-1.));
#33717=DIRECTION('center_axis',(-0.707106781186551,0.,0.707106781186544));
#33718=DIRECTION('ref_axis',(-0.707106781186544,-6.54205191118236E-17,-0.707106781186551));
#33719=DIRECTION('center_axis',(0.,-1.,0.));
#33720=DIRECTION('ref_axis',(-1.,0.,0.));
#33721=DIRECTION('',(-1.,0.,0.));
#33722=DIRECTION('',(0.,0.,-1.));
#33723=DIRECTION('',(1.,0.,0.));
#33724=DIRECTION('',(0.,0.,1.));
#33725=DIRECTION('',(1.,0.,0.));
#33726=DIRECTION('center_axis',(-0.70710678118655,0.,0.707106781186545));
#33727=DIRECTION('ref_axis',(0.707106781186545,0.,0.70710678118655));
#33728=DIRECTION('',(0.,-1.,0.));
#33729=DIRECTION('',(-0.707106781186548,0.,-0.707106781186548));
#33730=DIRECTION('',(0.,1.,0.));
#33731=DIRECTION('center_axis',(-1.,0.,0.));
#33732=DIRECTION('ref_axis',(0.,-1.,0.));
#33733=DIRECTION('',(0.,1.,0.));
#33734=DIRECTION('',(0.,0.,-1.));
#33735=DIRECTION('center_axis',(0.,0.,1.));
#33736=DIRECTION('ref_axis',(-0.70710678118655,-0.707106781186545,0.));
#33737=DIRECTION('center_axis',(0.70710678118655,0.,-0.707106781186545));
#33738=DIRECTION('ref_axis',(-0.707106781186545,6.54205191118238E-17,-0.70710678118655));
#33739=DIRECTION('',(0.,0.,-1.));
#33740=DIRECTION('center_axis',(0.707106781186546,0.,0.707106781186549));
#33741=DIRECTION('ref_axis',(-0.707106781186549,-1.96261557335472E-16,0.707106781186546));
#33742=DIRECTION('center_axis',(-0.707106781186547,0.,0.707106781186548));
#33743=DIRECTION('ref_axis',(-0.707106781186548,6.5420519111824E-17,-0.707106781186547));
#33744=DIRECTION('',(0.,0.,1.));
#33745=DIRECTION('center_axis',(-0.70710678118655,0.,0.707106781186545));
#33746=DIRECTION('ref_axis',(0.707106781186545,0.,0.70710678118655));
#33747=DIRECTION('',(0.,1.,0.));
#33748=DIRECTION('',(-0.707106781186545,0.,-0.70710678118655));
#33749=DIRECTION('',(0.,-1.,0.));
#33750=DIRECTION('center_axis',(0.,1.,0.));
#33751=DIRECTION('ref_axis',(1.,0.,0.));
#33752=DIRECTION('',(-1.,0.,0.));
#33753=DIRECTION('',(0.,0.,-1.));
#33754=DIRECTION('',(-1.,0.,0.));
#33755=DIRECTION('',(0.,0.,-1.));
#33756=DIRECTION('',(1.,0.,0.));
#33757=DIRECTION('center_axis',(-1.,0.,0.));
#33758=DIRECTION('ref_axis',(0.,-0.707106781186545,-0.70710678118655));
#33759=DIRECTION('center_axis',(0.707106781186546,0.,0.707106781186549));
#33760=DIRECTION('ref_axis',(0.70710678118655,6.54205191118238E-17,-0.707106781186546));
#33761=DIRECTION('',(1.,0.,0.));
#33762=DIRECTION('center_axis',(1.,-5.9211894646675E-15,0.));
#33763=DIRECTION('ref_axis',(0.,0.,-1.));
#33764=DIRECTION('center_axis',(-0.40824829046386,-0.40824829046386,-0.816496580927729));
#33765=DIRECTION('ref_axis',(0.577350269189629,0.577350269189626,-0.577350269189622));
#33766=DIRECTION('center_axis',(1.,0.,1.1842378929335E-14));
#33767=DIRECTION('ref_axis',(0.,1.,0.));
#33768=DIRECTION('center_axis',(0.,2.96059473233374E-15,-1.));
#33769=DIRECTION('ref_axis',(1.,0.,0.));
#33770=DIRECTION('center_axis',(0.,1.,0.));
#33771=DIRECTION('ref_axis',(0.,0.,-1.));
#33772=DIRECTION('center_axis',(0.,0.,-1.));
#33773=DIRECTION('ref_axis',(0.707106781186545,0.70710678118655,0.));
#33774=DIRECTION('',(0.,0.,-1.));
#33775=DIRECTION('center_axis',(-0.707106781186548,-2.09345661157836E-15,
-0.707106781186548));
#33776=DIRECTION('ref_axis',(-0.707106781186548,-2.09345661157836E-15,0.707106781186548));
#33777=DIRECTION('center_axis',(-0.408248290463859,-0.816496580927727,0.408248290463866));
#33778=DIRECTION('ref_axis',(0.577350269189622,-0.577350269189625,-0.577350269189631));
#33779=DIRECTION('center_axis',(-2.96059473233375E-15,0.,-1.));
#33780=DIRECTION('ref_axis',(0.,-1.,0.));
#33781=DIRECTION('center_axis',(0.,-1.,2.96059473233375E-15));
#33782=DIRECTION('ref_axis',(1.,0.,0.));
#33783=DIRECTION('center_axis',(-1.,0.,0.));
#33784=DIRECTION('ref_axis',(0.,-0.707106781186548,-0.707106781186547));
#33785=DIRECTION('',(-1.,0.,0.));
#33786=DIRECTION('center_axis',(0.707106781186552,0.707106781186543,-4.18691322315676E-15));
#33787=DIRECTION('ref_axis',(0.707106781186543,-0.707106781186552,4.18691322315681E-15));
#33788=DIRECTION('',(1.,0.,0.));
#33789=DIRECTION('center_axis',(-0.707106781186552,0.707106781186543,0.));
#33790=DIRECTION('ref_axis',(0.707106781186543,0.707106781186552,0.));
#33791=DIRECTION('center_axis',(0.,-1.,0.));
#33792=DIRECTION('ref_axis',(0.707106781186546,0.,-0.707106781186549));
#33793=DIRECTION('',(0.,-1.,0.));
#33794=DIRECTION('',(0.,1.,0.));
#33795=DIRECTION('center_axis',(0.,0.,1.));
#33796=DIRECTION('ref_axis',(0.707106781186545,-0.70710678118655,0.));
#33797=DIRECTION('',(0.,0.,1.));
#33798=DIRECTION('center_axis',(-0.707106781186548,2.09345661157836E-15,
-0.707106781186548));
#33799=DIRECTION('ref_axis',(0.707106781186548,-2.09345661157836E-15,-0.707106781186548));
#33800=DIRECTION('center_axis',(0.,1.,0.));
#33801=DIRECTION('ref_axis',(-0.707106781186544,0.,-0.707106781186551));
#33802=DIRECTION('',(0.,1.,0.));
#33803=DIRECTION('',(0.,-1.,0.));
#33804=DIRECTION('center_axis',(0.707106781186552,0.707106781186543,0.));
#33805=DIRECTION('ref_axis',(0.707106781186543,-0.707106781186552,0.));
#33806=DIRECTION('center_axis',(1.,0.,0.));
#33807=DIRECTION('ref_axis',(0.,-0.707106781186547,-0.707106781186547));
#33808=DIRECTION('',(1.,0.,0.));
#33809=DIRECTION('center_axis',(-1.,0.,0.));
#33810=DIRECTION('ref_axis',(0.,0.,-1.));
#33811=DIRECTION('center_axis',(0.,0.,-1.));
#33812=DIRECTION('ref_axis',(1.,-1.22464679914735E-16,0.));
#33813=DIRECTION('center_axis',(1.,0.,0.));
#33814=DIRECTION('ref_axis',(0.,0.,-1.));
#33815=DIRECTION('center_axis',(0.,0.,1.));
#33816=DIRECTION('ref_axis',(1.,-6.12323399573677E-17,0.));
#33817=DIRECTION('center_axis',(0.,0.,-1.));
#33818=DIRECTION('ref_axis',(1.,-6.12323399573677E-17,0.));
#33819=DIRECTION('center_axis',(-1.,0.,0.));
#33820=DIRECTION('ref_axis',(0.,0.707106781186547,-0.707106781186547));
#33821=DIRECTION('',(-1.,0.,0.));
#33822=DIRECTION('center_axis',(1.,0.,0.));
#33823=DIRECTION('ref_axis',(0.,0.707106781186548,-0.707106781186547));
#33824=DIRECTION('',(1.,0.,0.));
#33825=DIRECTION('',(-1.,0.,0.));
#33826=DIRECTION('center_axis',(0.70710678118655,-0.707106781186545,0.));
#33827=DIRECTION('ref_axis',(-0.707106781186545,-0.70710678118655,0.));
#33828=DIRECTION('center_axis',(0.,-1.,0.));
#33829=DIRECTION('ref_axis',(0.707106781186546,0.,-0.707106781186549));
#33830=DIRECTION('',(0.,1.,0.));
#33831=DIRECTION('',(0.,-1.,0.));
#33832=DIRECTION('center_axis',(1.,0.,0.));
#33833=DIRECTION('ref_axis',(0.,0.707106781186545,-0.70710678118655));
#33834=DIRECTION('',(-1.,0.,0.));
#33835=DIRECTION('center_axis',(0.707106781186546,0.,0.707106781186549));
#33836=DIRECTION('ref_axis',(0.70710678118655,-6.54205191118238E-17,-0.707106781186546));
#33837=DIRECTION('center_axis',(-0.707106781186546,0.,-0.707106781186549));
#33838=DIRECTION('ref_axis',(-0.707106781186549,0.,0.707106781186546));
#33839=DIRECTION('',(0.,-1.,0.));
#33840=DIRECTION('',(-0.707106781186549,0.,0.707106781186546));
#33841=DIRECTION('center_axis',(0.,0.,1.));
#33842=DIRECTION('ref_axis',(1.,0.,0.));
#33843=DIRECTION('',(0.,-1.,0.));
#33844=DIRECTION('center_axis',(0.,0.,1.));
#33845=DIRECTION('ref_axis',(-0.707106781186548,0.707106781186548,0.));
#33846=DIRECTION('',(-1.,0.,0.));
#33847=DIRECTION('center_axis',(0.,0.,1.));
#33848=DIRECTION('ref_axis',(0.707106781186548,0.707106781186548,0.));
#33849=DIRECTION('',(0.,1.,0.));
#33850=DIRECTION('center_axis',(0.,0.,1.));
#33851=DIRECTION('ref_axis',(0.707106781186548,-0.707106781186548,0.));
#33852=DIRECTION('',(1.,0.,0.));
#33853=DIRECTION('center_axis',(0.,0.,1.));
#33854=DIRECTION('ref_axis',(-0.707106781186548,-0.707106781186548,0.));
#33855=DIRECTION('center_axis',(0.,0.,-1.));
#33856=DIRECTION('ref_axis',(1.,0.,0.));
#33857=DIRECTION('center_axis',(0.,0.,-1.));
#33858=DIRECTION('ref_axis',(1.,0.,0.));
#33859=DIRECTION('center_axis',(0.,0.,-1.));
#33860=DIRECTION('ref_axis',(1.,0.,0.));
#33861=DIRECTION('center_axis',(0.,0.,-1.));
#33862=DIRECTION('ref_axis',(1.,0.,0.));
#33863=DIRECTION('center_axis',(0.,0.,1.));
#33864=DIRECTION('ref_axis',(1.,0.,0.));
#33865=DIRECTION('',(0.,-1.,0.));
#33866=DIRECTION('',(-1.,0.,0.));
#33867=DIRECTION('',(0.,1.,0.));
#33868=DIRECTION('',(1.,0.,0.));
#33869=DIRECTION('',(0.,-1.,0.));
#33870=DIRECTION('center_axis',(0.,0.,-1.));
#33871=DIRECTION('ref_axis',(-1.,1.22464679914735E-16,0.));
#33872=DIRECTION('center_axis',(-1.,0.,0.));
#33873=DIRECTION('ref_axis',(0.,-1.,0.));
#33874=DIRECTION('',(0.,0.,1.));
#33875=DIRECTION('center_axis',(0.,1.,0.));
#33876=DIRECTION('ref_axis',(-1.,0.,0.));
#33877=DIRECTION('',(0.,0.,1.));
#33878=DIRECTION('center_axis',(0.,0.,1.));
#33879=DIRECTION('ref_axis',(1.,0.,0.));
#33880=DIRECTION('center_axis',(0.,0.,-1.));
#33881=DIRECTION('ref_axis',(-1.,0.,0.));
#33882=DIRECTION('center_axis',(0.,-1.,0.));
#33883=DIRECTION('ref_axis',(-1.,0.,0.));
#33884=DIRECTION('center_axis',(0.,0.,1.));
#33885=DIRECTION('ref_axis',(-1.,0.,0.));
#33886=DIRECTION('center_axis',(0.,0.,1.));
#33887=DIRECTION('ref_axis',(1.,0.,0.));
#33888=DIRECTION('center_axis',(0.,0.,1.));
#33889=DIRECTION('ref_axis',(1.,0.,0.));
#33890=DIRECTION('',(0.,0.,1.));
#33891=DIRECTION('center_axis',(0.,0.,-1.));
#33892=DIRECTION('ref_axis',(-1.,0.,0.));
#33893=DIRECTION('center_axis',(0.,0.,1.));
#33894=DIRECTION('ref_axis',(1.,0.,0.));
#33895=DIRECTION('center_axis',(0.,0.,1.));
#33896=DIRECTION('ref_axis',(1.,0.,0.));
#33897=DIRECTION('center_axis',(0.,-1.,0.));
#33898=DIRECTION('ref_axis',(-1.,0.,0.));
#33899=DIRECTION('center_axis',(0.,0.,1.));
#33900=DIRECTION('ref_axis',(1.,0.,0.));
#33901=DIRECTION('center_axis',(0.,0.,-1.));
#33902=DIRECTION('ref_axis',(-1.,0.,0.));
#33903=DIRECTION('center_axis',(0.,-1.,0.));
#33904=DIRECTION('ref_axis',(-1.,0.,0.));
#33905=DIRECTION('center_axis',(0.,0.,1.));
#33906=DIRECTION('ref_axis',(-1.,0.,0.));
#33907=DIRECTION('center_axis',(0.,0.,1.));
#33908=DIRECTION('ref_axis',(1.,0.,0.));
#33909=DIRECTION('center_axis',(0.,0.,1.));
#33910=DIRECTION('ref_axis',(1.,0.,0.));
#33911=DIRECTION('',(0.,0.,1.));
#33912=DIRECTION('center_axis',(0.,0.,-1.));
#33913=DIRECTION('ref_axis',(-1.,0.,0.));
#33914=DIRECTION('center_axis',(0.,0.,1.));
#33915=DIRECTION('ref_axis',(1.,0.,0.));
#33916=DIRECTION('center_axis',(0.,0.,1.));
#33917=DIRECTION('ref_axis',(1.,0.,0.));
#33918=DIRECTION('center_axis',(0.,-1.,0.));
#33919=DIRECTION('ref_axis',(-1.,0.,0.));
#33920=DIRECTION('center_axis',(0.,0.,1.));
#33921=DIRECTION('ref_axis',(1.,0.,0.));
#33922=DIRECTION('center_axis',(0.,-1.,0.));
#33923=DIRECTION('ref_axis',(-1.,0.,0.));
#33924=DIRECTION('center_axis',(0.,0.,1.));
#33925=DIRECTION('ref_axis',(1.,0.,0.));
#33926=DIRECTION('center_axis',(0.,0.,1.));
#33927=DIRECTION('ref_axis',(1.,0.,0.));
#33928=DIRECTION('',(0.,0.,1.));
#33929=DIRECTION('center_axis',(0.,0.,1.));
#33930=DIRECTION('ref_axis',(1.,0.,0.));
#33931=DIRECTION('center_axis',(0.,0.,1.));
#33932=DIRECTION('ref_axis',(1.,0.,0.));
#33933=DIRECTION('center_axis',(0.,-1.,0.));
#33934=DIRECTION('ref_axis',(-1.,0.,0.));
#33935=DIRECTION('center_axis',(0.,0.,1.));
#33936=DIRECTION('ref_axis',(1.,0.,0.));
#33937=DIRECTION('center_axis',(0.,0.,1.));
#33938=DIRECTION('ref_axis',(1.,0.,0.));
#33939=DIRECTION('',(0.,0.,1.));
#33940=DIRECTION('center_axis',(0.,0.,1.));
#33941=DIRECTION('ref_axis',(1.,0.,0.));
#33942=DIRECTION('center_axis',(0.,0.,1.));
#33943=DIRECTION('ref_axis',(1.,0.,0.));
#33944=DIRECTION('center_axis',(0.,-2.368475785867E-14,1.));
#33945=DIRECTION('ref_axis',(-1.,0.,0.));
#33946=DIRECTION('center_axis',(0.,1.,0.));
#33947=DIRECTION('ref_axis',(-0.721328943656992,0.,0.692592632824439));
#33948=DIRECTION('center_axis',(-0.69259263282442,0.,-0.72132894365701));
#33949=DIRECTION('ref_axis',(0.,1.,0.));
#33950=DIRECTION('center_axis',(0.,0.,1.));
#33951=DIRECTION('ref_axis',(1.,0.,0.));
#33952=DIRECTION('center_axis',(-0.692592632824435,-2.10153204267973E-14,
-0.721328943656996));
#33953=DIRECTION('ref_axis',(-0.721328943656996,0.,0.692592632824435));
#33954=DIRECTION('center_axis',(0.,-1.,0.));
#33955=DIRECTION('ref_axis',(-1.,0.,0.));
#33956=DIRECTION('center_axis',(-2.368475785867E-14,0.,1.));
#33957=DIRECTION('ref_axis',(0.,-1.,0.));
#33958=DIRECTION('center_axis',(0.,1.,0.));
#33959=DIRECTION('ref_axis',(-0.927720039574705,0.,0.373276744750471));
#33960=DIRECTION('',(0.,-1.,0.));
#33961=DIRECTION('',(0.,1.,0.));
#33962=DIRECTION('center_axis',(0.,0.,-1.));
#33963=DIRECTION('ref_axis',(-0.707106781186552,-0.707106781186543,0.));
#33964=DIRECTION('',(0.,0.,1.));
#33965=DIRECTION('',(0.,0.,-1.));
#33966=DIRECTION('center_axis',(0.,1.,0.));
#33967=DIRECTION('ref_axis',(0.,0.,1.));
#33968=DIRECTION('center_axis',(0.,1.,0.));
#33969=DIRECTION('ref_axis',(0.853668140319692,0.,-0.52081734437624));
#33970=DIRECTION('center_axis',(0.,-1.,0.));
#33971=DIRECTION('ref_axis',(0.853668140319692,0.,-0.52081734437624));
#33972=DIRECTION('center_axis',(0.,-1.,0.));
#33973=DIRECTION('ref_axis',(0.,0.,-1.));
#33974=DIRECTION('center_axis',(0.,1.,0.));
#33975=DIRECTION('ref_axis',(0.853668140319692,0.,-0.52081734437624));
#33976=DIRECTION('center_axis',(0.,-1.,0.));
#33977=DIRECTION('ref_axis',(0.853668140319692,0.,-0.52081734437624));
#33978=DIRECTION('center_axis',(0.,0.,1.));
#33979=DIRECTION('ref_axis',(-0.707106781186552,0.707106781186543,0.));
#33980=DIRECTION('',(0.,0.,1.));
#33981=DIRECTION('',(0.,0.,-1.));
#33982=DIRECTION('center_axis',(0.,1.,0.));
#33983=DIRECTION('ref_axis',(1.,0.,0.));
#33984=DIRECTION('center_axis',(0.,1.,0.));
#33985=DIRECTION('ref_axis',(1.,0.,0.));
#33986=DIRECTION('',(-1.,0.,0.));
#33987=DIRECTION('center_axis',(0.,-1.,0.));
#33988=DIRECTION('ref_axis',(0.999999998065448,0.,6.22021185913536E-5));
#33989=DIRECTION('',(0.,0.,1.));
#33990=DIRECTION('center_axis',(-1.,0.,0.));
#33991=DIRECTION('ref_axis',(0.,0.,1.));
#33992=DIRECTION('',(0.,-1.,0.));
#33993=DIRECTION('',(0.,-1.,0.));
#33994=DIRECTION('',(0.,0.,-1.));
#33995=DIRECTION('',(0.,1.,0.));
#33996=DIRECTION('',(0.,0.,1.));
#33997=DIRECTION('center_axis',(-1.,0.,0.));
#33998=DIRECTION('ref_axis',(0.,0.707106781186573,-0.707106781186522));
#33999=DIRECTION('',(-1.,0.,0.));
#34000=DIRECTION('center_axis',(1.,0.,0.));
#34001=DIRECTION('ref_axis',(0.,0.,-1.));
#34002=DIRECTION('',(1.,0.,0.));
#34003=DIRECTION('center_axis',(0.,-1.,0.));
#34004=DIRECTION('ref_axis',(-0.710342984735764,0.,-0.703855698305189));
#34005=DIRECTION('',(0.,-1.,0.));
#34006=DIRECTION('center_axis',(0.,-1.,0.));
#34007=DIRECTION('ref_axis',(-0.710342984735764,0.,-0.703855698305189));
#34008=DIRECTION('',(0.,1.,0.));
#34009=DIRECTION('center_axis',(0.,-1.,0.));
#34010=DIRECTION('ref_axis',(-0.999957915114768,0.,0.00917431192661418));
#34011=DIRECTION('',(0.,-1.,0.));
#34012=DIRECTION('center_axis',(-0.815256777504774,-0.411367939544186,0.407593921750192));
#34013=DIRECTION('ref_axis',(-0.579099634547059,0.579124006914431,-0.57381094263079));
#34014=DIRECTION('center_axis',(-0.00917431192660542,0.,-0.999957915114768));
#34015=DIRECTION('ref_axis',(-0.999957915114768,0.,0.00917431192660542));
#34016=DIRECTION('center_axis',(0.,1.,0.));
#34017=DIRECTION('ref_axis',(-1.,0.,0.));
#34018=DIRECTION('center_axis',(0.,-1.,0.));
#34019=DIRECTION('ref_axis',(-1.,0.,0.));
#34020=DIRECTION('',(0.,1.,0.));
#34021=DIRECTION('center_axis',(0.,1.,0.));
#34022=DIRECTION('ref_axis',(-1.,0.,0.));
#34023=DIRECTION('',(0.,-1.,0.));
#34024=DIRECTION('center_axis',(0.,1.,0.));
#34025=DIRECTION('ref_axis',(-1.,0.,0.));
#34026=DIRECTION('',(0.,1.,0.));
#34027=DIRECTION('center_axis',(0.,1.,0.));
#34028=DIRECTION('ref_axis',(-1.,0.,0.));
#34029=DIRECTION('',(0.,1.,0.));
#34030=DIRECTION('center_axis',(0.,1.,0.));
#34031=DIRECTION('ref_axis',(1.,0.,0.));
#34032=DIRECTION('center_axis',(0.,-1.,0.));
#34033=DIRECTION('ref_axis',(-1.07657990266682E-16,0.,1.));
#34034=DIRECTION('',(0.,0.,1.));
#34035=DIRECTION('',(-1.,0.,0.));
#34036=DIRECTION('',(0.,0.,1.));
#34037=DIRECTION('center_axis',(0.,1.,0.));
#34038=DIRECTION('ref_axis',(0.,0.,1.));
#34039=DIRECTION('center_axis',(0.,1.,0.));
#34040=DIRECTION('ref_axis',(-1.07657990266682E-16,0.,1.));
#34041=DIRECTION('center_axis',(0.,0.,1.));
#34042=DIRECTION('ref_axis',(1.,0.,0.));
#34043=DIRECTION('center_axis',(0.,1.,0.));
#34044=DIRECTION('ref_axis',(-1.,0.,0.));
#34045=DIRECTION('center_axis',(0.,1.,0.));
#34046=DIRECTION('ref_axis',(-1.,0.,0.));
#34047=DIRECTION('',(0.,1.,0.));
#34048=DIRECTION('center_axis',(0.,-1.,0.));
#34049=DIRECTION('ref_axis',(-1.,0.,0.));
#34050=DIRECTION('',(0.,1.,0.));
#34051=DIRECTION('center_axis',(0.,-1.,0.));
#34052=DIRECTION('ref_axis',(-1.07657990266682E-16,0.,1.));
#34053=DIRECTION('',(0.,-1.,0.));
#34054=DIRECTION('center_axis',(0.,1.,0.));
#34055=DIRECTION('ref_axis',(-1.,0.,0.));
#34056=DIRECTION('',(0.,-1.,0.));
#34057=DIRECTION('center_axis',(0.,1.,0.));
#34058=DIRECTION('ref_axis',(-1.,0.,0.));
#34059=DIRECTION('',(0.,1.,0.));
#34060=DIRECTION('center_axis',(0.,-1.,0.));
#34061=DIRECTION('ref_axis',(-0.710342984735764,0.,-0.703855698305189));
#34062=DIRECTION('',(0.,-1.,0.));
#34063=DIRECTION('center_axis',(0.,1.,0.));
#34064=DIRECTION('ref_axis',(0.,0.,-1.));
#34065=DIRECTION('center_axis',(0.,1.,0.));
#34066=DIRECTION('ref_axis',(-0.710342984735764,0.,-0.703855698305189));
#34067=DIRECTION('',(0.,-1.,0.));
#34068=DIRECTION('center_axis',(1.,0.,0.));
#34069=DIRECTION('ref_axis',(0.,-0.707106781186573,-0.707106781186522));
#34070=DIRECTION('',(-1.,0.,0.));
#34071=DIRECTION('center_axis',(1.,0.,0.));
#34072=DIRECTION('ref_axis',(0.,-1.,0.));
#34073=DIRECTION('',(1.,0.,0.));
#34074=DIRECTION('center_axis',(-0.815256777504774,0.411367939544186,0.407593921750192));
#34075=DIRECTION('ref_axis',(-0.579099634547059,-0.579124006914431,-0.57381094263079));
#34076=DIRECTION('center_axis',(-0.00917431192660542,0.,-0.999957915114768));
#34077=DIRECTION('ref_axis',(-0.999957915114768,0.,0.00917431192660542));
#34078=DIRECTION('center_axis',(0.,-1.,0.));
#34079=DIRECTION('ref_axis',(0.00458720422654698,0.,0.999989478723343));
#34080=DIRECTION('center_axis',(0.,1.,0.));
#34081=DIRECTION('ref_axis',(-1.07657990266682E-16,0.,1.));
#34082=DIRECTION('center_axis',(0.,0.,-1.));
#34083=DIRECTION('ref_axis',(1.,0.,0.));
#34084=DIRECTION('center_axis',(0.,1.,0.));
#34085=DIRECTION('ref_axis',(1.,0.,0.));
#34086=DIRECTION('center_axis',(0.,1.,0.));
#34087=DIRECTION('ref_axis',(-1.,0.,0.));
#34088=DIRECTION('',(0.,0.,-1.));
#34089=DIRECTION('',(1.,0.,0.));
#34090=DIRECTION('',(0.,0.,-1.));
#34091=DIRECTION('center_axis',(0.,1.,0.));
#34092=DIRECTION('ref_axis',(-1.,0.,0.));
#34093=DIRECTION('',(0.,1.,0.));
#34094=DIRECTION('center_axis',(0.,-1.,0.));
#34095=DIRECTION('ref_axis',(-1.,0.,0.));
#34096=DIRECTION('',(0.,1.,0.));
#34097=DIRECTION('center_axis',(0.,-1.,0.));
#34098=DIRECTION('ref_axis',(-1.,0.,0.));
#34099=DIRECTION('',(0.,-1.,0.));
#34100=DIRECTION('center_axis',(0.,-1.,0.));
#34101=DIRECTION('ref_axis',(-1.,0.,0.));
#34102=DIRECTION('',(0.,1.,0.));
#34103=DIRECTION('center_axis',(0.,-1.,0.));
#34104=DIRECTION('ref_axis',(-0.882032681580533,0.,0.471188230565932));
#34105=DIRECTION('',(0.,-1.,0.));
#34106=DIRECTION('center_axis',(1.,0.,0.));
#34107=DIRECTION('ref_axis',(0.,1.,0.));
#34108=DIRECTION('',(0.,0.,1.));
#34109=DIRECTION('',(0.,1.,0.));
#34110=DIRECTION('',(0.,0.,1.));
#34111=DIRECTION('center_axis',(1.,0.,0.));
#34112=DIRECTION('ref_axis',(0.,0.,-1.));
#34113=DIRECTION('center_axis',(-1.,0.,0.));
#34114=DIRECTION('ref_axis',(0.,0.,1.));
#34115=DIRECTION('center_axis',(0.,-1.,-1.22464679914736E-16));
#34116=DIRECTION('ref_axis',(0.,-1.22464679914736E-16,1.));
#34117=DIRECTION('center_axis',(1.,0.,0.));
#34118=DIRECTION('ref_axis',(0.,0.,1.));
#34119=DIRECTION('center_axis',(1.,0.,0.));
#34120=DIRECTION('ref_axis',(0.,0.,1.));
#34121=DIRECTION('center_axis',(-1.,0.,0.));
#34122=DIRECTION('ref_axis',(0.,0.,1.));
#34123=DIRECTION('center_axis',(-1.,0.,0.));
#34124=DIRECTION('ref_axis',(0.,0.,1.));
#34125=DIRECTION('',(0.,1.,0.));
#34126=DIRECTION('',(0.,0.,-1.));
#34127=DIRECTION('',(0.,1.,0.));
#34128=DIRECTION('',(0.,0.,-1.));
#34129=DIRECTION('',(0.,0.,1.));
#34130=DIRECTION('',(0.,1.,0.));
#34131=DIRECTION('',(0.,0.,1.));
#34132=DIRECTION('',(0.,1.,0.));
#34133=DIRECTION('center_axis',(-1.,0.,0.));
#34134=DIRECTION('ref_axis',(0.,0.,1.));
#34135=DIRECTION('center_axis',(-1.,0.,0.));
#34136=DIRECTION('ref_axis',(0.,0.,1.));
#34137=DIRECTION('center_axis',(-1.,0.,0.));
#34138=DIRECTION('ref_axis',(0.,0.,1.));
#34139=DIRECTION('center_axis',(-1.,0.,0.));
#34140=DIRECTION('ref_axis',(0.,0.,1.));
#34141=DIRECTION('center_axis',(-1.,0.,0.));
#34142=DIRECTION('ref_axis',(0.,0.,1.));
#34143=DIRECTION('',(-1.,0.,0.));
#34144=DIRECTION('center_axis',(1.,0.,0.));
#34145=DIRECTION('ref_axis',(0.,0.,-1.));
#34146=DIRECTION('center_axis',(0.,-1.,-1.22464679914736E-16));
#34147=DIRECTION('ref_axis',(0.,-1.22464679914736E-16,1.));
#34148=DIRECTION('center_axis',(1.,0.,0.));
#34149=DIRECTION('ref_axis',(0.,0.,1.));
#34150=DIRECTION('center_axis',(1.,0.,0.));
#34151=DIRECTION('ref_axis',(0.,0.,1.));
#34152=DIRECTION('center_axis',(-1.,0.,0.));
#34153=DIRECTION('ref_axis',(0.,0.,1.));
#34154=DIRECTION('center_axis',(-1.,0.,0.));
#34155=DIRECTION('ref_axis',(0.,0.,1.));
#34156=DIRECTION('',(-1.,0.,0.));
#34157=DIRECTION('center_axis',(1.,0.,0.));
#34158=DIRECTION('ref_axis',(0.,0.,-1.));
#34159=DIRECTION('center_axis',(0.,-1.,-1.22464679914736E-16));
#34160=DIRECTION('ref_axis',(0.,-1.22464679914736E-16,1.));
#34161=DIRECTION('center_axis',(1.,0.,0.));
#34162=DIRECTION('ref_axis',(0.,0.,1.));
#34163=DIRECTION('center_axis',(1.,0.,0.));
#34164=DIRECTION('ref_axis',(0.,0.,1.));
#34165=DIRECTION('center_axis',(-1.,0.,0.));
#34166=DIRECTION('ref_axis',(0.,0.,1.));
#34167=DIRECTION('center_axis',(-1.,0.,0.));
#34168=DIRECTION('ref_axis',(0.,0.,1.));
#34169=DIRECTION('',(-1.,0.,0.));
#34170=DIRECTION('center_axis',(1.,0.,0.));
#34171=DIRECTION('ref_axis',(0.,0.,-1.));
#34172=DIRECTION('center_axis',(0.,-1.,-1.22464679914736E-16));
#34173=DIRECTION('ref_axis',(0.,-1.22464679914736E-16,1.));
#34174=DIRECTION('center_axis',(1.,0.,0.));
#34175=DIRECTION('ref_axis',(0.,0.,1.));
#34176=DIRECTION('center_axis',(1.,0.,0.));
#34177=DIRECTION('ref_axis',(0.,0.,1.));
#34178=DIRECTION('center_axis',(0.,1.,0.));
#34179=DIRECTION('ref_axis',(-2.31525300922612E-5,0.,-0.99999999973198));
#34180=DIRECTION('',(0.,1.,0.));
#34181=DIRECTION('center_axis',(0.,-0.707106781186552,-0.707106781186543));
#34182=DIRECTION('ref_axis',(4.79143098953268E-21,0.707106781186543,-0.707106781186552));
#34183=DIRECTION('',(0.,1.,0.));
#34184=DIRECTION('center_axis',(0.,0.707106781186552,-0.707106781186543));
#34185=DIRECTION('ref_axis',(4.79143098953268E-21,-0.707106781186543,-0.707106781186552));
#34186=DIRECTION('',(0.,1.,0.));
#34187=DIRECTION('center_axis',(-1.,0.,0.));
#34188=DIRECTION('ref_axis',(0.,0.,1.));
#34189=DIRECTION('center_axis',(-1.,0.,0.));
#34190=DIRECTION('ref_axis',(0.,0.,1.));
#34191=DIRECTION('',(-1.,0.,0.));
#34192=DIRECTION('center_axis',(0.,1.,0.));
#34193=DIRECTION('ref_axis',(0.224630175168819,0.,0.974444089932114));
#34194=DIRECTION('center_axis',(0.,-1.,0.));
#34195=DIRECTION('ref_axis',(0.224630175168819,0.,0.974444089932114));
#34196=DIRECTION('',(0.,1.,0.));
#34197=DIRECTION('center_axis',(0.,1.,0.));
#34198=DIRECTION('ref_axis',(0.224630175168819,0.,0.974444089932114));
#34199=DIRECTION('center_axis',(-1.,0.,0.));
#34200=DIRECTION('ref_axis',(0.,-1.,0.));
#34201=DIRECTION('',(0.,0.,1.));
#34202=DIRECTION('',(0.,-1.,0.));
#34203=DIRECTION('',(0.,0.707106781186568,-0.707106781186527));
#34204=DIRECTION('',(0.,0.,1.));
#34205=DIRECTION('',(0.,-1.,0.));
#34206=DIRECTION('',(0.,0.707106781186568,0.707106781186527));
#34207=DIRECTION('',(0.,-1.,0.));
#34208=DIRECTION('',(0.,0.,1.));
#34209=DIRECTION('center_axis',(1.,0.,0.));
#34210=DIRECTION('ref_axis',(0.,0.,1.));
#34211=DIRECTION('center_axis',(1.,0.,0.));
#34212=DIRECTION('ref_axis',(0.,0.,1.));
#34213=DIRECTION('center_axis',(1.,0.,0.));
#34214=DIRECTION('ref_axis',(0.,0.,1.));
#34215=DIRECTION('center_axis',(1.,0.,0.));
#34216=DIRECTION('ref_axis',(0.,0.,1.));
#34217=DIRECTION('center_axis',(0.,0.,1.));
#34218=DIRECTION('ref_axis',(1.,0.,0.));
#34219=DIRECTION('center_axis',(1.22464679914735E-16,-1.,0.));
#34220=DIRECTION('ref_axis',(-1.,-1.22464679914735E-16,0.));
#34221=DIRECTION('center_axis',(0.,0.,1.));
#34222=DIRECTION('ref_axis',(-1.,1.22464679914735E-16,0.));
#34223=DIRECTION('center_axis',(0.,0.,1.));
#34224=DIRECTION('ref_axis',(1.,0.,0.));
#34225=DIRECTION('',(0.,0.,1.));
#34226=DIRECTION('center_axis',(0.,0.,-1.));
#34227=DIRECTION('ref_axis',(1.,0.,0.));
#34228=DIRECTION('center_axis',(0.,0.,-1.));
#34229=DIRECTION('ref_axis',(1.,0.,0.));
#34230=DIRECTION('center_axis',(0.,-1.,0.));
#34231=DIRECTION('ref_axis',(0.,0.,-1.));
#34232=DIRECTION('center_axis',(0.,1.,0.));
#34233=DIRECTION('ref_axis',(0.769575246904488,0.,0.638556136413938));
#34234=DIRECTION('center_axis',(0.,-1.,0.));
#34235=DIRECTION('ref_axis',(0.769575246904488,0.,0.638556136413938));
#34236=DIRECTION('center_axis',(0.,1.,0.));
#34237=DIRECTION('ref_axis',(0.490062423506214,0.,0.8716873413485));
#34238=DIRECTION('',(0.,1.,0.));
#34239=DIRECTION('center_axis',(0.,1.,0.));
#34240=DIRECTION('ref_axis',(0.769575246904488,0.,0.638556136413938));
#34241=DIRECTION('',(0.,-1.,0.));
#34242=DIRECTION('center_axis',(1.,0.,0.));
#34243=DIRECTION('ref_axis',(0.,0.,-1.));
#34244=DIRECTION('',(0.,0.,-1.));
#34245=DIRECTION('',(0.,1.,0.));
#34246=DIRECTION('',(0.,0.,1.));
#34247=DIRECTION('center_axis',(0.,1.,0.));
#34248=DIRECTION('ref_axis',(0.,0.,1.));
#34249=DIRECTION('center_axis',(0.,-1.,0.));
#34250=DIRECTION('ref_axis',(0.769575246904488,0.,0.638556136413938));
#34251=DIRECTION('center_axis',(0.,1.,0.));
#34252=DIRECTION('ref_axis',(1.,0.,0.));
#34253=DIRECTION('',(0.,0.,1.));
#34254=DIRECTION('center_axis',(0.,-1.,0.));
#34255=DIRECTION('ref_axis',(-6.22021185922419E-5,0.,0.999999998065448));
#34256=DIRECTION('',(-1.,0.,0.));
#34257=DIRECTION('center_axis',(1.,0.,0.));
#34258=DIRECTION('ref_axis',(0.,0.,-1.));
#34259=DIRECTION('',(0.,0.,-1.));
#34260=DIRECTION('',(0.,1.,0.));
#34261=DIRECTION('center_axis',(0.,0.,-1.));
#34262=DIRECTION('ref_axis',(-1.,0.,0.));
#34263=DIRECTION('center_axis',(0.,0.,1.));
#34264=DIRECTION('ref_axis',(1.,0.,0.));
#34265=DIRECTION('center_axis',(-1.22464679914735E-16,-1.,0.));
#34266=DIRECTION('ref_axis',(1.,-1.22464679914735E-16,0.));
#34267=DIRECTION('center_axis',(0.,0.,1.));
#34268=DIRECTION('ref_axis',(1.,0.,0.));
#34269=DIRECTION('center_axis',(0.,0.,-1.));
#34270=DIRECTION('ref_axis',(0.,-1.,0.));
#34271=DIRECTION('center_axis',(0.,0.,-1.));
#34272=DIRECTION('ref_axis',(-0.707106781186547,-0.707106781186547,0.));
#34273=DIRECTION('',(-1.,0.,0.));
#34274=DIRECTION('center_axis',(0.,0.,-1.));
#34275=DIRECTION('ref_axis',(0.707106781186547,-0.707106781186547,0.));
#34276=DIRECTION('',(0.,-1.,0.));
#34277=DIRECTION('center_axis',(0.,0.,-1.));
#34278=DIRECTION('ref_axis',(0.707106781186547,0.707106781186547,0.));
#34279=DIRECTION('',(1.,0.,0.));
#34280=DIRECTION('center_axis',(0.,0.,-1.));
#34281=DIRECTION('ref_axis',(-0.707106781186547,0.707106781186547,0.));
#34282=DIRECTION('center_axis',(0.,0.,-1.));
#34283=DIRECTION('ref_axis',(1.,0.,0.));
#34284=DIRECTION('center_axis',(0.,0.,-1.));
#34285=DIRECTION('ref_axis',(1.,0.,0.));
#34286=DIRECTION('center_axis',(0.,0.,-1.));
#34287=DIRECTION('ref_axis',(1.,0.,0.));
#34288=DIRECTION('center_axis',(0.,0.,-1.));
#34289=DIRECTION('ref_axis',(1.,0.,0.));
#34290=DIRECTION('',(0.,-1.,0.));
#34291=DIRECTION('',(-1.,0.,0.));
#34292=DIRECTION('',(0.,-1.,0.));
#34293=DIRECTION('',(-1.,0.,0.));
#34294=DIRECTION('',(0.,1.,0.));
#34295=DIRECTION('',(1.,0.,0.));
#34296=DIRECTION('',(0.,-1.,0.));
#34297=DIRECTION('',(1.,0.,0.));
#34298=DIRECTION('',(0.,-1.,0.));
#34299=DIRECTION('',(1.,0.,0.));
#34300=DIRECTION('',(-1.,0.,0.));
#34301=DIRECTION('center_axis',(0.,1.,0.));
#34302=DIRECTION('ref_axis',(0.66778348591556,0.,-0.744355570905776));
#34303=DIRECTION('center_axis',(0.,-1.,0.));
#34304=DIRECTION('ref_axis',(0.66778348591556,0.,-0.744355570905776));
#34305=DIRECTION('center_axis',(0.,-0.707106781186552,0.707106781186543));
#34306=DIRECTION('ref_axis',(1.96261557335473E-16,-0.707106781186543,-0.707106781186552));
#34307=DIRECTION('center_axis',(0.,0.707106781186552,0.707106781186543));
#34308=DIRECTION('ref_axis',(1.96261557335473E-16,0.707106781186543,-0.707106781186552));
#34309=DIRECTION('center_axis',(-1.,0.,0.));
#34310=DIRECTION('ref_axis',(0.,0.,1.));
#34311=DIRECTION('center_axis',(0.,-1.,1.22464679914736E-16));
#34312=DIRECTION('ref_axis',(0.,-1.22464679914736E-16,-1.));
#34313=DIRECTION('center_axis',(-1.,0.,0.));
#34314=DIRECTION('ref_axis',(0.,0.,1.));
#34315=DIRECTION('center_axis',(0.,-1.,1.22464679914736E-16));
#34316=DIRECTION('ref_axis',(0.,-1.22464679914736E-16,-1.));
#34317=DIRECTION('center_axis',(-1.,0.,0.));
#34318=DIRECTION('ref_axis',(0.,0.,1.));
#34319=DIRECTION('center_axis',(0.,-1.,1.22464679914736E-16));
#34320=DIRECTION('ref_axis',(0.,-1.22464679914736E-16,-1.));
#34321=DIRECTION('center_axis',(-1.,0.,0.));
#34322=DIRECTION('ref_axis',(0.,0.,1.));
#34323=DIRECTION('center_axis',(0.,-1.,1.22464679914736E-16));
#34324=DIRECTION('ref_axis',(0.,-1.22464679914736E-16,-1.));
#34325=DIRECTION('center_axis',(0.,1.,0.));
#34326=DIRECTION('ref_axis',(0.734977615278278,0.,-0.678091369241532));
#34327=DIRECTION('center_axis',(0.,-0.707106781186552,-0.707106781186543));
#34328=DIRECTION('ref_axis',(0.,0.707106781186543,-0.707106781186552));
#34329=DIRECTION('',(0.,-1.,0.));
#34330=DIRECTION('center_axis',(0.,0.707106781186552,-0.707106781186543));
#34331=DIRECTION('ref_axis',(0.,-0.707106781186543,-0.707106781186552));
#34332=DIRECTION('',(0.,1.,0.));
#34333=DIRECTION('',(0.,1.,0.));
#34334=DIRECTION('',(0.,1.,0.));
#34335=DIRECTION('center_axis',(0.,0.,-1.));
#34336=DIRECTION('ref_axis',(0.707106781186543,0.707106781186552,0.));
#34337=DIRECTION('center_axis',(0.,0.,1.));
#34338=DIRECTION('ref_axis',(0.707106781186543,0.707106781186552,0.));
#34339=DIRECTION('',(0.,0.,-1.));
#34340=DIRECTION('center_axis',(0.,0.,-1.));
#34341=DIRECTION('ref_axis',(-1.,0.,0.));
#34342=DIRECTION('',(-0.707106781186543,0.707106781186552,0.));
#34343=DIRECTION('',(1.,0.,0.));
#34344=DIRECTION('',(0.,1.,0.));
#34345=DIRECTION('center_axis',(0.,1.,0.));
#34346=DIRECTION('ref_axis',(0.,0.,-1.));
#34347=DIRECTION('center_axis',(0.,1.,0.));
#34348=DIRECTION('ref_axis',(0.,0.,-1.));
#34349=DIRECTION('center_axis',(-0.0803841899203101,0.,0.996763955011845));
#34350=DIRECTION('ref_axis',(0.996763955011845,0.,0.0803841899203101));
#34351=DIRECTION('',(0.996763955011845,0.,0.0803841899203101));
#34352=DIRECTION('',(0.996211888614194,0.0332777802630094,0.0803396684366286));
#34353=DIRECTION('',(-0.996763955011845,0.,-0.0803841899203101));
#34354=DIRECTION('',(0.996763955011845,0.,0.0803841899203101));
#34355=DIRECTION('',(-0.996211888614194,0.0332777802630094,-0.0803396684366286));
#34356=DIRECTION('',(-0.996763955011845,0.,-0.0803841899203101));
#34357=DIRECTION('center_axis',(1.,0.,0.));
#34358=DIRECTION('ref_axis',(0.,0.,-1.));
#34359=DIRECTION('',(0.,0.,1.));
#34360=DIRECTION('center_axis',(0.,-1.,0.));
#34361=DIRECTION('ref_axis',(0.,0.,-1.));
#34362=DIRECTION('center_axis',(0.,-1.,0.));
#34363=DIRECTION('ref_axis',(-0.742667400108486,0.,0.669660460842733));
#34364=DIRECTION('center_axis',(0.,-1.,0.));
#34365=DIRECTION('ref_axis',(1.,0.,0.));
#34366=DIRECTION('',(1.,0.,0.));
#34367=DIRECTION('center_axis',(0.,1.,0.));
#34368=DIRECTION('ref_axis',(-0.99999999973198,0.,2.31525300940375E-5));
#34369=DIRECTION('center_axis',(0.,1.,0.));
#34370=DIRECTION('ref_axis',(0.,0.,1.));
#34371=DIRECTION('center_axis',(0.,1.,0.));
#34372=DIRECTION('ref_axis',(-0.742667400108486,0.,0.669660460842733));
#34373=DIRECTION('center_axis',(0.,1.,0.));
#34374=DIRECTION('ref_axis',(-1.,0.,0.));
#34375=DIRECTION('center_axis',(0.,-1.,0.));
#34376=DIRECTION('ref_axis',(-0.99999999973198,0.,2.31525300940375E-5));
#34377=DIRECTION('',(-1.,0.,0.));
#34378=DIRECTION('center_axis',(0.,0.,1.));
#34379=DIRECTION('ref_axis',(0.707106781186543,-0.707106781186552,0.));
#34380=DIRECTION('center_axis',(0.,0.,1.));
#34381=DIRECTION('ref_axis',(0.707106781186543,-0.707106781186552,0.));
#34382=DIRECTION('center_axis',(0.,0.,-1.));
#34383=DIRECTION('ref_axis',(-1.,0.,0.));
#34384=DIRECTION('',(0.,1.,0.));
#34385=DIRECTION('',(-1.,0.,0.));
#34386=DIRECTION('',(-0.707106781186552,-0.707106781186543,0.));
#34387=DIRECTION('center_axis',(-1.,0.,0.));
#34388=DIRECTION('ref_axis',(0.,0.,1.));
#34389=DIRECTION('',(0.,0.,1.));
#34390=DIRECTION('center_axis',(0.,0.,-1.));
#34391=DIRECTION('ref_axis',(-1.,0.,0.));
#34392=DIRECTION('',(-1.,0.,0.));
#34393=DIRECTION('center_axis',(0.,1.,0.));
#34394=DIRECTION('ref_axis',(-1.,0.,3.55271367880049E-15));
#34395=DIRECTION('',(0.707106781186541,-0.707106781186554,0.));
#34396=DIRECTION('center_axis',(0.,1.,0.));
#34397=DIRECTION('ref_axis',(-1.,0.,3.55271367880049E-15));
#34398=DIRECTION('center_axis',(0.,1.,0.));
#34399=DIRECTION('ref_axis',(-1.,0.,3.55271367880049E-15));
#34400=DIRECTION('center_axis',(0.,1.,0.));
#34401=DIRECTION('ref_axis',(-1.,0.,3.55271367880049E-15));
#34402=DIRECTION('',(0.,-0.707106781186552,-0.707106781186543));
#34403=DIRECTION('center_axis',(0.,1.,0.));
#34404=DIRECTION('ref_axis',(1.,0.,0.));
#34405=DIRECTION('',(0.,0.,1.));
#34406=DIRECTION('center_axis',(0.,1.,0.));
#34407=DIRECTION('ref_axis',(-2.66453525910037E-15,0.,-1.));
#34408=DIRECTION('',(-1.,0.,0.));
#34409=DIRECTION('center_axis',(0.,-1.,0.));
#34410=DIRECTION('ref_axis',(-8.88178419700126E-16,0.,1.));
#34411=DIRECTION('',(0.,0.,1.));
#34412=DIRECTION('center_axis',(0.,-1.,0.));
#34413=DIRECTION('ref_axis',(1.,0.,0.));
#34414=DIRECTION('',(-1.,0.,0.));
#34415=DIRECTION('center_axis',(0.,-1.,0.));
#34416=DIRECTION('ref_axis',(0.,0.,-1.));
#34417=DIRECTION('center_axis',(0.,1.,0.));
#34418=DIRECTION('ref_axis',(-1.,0.,0.));
#34419=DIRECTION('',(0.,0.,1.));
#34420=DIRECTION('center_axis',(0.,-1.,0.));
#34421=DIRECTION('ref_axis',(1.,0.,0.));
#34422=DIRECTION('',(1.,0.,0.));
#34423=DIRECTION('',(1.,0.,0.));
#34424=DIRECTION('',(0.,0.,-1.));
#34425=DIRECTION('',(-1.,0.,0.));
#34426=DIRECTION('',(0.,0.,1.));
#34427=DIRECTION('center_axis',(0.,-1.,0.));
#34428=DIRECTION('ref_axis',(1.,0.,0.));
#34429=DIRECTION('',(1.,0.,0.));
#34430=DIRECTION('',(0.562642780375869,0.,-0.826700128033685));
#34431=DIRECTION('',(0.,0.,1.));
#34432=DIRECTION('',(1.,0.,0.));
#34433=DIRECTION('',(0.,0.,-1.));
#34434=DIRECTION('',(-1.,0.,0.));
#34435=DIRECTION('',(-0.563462177299479,0.,0.826141861155171));
#34436=DIRECTION('',(0.,0.,-1.));
#34437=DIRECTION('',(-1.,0.,0.));
#34438=DIRECTION('',(0.,0.,1.));
#34439=DIRECTION('',(0.,0.,-1.));
#34440=DIRECTION('',(-1.,0.,0.));
#34441=DIRECTION('',(0.,0.,1.));
#34442=DIRECTION('',(0.,0.,1.));
#34443=DIRECTION('',(1.,0.,0.));
#34444=DIRECTION('center_axis',(0.,1.,0.));
#34445=DIRECTION('ref_axis',(-0.99999999973198,0.,2.31525300940375E-5));
#34446=DIRECTION('center_axis',(0.,-1.,0.));
#34447=DIRECTION('ref_axis',(-0.99999999973198,0.,2.31525300940375E-5));
#34448=DIRECTION('center_axis',(0.,1.,0.));
#34449=DIRECTION('ref_axis',(1.,0.,0.));
#34450=DIRECTION('center_axis',(0.,0.,-1.));
#34451=DIRECTION('ref_axis',(-1.,0.,0.));
#34452=DIRECTION('',(1.,0.,0.));
#34453=DIRECTION('center_axis',(-1.,0.,0.));
#34454=DIRECTION('ref_axis',(0.,0.,1.));
#34455=DIRECTION('',(0.,0.,-1.));
#34456=DIRECTION('center_axis',(0.,1.,0.));
#34457=DIRECTION('ref_axis',(-1.,0.,0.));
#34458=DIRECTION('center_axis',(0.,1.,0.));
#34459=DIRECTION('ref_axis',(-1.,0.,0.));
#34460=DIRECTION('',(0.,1.,0.));
#34461=DIRECTION('center_axis',(0.,-1.,0.));
#34462=DIRECTION('ref_axis',(-1.,0.,0.));
#34463=DIRECTION('center_axis',(0.,-1.,0.));
#34464=DIRECTION('ref_axis',(-1.,0.,0.));
#34465=DIRECTION('center_axis',(0.,-1.,0.));
#34466=DIRECTION('ref_axis',(-1.,0.,0.));
#34467=DIRECTION('',(0.707106781186543,0.707106781186552,0.));
#34468=DIRECTION('center_axis',(0.,1.,0.));
#34469=DIRECTION('ref_axis',(1.,0.,0.));
#34470=DIRECTION('',(1.,0.,0.));
#34471=DIRECTION('center_axis',(0.,1.,0.));
#34472=DIRECTION('ref_axis',(1.,0.,0.));
#34473=DIRECTION('',(0.,0.,-1.));
#34474=DIRECTION('center_axis',(0.,1.,0.));
#34475=DIRECTION('ref_axis',(-8.88178419700126E-16,0.,1.));
#34476=DIRECTION('',(1.,0.,0.));
#34477=DIRECTION('center_axis',(0.,-1.,0.));
#34478=DIRECTION('ref_axis',(-2.66453525910037E-15,0.,-1.));
#34479=DIRECTION('',(0.,0.,-1.));
#34480=DIRECTION('center_axis',(0.,-1.,0.));
#34481=DIRECTION('ref_axis',(-1.,0.,3.55271367880049E-15));
#34482=DIRECTION('center_axis',(0.,-1.,0.));
#34483=DIRECTION('ref_axis',(-1.,0.,3.55271367880049E-15));
#34484=DIRECTION('',(-1.,0.,0.));
#34485=DIRECTION('center_axis',(0.,1.,0.));
#34486=DIRECTION('ref_axis',(1.,0.,0.));
#34487=DIRECTION('',(0.,0.,-1.));
#34488=DIRECTION('center_axis',(0.,1.,0.));
#34489=DIRECTION('ref_axis',(1.,0.,0.));
#34490=DIRECTION('center_axis',(0.,-1.,0.));
#34491=DIRECTION('ref_axis',(-1.,0.,3.55271367880049E-15));
#34492=DIRECTION('',(0.707106781186545,0.70710678118655,0.));
#34493=DIRECTION('center_axis',(0.,1.,0.));
#34494=DIRECTION('ref_axis',(-0.99999999973198,0.,2.31525300940375E-5));
#34495=DIRECTION('center_axis',(0.,-1.,0.));
#34496=DIRECTION('ref_axis',(-0.99999999973198,0.,2.31525300940375E-5));
#34497=DIRECTION('center_axis',(0.,1.,0.));
#34498=DIRECTION('ref_axis',(1.,0.,0.));
#34499=DIRECTION('center_axis',(0.,1.,0.));
#34500=DIRECTION('ref_axis',(-0.99999999973198,0.,2.31525300940375E-5));
#34501=DIRECTION('',(0.,1.,0.));
#34502=DIRECTION('center_axis',(0.,0.707106781186527,0.707106781186568));
#34503=DIRECTION('ref_axis',(3.63166511851617E-17,-0.707106781186568,0.707106781186527));
#34504=DIRECTION('center_axis',(0.,1.,0.));
#34505=DIRECTION('ref_axis',(-0.99999999973198,0.,2.31525300940375E-5));
#34506=DIRECTION('center_axis',(0.,-0.707106781186527,0.707106781186568));
#34507=DIRECTION('ref_axis',(3.63166511851617E-17,0.707106781186568,0.707106781186527));
#34508=DIRECTION('',(0.,1.,0.));
#34509=DIRECTION('center_axis',(0.,1.,0.));
#34510=DIRECTION('ref_axis',(1.,0.,0.));
#34511=DIRECTION('',(-1.,0.,0.));
#34512=DIRECTION('center_axis',(0.,1.,0.));
#34513=DIRECTION('ref_axis',(0.,0.,-1.));
#34514=DIRECTION('',(-1.,0.,0.));
#34515=DIRECTION('center_axis',(0.,1.,0.));
#34516=DIRECTION('ref_axis',(0.,0.,-1.));
#34517=DIRECTION('center_axis',(0.,1.,0.));
#34518=DIRECTION('ref_axis',(1.,0.,0.));
#34519=DIRECTION('',(1.,0.,0.));
#34520=DIRECTION('center_axis',(0.,-1.,0.));
#34521=DIRECTION('ref_axis',(0.,0.,-1.));
#34522=DIRECTION('',(1.,0.,0.));
#34523=DIRECTION('center_axis',(0.,-1.,0.));
#34524=DIRECTION('ref_axis',(0.,0.,-1.));
#34525=DIRECTION('center_axis',(0.,1.,0.));
#34526=DIRECTION('ref_axis',(1.,0.,0.));
#34527=DIRECTION('center_axis',(0.,-1.,0.));
#34528=DIRECTION('ref_axis',(1.,0.,0.));
#34529=DIRECTION('center_axis',(0.,1.,0.));
#34530=DIRECTION('ref_axis',(1.,0.,0.));
#34531=DIRECTION('center_axis',(0.,1.,0.));
#34532=DIRECTION('ref_axis',(1.,0.,0.));
#34533=DIRECTION('center_axis',(0.,1.,0.));
#34534=DIRECTION('ref_axis',(1.,0.,0.));
#34535=DIRECTION('center_axis',(0.,0.707106781186543,-0.707106781186552));
#34536=DIRECTION('ref_axis',(0.,-0.707106781186552,-0.707106781186543));
#34537=DIRECTION('center_axis',(0.,1.,0.));
#34538=DIRECTION('ref_axis',(1.,0.,0.));
#34539=DIRECTION('center_axis',(0.,-1.,0.));
#34540=DIRECTION('ref_axis',(1.,0.,0.));
#34541=DIRECTION('center_axis',(0.,-0.707106781186543,-0.707106781186552));
#34542=DIRECTION('ref_axis',(0.,0.707106781186552,-0.707106781186543));
#34543=DIRECTION('center_axis',(0.,-0.707106781186552,-0.707106781186543));
#34544=DIRECTION('ref_axis',(-1.,0.,0.));
#34545=DIRECTION('',(1.,0.,0.));
#34546=DIRECTION('',(-0.57735026918962,-0.577350269189625,0.577350269189633));
#34547=DIRECTION('center_axis',(0.,-1.,0.));
#34548=DIRECTION('ref_axis',(-2.66453525910037E-15,0.,-1.));
#34549=DIRECTION('',(0.707106781186537,0.707106781186558,0.));
#34550=DIRECTION('',(0.,0.707106781186552,0.707106781186543));
#34551=DIRECTION('center_axis',(0.,-1.,0.));
#34552=DIRECTION('ref_axis',(0.,0.,-1.));
#34553=DIRECTION('center_axis',(0.,0.923879532511286,-0.382683432365092));
#34554=DIRECTION('ref_axis',(5.40315374398936E-15,-0.382683432365092,-0.923879532511286));
#34555=DIRECTION('center_axis',(0.,-1.,0.));
#34556=DIRECTION('ref_axis',(0.,0.,-1.));
#34557=DIRECTION('center_axis',(0.,0.923879532511286,0.382683432365092));
#34558=DIRECTION('ref_axis',(0.,-0.382683432365092,0.923879532511286));
#34559=DIRECTION('center_axis',(0.,-0.923879532511286,-0.382683432365092));
#34560=DIRECTION('ref_axis',(5.40315374398936E-15,-0.382683432365092,0.923879532511286));
#34561=DIRECTION('',(-1.,0.,0.));
#34562=DIRECTION('center_axis',(0.,-0.923879532511286,-0.382683432365092));
#34563=DIRECTION('ref_axis',(1.55829399144591E-15,-0.382683432365092,0.923879532511286));
#34564=DIRECTION('center_axis',(0.,1.,0.));
#34565=DIRECTION('ref_axis',(0.,0.,-1.));
#34566=DIRECTION('center_axis',(0.,-0.707106781186543,-0.707106781186552));
#34567=DIRECTION('ref_axis',(0.,0.707106781186552,-0.707106781186543));
#34568=DIRECTION('center_axis',(0.,1.,0.));
#34569=DIRECTION('ref_axis',(0.,0.,-1.));
#34570=DIRECTION('center_axis',(0.,0.,1.));
#34571=DIRECTION('ref_axis',(1.,0.,0.));
#34572=DIRECTION('',(0.,-1.,0.));
#34573=DIRECTION('',(1.,0.,0.));
#34574=DIRECTION('center_axis',(0.,0.,1.));
#34575=DIRECTION('ref_axis',(1.,0.,0.));
#34576=DIRECTION('',(-1.,0.,0.));
#34577=DIRECTION('',(0.,-1.,0.));
#34578=DIRECTION('',(1.,0.,0.));
#34579=DIRECTION('center_axis',(0.,1.,0.));
#34580=DIRECTION('ref_axis',(-6.22021185922419E-5,0.,0.999999998065448));
#34581=DIRECTION('center_axis',(0.,1.,0.));
#34582=DIRECTION('ref_axis',(-6.22021185922419E-5,0.,0.999999998065448));
#34583=DIRECTION('center_axis',(0.,1.,0.));
#34584=DIRECTION('ref_axis',(-6.22021185922419E-5,0.,0.999999998065448));
#34585=DIRECTION('center_axis',(0.,1.,0.));
#34586=DIRECTION('ref_axis',(1.,0.,0.));
#34587=DIRECTION('center_axis',(0.,0.,-1.));
#34588=DIRECTION('ref_axis',(-1.,0.,0.));
#34589=DIRECTION('',(1.,0.,0.));
#34590=DIRECTION('',(-1.,0.,0.));
#34591=DIRECTION('',(0.,-1.,0.));
#34592=DIRECTION('',(-1.,0.,0.));
#34593=DIRECTION('center_axis',(0.,-1.,0.));
#34594=DIRECTION('ref_axis',(-8.88178419700126E-16,0.,1.));
#34595=DIRECTION('',(0.707106781186552,-0.707106781186543,0.));
#34596=DIRECTION('',(0.,-0.707106781186552,0.707106781186543));
#34597=DIRECTION('center_axis',(0.,1.,0.));
#34598=DIRECTION('ref_axis',(-1.,0.,0.));
#34599=DIRECTION('center_axis',(0.,1.,0.));
#34600=DIRECTION('ref_axis',(-1.,0.,0.));
#34601=DIRECTION('',(0.,1.,0.));
#34602=DIRECTION('center_axis',(0.,-1.,0.));
#34603=DIRECTION('ref_axis',(-1.,0.,0.));
#34604=DIRECTION('center_axis',(1.,0.,0.));
#34605=DIRECTION('ref_axis',(0.,0.,-1.));
#34606=DIRECTION('',(0.,0.,-1.));
#34607=DIRECTION('',(0.,0.,1.));
#34608=DIRECTION('',(0.,-1.,0.));
#34609=DIRECTION('center_axis',(1.,0.,0.));
#34610=DIRECTION('ref_axis',(0.,0.,-1.));
#34611=DIRECTION('',(0.,0.,1.));
#34612=DIRECTION('',(0.,-1.,0.));
#34613=DIRECTION('',(0.,0.,-1.));
#34614=DIRECTION('center_axis',(0.,0.,-1.));
#34615=DIRECTION('ref_axis',(-1.,0.,0.));
#34616=DIRECTION('',(-1.,0.,0.));
#34617=DIRECTION('',(0.,1.,0.));
#34618=DIRECTION('',(1.,0.,0.));
#34619=DIRECTION('center_axis',(0.,0.,-1.));
#34620=DIRECTION('ref_axis',(-1.,0.,0.));
#34621=DIRECTION('',(-1.,0.,0.));
#34622=DIRECTION('',(0.,1.,0.));
#34623=DIRECTION('',(1.,0.,0.));
#34624=DIRECTION('',(0.,1.,0.));
#34625=DIRECTION('center_axis',(0.,0.,-1.));
#34626=DIRECTION('ref_axis',(-1.,0.,0.));
#34627=DIRECTION('',(1.,0.,0.));
#34628=DIRECTION('',(0.,1.,0.));
#34629=DIRECTION('',(-1.,0.,0.));
#34630=DIRECTION('',(0.,1.,0.));
#34631=DIRECTION('center_axis',(0.,1.,0.));
#34632=DIRECTION('ref_axis',(-0.99999999973198,0.,2.31525300940375E-5));
#34633=DIRECTION('center_axis',(0.,1.,0.));
#34634=DIRECTION('ref_axis',(-0.99999999973198,0.,2.31525300940375E-5));
#34635=DIRECTION('center_axis',(0.,1.,0.));
#34636=DIRECTION('ref_axis',(1.,0.,0.));
#34637=DIRECTION('center_axis',(0.,-1.,0.));
#34638=DIRECTION('ref_axis',(0.99999999973198,0.,-2.31525300911954E-5));
#34639=DIRECTION('center_axis',(0.,1.,0.));
#34640=DIRECTION('ref_axis',(-0.99999999973198,0.,2.31525300940375E-5));
#34641=DIRECTION('center_axis',(0.,-1.,0.));
#34642=DIRECTION('ref_axis',(-0.99999999973198,0.,2.31525300940375E-5));
#34643=DIRECTION('center_axis',(0.,1.,0.));
#34644=DIRECTION('ref_axis',(0.99999999973198,0.,-2.31525300911954E-5));
#34645=DIRECTION('',(0.,1.,0.));
#34646=DIRECTION('center_axis',(0.,1.,0.));
#34647=DIRECTION('ref_axis',(0.99999999973198,0.,-2.31525300911954E-5));
#34648=DIRECTION('',(0.,-1.,0.));
#34649=DIRECTION('center_axis',(0.,1.,0.));
#34650=DIRECTION('ref_axis',(1.,0.,0.));
#34651=DIRECTION('center_axis',(0.,-1.,0.));
#34652=DIRECTION('ref_axis',(-1.,0.,3.55271367880049E-15));
#34653=DIRECTION('',(2.09345661157837E-15,0.707106781186552,-0.707106781186543));
#34654=DIRECTION('center_axis',(0.,-0.707106781186527,0.707106781186568));
#34655=DIRECTION('ref_axis',(1.,0.,0.));
#34656=DIRECTION('',(0.577350269189634,0.577350269189639,0.577350269189605));
#34657=DIRECTION('center_axis',(1.,0.,0.));
#34658=DIRECTION('ref_axis',(0.,0.,-1.));
#34659=DIRECTION('',(0.,1.,0.));
#34660=DIRECTION('',(0.,0.,-1.));
#34661=DIRECTION('center_axis',(1.,0.,0.));
#34662=DIRECTION('ref_axis',(0.,0.,-1.));
#34663=DIRECTION('',(0.,0.,1.));
#34664=DIRECTION('',(0.,1.,0.));
#34665=DIRECTION('',(0.,0.,-1.));
#34666=DIRECTION('center_axis',(0.,1.,0.));
#34667=DIRECTION('ref_axis',(0.999999998065448,0.,6.22021185913536E-5));
#34668=DIRECTION('center_axis',(0.,0.707106781186543,-0.707106781186552));
#34669=DIRECTION('ref_axis',(-6.91941690502001E-18,0.707106781186552,0.707106781186543));
#34670=DIRECTION('center_axis',(0.,1.,0.));
#34671=DIRECTION('ref_axis',(0.999999998065448,0.,6.22021185913536E-5));
#34672=DIRECTION('center_axis',(0.,-0.707106781186543,-0.707106781186552));
#34673=DIRECTION('ref_axis',(-6.91941690502001E-18,-0.707106781186552,0.707106781186543));
#34674=DIRECTION('center_axis',(0.,1.,0.));
#34675=DIRECTION('ref_axis',(0.999999998065448,0.,6.22021185913536E-5));
#34676=DIRECTION('center_axis',(0.,1.,0.));
#34677=DIRECTION('ref_axis',(0.490062423506214,0.,0.8716873413485));
#34678=DIRECTION('',(0.,-1.,0.));
#34679=DIRECTION('center_axis',(0.,1.,0.));
#34680=DIRECTION('ref_axis',(1.,0.,0.));
#34681=DIRECTION('',(1.,0.,0.));
#34682=DIRECTION('center_axis',(0.,0.707106781186543,0.707106781186552));
#34683=DIRECTION('ref_axis',(1.,0.,0.));
#34684=DIRECTION('center_axis',(0.,1.,0.));
#34685=DIRECTION('ref_axis',(1.,0.,0.));
#34686=DIRECTION('',(0.707106781186543,0.707106781186552,0.));
#34687=DIRECTION('center_axis',(-1.,0.,0.));
#34688=DIRECTION('ref_axis',(0.,0.,1.));
#34689=DIRECTION('',(0.,0.,1.));
#34690=DIRECTION('',(0.,0.,-1.));
#34691=DIRECTION('center_axis',(1.,0.,0.));
#34692=DIRECTION('ref_axis',(0.,1.22464679914735E-16,1.));
#34693=DIRECTION('',(0.,-1.,0.));
#34694=DIRECTION('',(0.,1.22464679914735E-16,1.));
#34695=DIRECTION('',(0.,-1.,0.));
#34696=DIRECTION('center_axis',(0.,0.,-1.));
#34697=DIRECTION('ref_axis',(1.,5.65920170377317E-32,0.));
#34698=DIRECTION('',(1.,5.65920170377317E-32,0.));
#34699=DIRECTION('',(0.,-1.,0.));
#34700=DIRECTION('center_axis',(-1.,0.,0.));
#34701=DIRECTION('ref_axis',(0.,-1.22464679914735E-16,-1.));
#34702=DIRECTION('',(0.,-1.22464679914735E-16,-1.));
#34703=DIRECTION('',(0.,-1.,0.));
#34704=DIRECTION('',(0.,-1.,0.));
#34705=DIRECTION('',(0.,-1.,0.));
#34706=DIRECTION('center_axis',(-1.,0.,0.));
#34707=DIRECTION('ref_axis',(0.,-1.22464679914737E-16,-1.));
#34708=DIRECTION('',(0.,-1.22464679914737E-16,-1.));
#34709=DIRECTION('',(0.,-1.,0.));
#34710=DIRECTION('',(0.,-1.,0.));
#34711=DIRECTION('',(0.,-1.,0.));
#34712=DIRECTION('center_axis',(0.,0.,1.));
#34713=DIRECTION('ref_axis',(-1.,0.,0.));
#34714=DIRECTION('',(-1.,0.,0.));
#34715=DIRECTION('center_axis',(-5.65920170377317E-32,1.,-1.22464679914735E-16));
#34716=DIRECTION('ref_axis',(1.,5.65920170377317E-32,0.));
#34717=DIRECTION('center_axis',(0.,0.,1.));
#34718=DIRECTION('ref_axis',(-1.,0.,0.));
#34719=DIRECTION('',(0.,-1.,0.));
#34720=DIRECTION('',(-1.,0.,0.));
#34721=DIRECTION('',(0.,-1.,0.));
#34722=DIRECTION('center_axis',(0.826700128033685,0.,0.562642780375869));
#34723=DIRECTION('ref_axis',(-0.562642780375869,1.01241566565116E-16,0.826700128033685));
#34724=DIRECTION('',(-0.562642780375869,1.01241566565116E-16,0.826700128033685));
#34725=DIRECTION('',(0.,-1.,0.));
#34726=DIRECTION('center_axis',(-1.,0.,0.));
#34727=DIRECTION('ref_axis',(0.,-1.22464679914735E-16,-1.));
#34728=DIRECTION('',(0.,-1.22464679914735E-16,-1.));
#34729=DIRECTION('',(0.,-1.,0.));
#34730=DIRECTION('center_axis',(0.,0.,1.));
#34731=DIRECTION('ref_axis',(-1.,-2.73020257228944E-32,0.));
#34732=DIRECTION('',(-1.,-2.73020257228944E-32,0.));
#34733=DIRECTION('',(0.,-1.,0.));
#34734=DIRECTION('center_axis',(1.,0.,0.));
#34735=DIRECTION('ref_axis',(0.,1.22464679914735E-16,1.));
#34736=DIRECTION('',(0.,1.22464679914735E-16,1.));
#34737=DIRECTION('',(0.,-1.,0.));
#34738=DIRECTION('center_axis',(0.,0.,-1.));
#34739=DIRECTION('ref_axis',(1.,0.,0.));
#34740=DIRECTION('',(1.,0.,0.));
#34741=DIRECTION('',(0.,-1.,0.));
#34742=DIRECTION('center_axis',(-0.826141861155171,0.,-0.563462177299479));
#34743=DIRECTION('ref_axis',(0.563462177299479,-1.01173198590532E-16,-0.826141861155171));
#34744=DIRECTION('',(0.563462177299479,-1.01173198590532E-16,-0.826141861155171));
#34745=DIRECTION('',(0.,-1.,0.));
#34746=DIRECTION('center_axis',(1.,0.,0.));
#34747=DIRECTION('ref_axis',(0.,1.22464679914735E-16,1.));
#34748=DIRECTION('',(0.,1.22464679914735E-16,1.));
#34749=DIRECTION('',(0.,-1.,0.));
#34750=DIRECTION('center_axis',(0.,0.,-1.));
#34751=DIRECTION('ref_axis',(1.,0.,0.));
#34752=DIRECTION('',(1.,0.,0.));
#34753=DIRECTION('',(0.,-1.,0.));
#34754=DIRECTION('center_axis',(-1.,0.,0.));
#34755=DIRECTION('ref_axis',(0.,-1.22464679914735E-16,-1.));
#34756=DIRECTION('',(0.,-1.22464679914735E-16,-1.));
#34757=DIRECTION('center_axis',(0.,-1.,0.));
#34758=DIRECTION('ref_axis',(0.,0.,-1.));
#34759=DIRECTION('',(0.,-1.,0.));
#34760=DIRECTION('',(0.,-1.,0.));
#34761=DIRECTION('',(0.,-1.,0.));
#34762=DIRECTION('',(0.,-1.,0.));
#34763=DIRECTION('',(0.,-1.,0.));
#34764=DIRECTION('',(0.,-1.,0.));
#34765=DIRECTION('',(0.,-1.,0.));
#34766=DIRECTION('',(0.,-1.,0.));
#34767=DIRECTION('',(0.,-1.,0.));
#34768=DIRECTION('',(0.,-1.,0.));
#34769=DIRECTION('',(0.,-1.,0.));
#34770=DIRECTION('',(0.,-1.,0.));
#34771=DIRECTION('',(0.,-1.,0.));
#34772=DIRECTION('',(0.,-1.,0.));
#34773=DIRECTION('',(0.,-1.,0.));
#34774=DIRECTION('',(0.,-1.,0.));
#34775=DIRECTION('',(0.,-1.,0.));
#34776=DIRECTION('',(0.,-1.,0.));
#34777=DIRECTION('center_axis',(5.78607751208046E-16,1.,-3.04931545996342E-16));
#34778=DIRECTION('ref_axis',(1.,-5.78607751208046E-16,0.));
#34779=DIRECTION('center_axis',(0.,0.,1.));
#34780=DIRECTION('ref_axis',(-1.,0.,0.));
#34781=DIRECTION('',(0.,-1.,0.));
#34782=DIRECTION('',(-1.,0.,0.));
#34783=DIRECTION('',(0.,-1.,0.));
#34784=DIRECTION('center_axis',(1.,0.,0.));
#34785=DIRECTION('ref_axis',(0.,1.22464679914735E-16,1.));
#34786=DIRECTION('',(0.,1.22464679914735E-16,1.));
#34787=DIRECTION('',(0.,-1.,0.));
#34788=DIRECTION('center_axis',(0.,0.,-1.));
#34789=DIRECTION('ref_axis',(1.,0.,0.));
#34790=DIRECTION('',(1.,0.,0.));
#34791=DIRECTION('',(0.,-1.,0.));
#34792=DIRECTION('center_axis',(-1.,0.,0.));
#34793=DIRECTION('ref_axis',(0.,-1.22464679914735E-16,-1.));
#34794=DIRECTION('',(0.,-1.22464679914735E-16,-1.));
#34795=DIRECTION('center_axis',(0.,-1.,0.));
#34796=DIRECTION('ref_axis',(0.,0.,-1.));
#34797=DIRECTION('center_axis',(0.,0.,-1.));
#34798=DIRECTION('ref_axis',(-1.,0.,0.));
#34799=DIRECTION('center_axis',(0.,0.,1.));
#34800=DIRECTION('ref_axis',(1.,0.,0.));
#34801=DIRECTION('center_axis',(0.,0.,1.));
#34802=DIRECTION('ref_axis',(1.,0.,0.));
#34803=DIRECTION('',(0.,0.,1.));
#34804=DIRECTION('center_axis',(0.,0.,-1.));
#34805=DIRECTION('ref_axis',(-1.,0.,0.));
#34806=DIRECTION('center_axis',(0.,0.,1.));
#34807=DIRECTION('ref_axis',(1.,0.,0.));
#34808=DIRECTION('center_axis',(0.,0.,1.));
#34809=DIRECTION('ref_axis',(1.,0.,0.));
#34810=DIRECTION('',(0.,0.,1.));
#34811=DIRECTION('center_axis',(0.,0.,1.));
#34812=DIRECTION('ref_axis',(1.,0.,0.));
#34813=DIRECTION('',(0.,0.,1.));
#34814=DIRECTION('center_axis',(0.,0.,1.));
#34815=DIRECTION('ref_axis',(1.,0.,0.));
#34816=DIRECTION('',(0.,0.,1.));
#34817=DIRECTION('center_axis',(-1.,0.,0.));
#34818=DIRECTION('ref_axis',(0.,-1.,0.));
#34819=DIRECTION('',(0.,0.,1.));
#34820=DIRECTION('center_axis',(1.,0.,0.));
#34821=DIRECTION('ref_axis',(0.,1.,0.));
#34822=DIRECTION('',(0.,0.,1.));
#34823=DIRECTION('center_axis',(0.,-1.,0.));
#34824=DIRECTION('ref_axis',(1.,0.,0.));
#34825=DIRECTION('center_axis',(0.,0.,-1.));
#34826=DIRECTION('ref_axis',(0.,-1.,0.));
#34827=DIRECTION('center_axis',(-0.707106781186546,0.,-0.707106781186549));
#34828=DIRECTION('ref_axis',(-0.707106781186549,0.,0.707106781186546));
#34829=DIRECTION('',(0.,1.,0.));
#34830=DIRECTION('',(-0.707106781186546,0.,0.707106781186549));
#34831=DIRECTION('center_axis',(-1.,0.,0.));
#34832=DIRECTION('ref_axis',(0.,-1.,0.));
#34833=DIRECTION('',(0.,0.,1.));
#34834=DIRECTION('center_axis',(-0.707106781186555,0.,-0.70710678118654));
#34835=DIRECTION('ref_axis',(-0.70710678118654,0.,0.707106781186555));
#34836=DIRECTION('',(-0.57735026918962,0.577350269189625,0.577350269189633));
#34837=DIRECTION('center_axis',(0.,0.707106781186552,-0.707106781186543));
#34838=DIRECTION('ref_axis',(-1.,0.,0.));
#34839=DIRECTION('',(-1.,0.,0.));
#34840=DIRECTION('center_axis',(0.,-1.,0.));
#34841=DIRECTION('ref_axis',(1.,0.,0.));
#34842=DIRECTION('',(-1.,0.,0.));
#34843=DIRECTION('',(0.,0.,1.));
#34844=DIRECTION('center_axis',(-0.70710678118653,0.,0.707106781186565));
#34845=DIRECTION('ref_axis',(0.707106781186565,0.,0.70710678118653));
#34846=DIRECTION('',(0.,-1.,0.));
#34847=DIRECTION('',(0.577350269189635,-0.577350269189638,0.577350269189604));
#34848=DIRECTION('center_axis',(0.,0.707106781186527,0.707106781186568));
#34849=DIRECTION('ref_axis',(1.,0.,0.));
#34850=DIRECTION('center_axis',(1.,0.,0.));
#34851=DIRECTION('ref_axis',(0.,1.,0.));
#34852=DIRECTION('center_axis',(0.,1.,0.));
#34853=DIRECTION('ref_axis',(1.,0.,0.));
#34854=DIRECTION('center_axis',(0.,1.,0.));
#34855=DIRECTION('ref_axis',(1.,0.,0.));
#34856=DIRECTION('',(0.707106781186548,-0.707106781186548,-8.65956056235493E-17));
#34857=DIRECTION('center_axis',(0.,1.,0.));
#34858=DIRECTION('ref_axis',(1.,0.,0.));
#34859=DIRECTION('center_axis',(0.,-1.,0.));
#34860=DIRECTION('ref_axis',(1.,0.,0.));
#34861=DIRECTION('center_axis',(0.,-1.,0.));
#34862=DIRECTION('ref_axis',(1.,0.,0.));
#34863=DIRECTION('center_axis',(0.,-1.,0.));
#34864=DIRECTION('ref_axis',(1.,0.,0.));
#34865=DIRECTION('',(0.707106781186548,0.707106781186548,8.65956056235493E-17));
#34866=DIRECTION('center_axis',(0.,1.,0.));
#34867=DIRECTION('ref_axis',(1.,0.,0.));
#34868=DIRECTION('center_axis',(0.,1.,0.));
#34869=DIRECTION('ref_axis',(1.,0.,0.));
#34870=DIRECTION('center_axis',(0.,1.,0.));
#34871=DIRECTION('ref_axis',(1.,0.,0.));
#34872=DIRECTION('',(0.707106781186548,-0.707106781186548,-8.65956056235493E-17));
#34873=DIRECTION('center_axis',(0.,1.,0.));
#34874=DIRECTION('ref_axis',(1.,0.,0.));
#34875=DIRECTION('center_axis',(0.,1.,0.));
#34876=DIRECTION('ref_axis',(1.,0.,0.));
#34877=DIRECTION('',(0.,-1.,0.));
#34878=DIRECTION('center_axis',(0.,-1.,0.));
#34879=DIRECTION('ref_axis',(1.,0.,0.));
#34880=DIRECTION('center_axis',(0.,1.,0.));
#34881=DIRECTION('ref_axis',(1.,0.,0.));
#34882=DIRECTION('center_axis',(0.,1.,0.));
#34883=DIRECTION('ref_axis',(1.,0.,0.));
#34884=DIRECTION('',(-0.707106781186548,0.707106781186548,-8.65956056235493E-17));
#34885=DIRECTION('center_axis',(0.,-1.,0.));
#34886=DIRECTION('ref_axis',(1.,0.,0.));
#34887=DIRECTION('',(0.707106781186548,0.707106781186548,8.65956056235493E-17));
#34888=DIRECTION('center_axis',(0.,-1.,0.));
#34889=DIRECTION('ref_axis',(1.,0.,0.));
#34890=DIRECTION('center_axis',(0.,1.,0.));
#34891=DIRECTION('ref_axis',(1.,0.,0.));
#34892=DIRECTION('center_axis',(0.,1.,0.));
#34893=DIRECTION('ref_axis',(1.,0.,0.));
#34894=DIRECTION('',(0.,-1.,0.));
#34895=DIRECTION('center_axis',(0.,-1.,0.));
#34896=DIRECTION('ref_axis',(1.,0.,0.));
#34897=DIRECTION('',(-0.707106781186548,-0.707106781186548,8.65956056235493E-17));
#34898=DIRECTION('center_axis',(0.,-0.923879532511286,0.382683432365092));
#34899=DIRECTION('ref_axis',(0.,-0.382683432365092,-0.923879532511286));
#34900=DIRECTION('center_axis',(0.,0.923879532511286,-0.382683432365092));
#34901=DIRECTION('ref_axis',(1.24663519315673E-14,0.382683432365092,0.923879532511286));
#34902=DIRECTION('',(1.,0.,0.));
#34903=DIRECTION('center_axis',(0.,1.,0.));
#34904=DIRECTION('ref_axis',(-1.,0.,0.));
#34905=DIRECTION('',(0.707106781186543,-0.707106781186552,0.));
#34906=DIRECTION('center_axis',(-0.707106781186552,-0.707106781186543,0.));
#34907=DIRECTION('ref_axis',(0.,0.,1.));
#34908=DIRECTION('',(0.707106781186543,-0.707106781186552,0.));
#34909=DIRECTION('center_axis',(0.,-1.,0.));
#34910=DIRECTION('ref_axis',(1.,0.,0.));
#34911=DIRECTION('',(0.,-0.707106781186552,-0.707106781186543));
#34912=DIRECTION('center_axis',(0.,1.,0.));
#34913=DIRECTION('ref_axis',(1.,0.,0.));
#34914=DIRECTION('center_axis',(0.,-0.707106781186543,0.707106781186552));
#34915=DIRECTION('ref_axis',(1.,0.,0.));
#34916=DIRECTION('center_axis',(-0.70710678118655,-0.707106781186545,0.));
#34917=DIRECTION('ref_axis',(0.,0.,1.));
#34918=DIRECTION('',(0.707106781186545,-0.70710678118655,0.));
#34919=DIRECTION('center_axis',(0.,1.,0.));
#34920=DIRECTION('ref_axis',(-2.66453525910037E-15,0.,-1.));
#34921=DIRECTION('',(2.09345661157837E-15,-0.707106781186552,0.707106781186543));
#34922=DIRECTION('center_axis',(0.,-0.707106781186543,-0.707106781186552));
#34923=DIRECTION('ref_axis',(-1.,0.,0.));
#34924=DIRECTION('center_axis',(-0.707106781186552,-0.707106781186543,0.));
#34925=DIRECTION('ref_axis',(0.,0.,1.));
#34926=DIRECTION('',(0.707106781186543,-0.707106781186552,0.));
#34927=DIRECTION('center_axis',(0.,-1.,0.));
#34928=DIRECTION('ref_axis',(1.,0.,0.));
#34929=DIRECTION('center_axis',(0.,1.,0.));
#34930=DIRECTION('ref_axis',(1.,0.,0.));
#34931=DIRECTION('center_axis',(0.,-1.,0.));
#34932=DIRECTION('ref_axis',(1.,0.,0.));
#34933=DIRECTION('center_axis',(0.,1.,0.));
#34934=DIRECTION('ref_axis',(0.,0.,-1.));
#34935=DIRECTION('center_axis',(0.,0.707106781186543,-0.707106781186552));
#34936=DIRECTION('ref_axis',(0.,-0.707106781186552,-0.707106781186543));
#34937=DIRECTION('center_axis',(-0.707106781186552,0.707106781186543,0.));
#34938=DIRECTION('ref_axis',(0.,0.,1.));
#34939=DIRECTION('',(0.707106781186543,0.707106781186552,0.));
#34940=DIRECTION('center_axis',(0.,1.,0.));
#34941=DIRECTION('ref_axis',(-8.88178419700126E-16,0.,1.));
#34942=DIRECTION('',(0.,0.707106781186552,0.707106781186543));
#34943=DIRECTION('center_axis',(0.,0.707106781186543,-0.707106781186552));
#34944=DIRECTION('ref_axis',(-1.,0.,0.));
#34945=DIRECTION('center_axis',(-0.70710678118655,0.707106781186545,0.));
#34946=DIRECTION('ref_axis',(0.,0.,1.));
#34947=DIRECTION('center_axis',(0.,0.707106781186543,0.707106781186552));
#34948=DIRECTION('ref_axis',(1.,0.,0.));
#34949=DIRECTION('',(0.,0.707106781186552,-0.707106781186543));
#34950=DIRECTION('center_axis',(0.,1.,0.));
#34951=DIRECTION('ref_axis',(1.,0.,0.));
#34952=DIRECTION('',(0.707106781186543,0.707106781186552,0.));
#34953=DIRECTION('center_axis',(-0.707106781186552,0.707106781186543,0.));
#34954=DIRECTION('ref_axis',(0.,0.,1.));
#34955=DIRECTION('center_axis',(0.707106781186543,0.,-0.707106781186553));
#34956=DIRECTION('ref_axis',(-0.707106781186553,0.,-0.707106781186543));
#34957=DIRECTION('',(0.707106781186553,0.,0.707106781186543));
#34958=DIRECTION('',(0.,-1.,0.));
#34959=DIRECTION('',(-0.707106781186553,0.,-0.707106781186543));
#34960=DIRECTION('center_axis',(0.,0.,1.));
#34961=DIRECTION('ref_axis',(0.707106781186548,0.707106781186548,0.));
#34962=DIRECTION('',(0.,0.707106781186553,0.707106781186543));
#34963=DIRECTION('center_axis',(0.,0.,-1.));
#34964=DIRECTION('ref_axis',(0.707106781186547,0.707106781186547,0.));
#34965=DIRECTION('center_axis',(0.,0.707106781186549,-0.707106781186546));
#34966=DIRECTION('ref_axis',(-1.,0.,0.));
#34967=DIRECTION('',(0.,0.707106781186546,0.707106781186549));
#34968=DIRECTION('',(1.,0.,0.));
#34969=DIRECTION('center_axis',(0.,0.,1.));
#34970=DIRECTION('ref_axis',(-0.707106781186548,0.707106781186548,0.));
#34971=DIRECTION('center_axis',(0.,0.,-1.));
#34972=DIRECTION('ref_axis',(-0.707106781186547,0.707106781186547,0.));
#34973=DIRECTION('center_axis',(0.,0.,1.));
#34974=DIRECTION('ref_axis',(-0.707106781186548,-0.707106781186548,0.));
#34975=DIRECTION('',(0.,-0.707106781186553,0.707106781186543));
#34976=DIRECTION('center_axis',(0.,0.,-1.));
#34977=DIRECTION('ref_axis',(-0.707106781186547,-0.707106781186547,0.));
#34978=DIRECTION('center_axis',(0.,-0.707106781186549,-0.707106781186546));
#34979=DIRECTION('ref_axis',(-1.,0.,0.));
#34980=DIRECTION('',(0.,-0.707106781186546,0.707106781186549));
#34981=DIRECTION('',(-1.,0.,0.));
#34982=DIRECTION('center_axis',(0.,0.,1.));
#34983=DIRECTION('ref_axis',(0.707106781186548,-0.707106781186548,0.));
#34984=DIRECTION('center_axis',(0.,0.,-1.));
#34985=DIRECTION('ref_axis',(0.707106781186547,-0.707106781186547,0.));
#34986=DIRECTION('center_axis',(0.,0.,1.));
#34987=DIRECTION('ref_axis',(-0.707106781186547,-0.707106781186547,0.));
#34988=DIRECTION('',(0.,0.,1.));
#34989=DIRECTION('center_axis',(0.,0.,1.));
#34990=DIRECTION('ref_axis',(-0.707106781186547,-0.707106781186547,0.));
#34991=DIRECTION('center_axis',(0.,-1.,0.));
#34992=DIRECTION('ref_axis',(1.,0.,0.));
#34993=DIRECTION('',(0.,0.,-1.));
#34994=DIRECTION('',(1.,0.,0.));
#34995=DIRECTION('center_axis',(0.,0.,1.));
#34996=DIRECTION('ref_axis',(0.707106781186547,-0.707106781186547,0.));
#34997=DIRECTION('',(0.,0.,1.));
#34998=DIRECTION('center_axis',(0.,0.,1.));
#34999=DIRECTION('ref_axis',(0.707106781186547,-0.707106781186547,0.));
#35000=DIRECTION('center_axis',(1.,0.,0.));
#35001=DIRECTION('ref_axis',(0.,1.,0.));
#35002=DIRECTION('',(0.,0.,-1.));
#35003=DIRECTION('',(0.,1.,0.));
#35004=DIRECTION('center_axis',(0.,-0.707106781186543,0.707106781186552));
#35005=DIRECTION('ref_axis',(1.,0.,0.));
#35006=DIRECTION('center_axis',(0.,0.,-1.));
#35007=DIRECTION('ref_axis',(-0.707106781186547,-0.707106781186547,0.));
#35008=DIRECTION('',(0.,0.707106781186543,0.707106781186552));
#35009=DIRECTION('center_axis',(0.,0.,-1.));
#35010=DIRECTION('ref_axis',(-0.707106781186547,0.707106781186547,0.));
#35011=DIRECTION('',(0.,0.707106781186543,-0.707106781186552));
#35012=DIRECTION('center_axis',(0.,0.,1.));
#35013=DIRECTION('ref_axis',(-0.707106781186547,0.707106781186547,0.));
#35014=DIRECTION('center_axis',(0.,0.707106781186548,0.707106781186548));
#35015=DIRECTION('ref_axis',(1.,0.,0.));
#35016=DIRECTION('',(0.,0.707106781186548,-0.707106781186548));
#35017=DIRECTION('',(-1.,0.,0.));
#35018=DIRECTION('center_axis',(0.,0.,-1.));
#35019=DIRECTION('ref_axis',(0.707106781186548,0.707106781186548,0.));
#35020=DIRECTION('',(0.70710678118656,0.,-0.707106781186535));
#35021=DIRECTION('center_axis',(0.,0.,1.));
#35022=DIRECTION('ref_axis',(0.707106781186547,0.707106781186547,0.));
#35023=DIRECTION('center_axis',(0.707106781186552,0.,0.707106781186543));
#35024=DIRECTION('ref_axis',(0.707106781186543,0.,-0.707106781186552));
#35025=DIRECTION('',(0.707106781186543,0.,-0.707106781186552));
#35026=DIRECTION('center_axis',(0.,0.,-1.));
#35027=DIRECTION('ref_axis',(0.707106781186548,-0.707106781186548,0.));
#35028=DIRECTION('',(0.,-0.707106781186552,-0.707106781186543));
#35029=DIRECTION('center_axis',(0.,-0.707106781186548,0.707106781186548));
#35030=DIRECTION('ref_axis',(1.,0.,0.));
#35031=DIRECTION('center_axis',(0.,0.,1.));
#35032=DIRECTION('ref_axis',(0.707106781186547,0.707106781186547,0.));
#35033=DIRECTION('',(0.,0.,1.));
#35034=DIRECTION('center_axis',(0.,0.,1.));
#35035=DIRECTION('ref_axis',(-0.707106781186547,0.707106781186547,0.));
#35036=DIRECTION('',(0.,0.,-1.));
#35037=DIRECTION('center_axis',(0.,1.,0.));
#35038=DIRECTION('ref_axis',(-1.,0.,0.));
#35039=DIRECTION('axis',(0.,0.,1.));
#35040=DIRECTION('refdir',(1.,0.,0.));
#35041=DIRECTION('center_axis',(0.,0.,1.));
#35042=DIRECTION('ref_axis',(1.,0.,0.));
#35043=DIRECTION('',(0.,0.,-1.));
#35044=DIRECTION('center_axis',(0.,0.,1.));
#35045=DIRECTION('ref_axis',(1.,0.,0.));
#35046=DIRECTION('center_axis',(0.,0.,1.));
#35047=DIRECTION('ref_axis',(1.,0.,0.));
#35048=DIRECTION('',(0.,0.,-1.));
#35049=DIRECTION('center_axis',(0.,0.,1.));
#35050=DIRECTION('ref_axis',(1.,0.,0.));
#35051=DIRECTION('',(0.,0.,-1.));
#35052=DIRECTION('center_axis',(0.,0.,1.));
#35053=DIRECTION('ref_axis',(1.,0.,0.));
#35054=DIRECTION('',(0.,0.,-1.));
#35055=DIRECTION('center_axis',(0.,0.,1.));
#35056=DIRECTION('ref_axis',(1.,0.,0.));
#35057=DIRECTION('',(0.,0.,-1.));
#35058=DIRECTION('center_axis',(0.,0.,1.));
#35059=DIRECTION('ref_axis',(1.,0.,0.));
#35060=DIRECTION('',(0.,0.,-1.));
#35061=DIRECTION('center_axis',(0.,0.,1.));
#35062=DIRECTION('ref_axis',(1.,0.,0.));
#35063=DIRECTION('',(0.,0.,-1.));
#35064=DIRECTION('center_axis',(0.,0.,1.));
#35065=DIRECTION('ref_axis',(1.,0.,0.));
#35066=DIRECTION('',(0.,0.,-1.));
#35067=DIRECTION('center_axis',(0.,0.,1.));
#35068=DIRECTION('ref_axis',(1.,0.,0.));
#35069=DIRECTION('',(0.,0.,-1.));
#35070=DIRECTION('center_axis',(0.,0.,1.));
#35071=DIRECTION('ref_axis',(1.,0.,0.));
#35072=DIRECTION('',(0.,0.,-1.));
#35073=DIRECTION('center_axis',(0.,0.,1.));
#35074=DIRECTION('ref_axis',(1.,0.,0.));
#35075=DIRECTION('',(0.,0.,-1.));
#35076=DIRECTION('center_axis',(0.,0.,1.));
#35077=DIRECTION('ref_axis',(1.,0.,0.));
#35078=DIRECTION('',(0.,0.,-1.));
#35079=DIRECTION('center_axis',(0.,0.,1.));
#35080=DIRECTION('ref_axis',(1.,0.,0.));
#35081=DIRECTION('',(0.,0.,-1.));
#35082=DIRECTION('center_axis',(0.,0.,1.));
#35083=DIRECTION('ref_axis',(1.,0.,0.));
#35084=DIRECTION('',(0.,0.,-1.));
#35085=DIRECTION('center_axis',(0.,0.,1.));
#35086=DIRECTION('ref_axis',(1.,0.,0.));
#35087=DIRECTION('',(0.,0.,-1.));
#35088=DIRECTION('center_axis',(0.,0.,1.));
#35089=DIRECTION('ref_axis',(1.,0.,0.));
#35090=DIRECTION('center_axis',(0.,0.,1.));
#35091=DIRECTION('ref_axis',(0.288300159963205,-0.957540086766706,0.));
#35092=DIRECTION('',(0.,0.,1.));
#35093=DIRECTION('center_axis',(0.,0.,1.));
#35094=DIRECTION('ref_axis',(1.,9.16593808558309E-14,0.));
#35095=DIRECTION('center_axis',(0.,0.,1.));
#35096=DIRECTION('ref_axis',(1.,9.16593808558309E-14,0.));
#35097=DIRECTION('',(0.,0.,1.));
#35098=DIRECTION('center_axis',(0.,0.,1.));
#35099=DIRECTION('ref_axis',(1.,9.16593808558309E-14,0.));
#35100=DIRECTION('',(0.,0.,1.));
#35101=DIRECTION('center_axis',(0.,0.,1.));
#35102=DIRECTION('ref_axis',(1.,9.16593808558309E-14,0.));
#35103=DIRECTION('',(0.,0.,1.));
#35104=DIRECTION('center_axis',(0.,0.,1.));
#35105=DIRECTION('ref_axis',(1.,9.16593808558309E-14,0.));
#35106=DIRECTION('',(0.,0.,1.));
#35107=DIRECTION('center_axis',(0.,0.,1.));
#35108=DIRECTION('ref_axis',(1.,9.16593808558309E-14,0.));
#35109=DIRECTION('',(0.,0.,1.));
#35110=DIRECTION('center_axis',(0.,0.,1.));
#35111=DIRECTION('ref_axis',(1.,9.16593808558309E-14,0.));
#35112=DIRECTION('',(0.,0.,1.));
#35113=DIRECTION('center_axis',(0.,0.,1.));
#35114=DIRECTION('ref_axis',(1.,9.16593808558309E-14,0.));
#35115=DIRECTION('',(0.,0.,1.));
#35116=DIRECTION('center_axis',(0.,0.,1.));
#35117=DIRECTION('ref_axis',(1.,9.16593808558309E-14,0.));
#35118=DIRECTION('',(0.,0.,1.));
#35119=DIRECTION('center_axis',(0.,0.,1.));
#35120=DIRECTION('ref_axis',(1.,9.16593808558309E-14,0.));
#35121=DIRECTION('',(0.,0.,1.));
#35122=DIRECTION('center_axis',(0.,0.,1.));
#35123=DIRECTION('ref_axis',(1.,9.16593808558309E-14,0.));
#35124=DIRECTION('',(0.,0.,1.));
#35125=DIRECTION('center_axis',(0.,0.,1.));
#35126=DIRECTION('ref_axis',(1.,9.16593808558309E-14,0.));
#35127=DIRECTION('',(0.,0.,1.));
#35128=DIRECTION('center_axis',(0.,0.,1.));
#35129=DIRECTION('ref_axis',(1.,9.16593808558309E-14,0.));
#35130=DIRECTION('',(0.,0.,1.));
#35131=DIRECTION('center_axis',(0.,0.,1.));
#35132=DIRECTION('ref_axis',(1.,9.16593808558309E-14,0.));
#35133=DIRECTION('',(0.,0.,1.));
#35134=DIRECTION('',(0.,0.,-1.));
#35135=DIRECTION('',(0.,0.,-1.));
#35136=DIRECTION('',(0.,0.,-1.));
#35137=DIRECTION('',(0.,0.,-1.));
#35138=DIRECTION('',(0.,0.,-1.));
#35139=DIRECTION('',(0.,0.,-1.));
#35140=DIRECTION('',(0.,0.,-1.));
#35141=DIRECTION('',(0.,0.,-1.));
#35142=DIRECTION('',(0.,0.,-1.));
#35143=DIRECTION('',(0.,0.,-1.));
#35144=DIRECTION('',(0.,0.,-1.));
#35145=DIRECTION('',(0.,0.,-1.));
#35146=DIRECTION('',(0.,0.,-1.));
#35147=DIRECTION('',(0.,0.,-1.));
#35148=DIRECTION('',(0.,0.,-1.));
#35149=DIRECTION('',(0.,0.,-1.));
#35150=DIRECTION('',(0.,0.,-1.));
#35151=DIRECTION('',(0.,0.,-1.));
#35152=DIRECTION('',(0.,0.,-1.));
#35153=DIRECTION('',(0.,0.,-1.));
#35154=DIRECTION('',(0.,0.,-1.));
#35155=DIRECTION('',(0.,0.,-1.));
#35156=DIRECTION('',(0.,0.,-1.));
#35157=DIRECTION('',(0.,0.,-1.));
#35158=DIRECTION('',(0.,0.,-1.));
#35159=DIRECTION('',(0.,0.,-1.));
#35160=DIRECTION('',(0.,0.,-1.));
#35161=DIRECTION('',(0.,0.,-1.));
#35162=DIRECTION('',(0.,0.,-1.));
#35163=DIRECTION('',(0.,0.,-1.));
#35164=DIRECTION('',(0.,0.,-1.));
#35165=DIRECTION('',(0.,0.,-1.));
#35166=DIRECTION('',(0.,0.,-1.));
#35167=DIRECTION('center_axis',(0.,0.,1.));
#35168=DIRECTION('ref_axis',(1.,0.,0.));
#35169=DIRECTION('center_axis',(0.,1.,0.));
#35170=DIRECTION('ref_axis',(1.,0.,0.));
#35171=DIRECTION('',(1.,0.,0.));
#35172=DIRECTION('',(0.,0.,-1.));
#35173=DIRECTION('',(1.,0.,0.));
#35174=DIRECTION('',(0.,0.,-1.));
#35175=DIRECTION('center_axis',(-1.,0.,0.));
#35176=DIRECTION('ref_axis',(0.,1.,0.));
#35177=DIRECTION('',(0.,1.,0.));
#35178=DIRECTION('',(0.,0.,-1.));
#35179=DIRECTION('',(0.,1.,0.));
#35180=DIRECTION('center_axis',(0.,-1.,0.));
#35181=DIRECTION('ref_axis',(-1.,0.,0.));
#35182=DIRECTION('',(-1.,0.,0.));
#35183=DIRECTION('',(0.,0.,-1.));
#35184=DIRECTION('',(-1.,0.,0.));
#35185=DIRECTION('center_axis',(1.,0.,0.));
#35186=DIRECTION('ref_axis',(0.,-1.,0.));
#35187=DIRECTION('',(0.,-1.,0.));
#35188=DIRECTION('',(0.,-1.,0.));
#35189=DIRECTION('center_axis',(0.,0.,-1.));
#35190=DIRECTION('ref_axis',(-1.,0.,0.));
#35191=DIRECTION('',(0.,0.,-1.));
#35192=DIRECTION('',(0.,0.,-1.));
#35193=DIRECTION('',(0.,0.,-1.));
#35194=DIRECTION('',(0.,0.,-1.));
#35195=DIRECTION('',(0.,0.,-1.));
#35196=DIRECTION('',(0.,0.,-1.));
#35197=DIRECTION('',(0.,0.,-1.));
#35198=DIRECTION('',(0.,0.,-1.));
#35199=DIRECTION('',(0.,0.,-1.));
#35200=DIRECTION('',(0.,0.,-1.));
#35201=DIRECTION('',(0.,0.,-1.));
#35202=DIRECTION('',(0.,0.,-1.));
#35203=DIRECTION('',(0.,0.,-1.));
#35204=DIRECTION('',(0.,0.,-1.));
#35205=DIRECTION('',(0.,0.,-1.));
#35206=DIRECTION('',(0.,0.,-1.));
#35207=DIRECTION('',(0.,0.,-1.));
#35208=DIRECTION('',(0.,0.,-1.));
#35209=DIRECTION('',(0.,0.,-1.));
#35210=DIRECTION('',(0.,0.,-1.));
#35211=DIRECTION('',(0.,0.,-1.));
#35212=DIRECTION('',(0.,0.,-1.));
#35213=DIRECTION('',(0.,0.,-1.));
#35214=DIRECTION('',(0.,0.,-1.));
#35215=DIRECTION('',(0.,0.,-1.));
#35216=DIRECTION('',(0.,0.,-1.));
#35217=DIRECTION('',(0.,0.,-1.));
#35218=DIRECTION('',(0.,0.,-1.));
#35219=DIRECTION('',(0.,0.,-1.));
#35220=DIRECTION('',(0.,0.,-1.));
#35221=DIRECTION('',(0.,0.,-1.));
#35222=DIRECTION('',(0.,0.,-1.));
#35223=DIRECTION('',(0.,0.,-1.));
#35224=DIRECTION('center_axis',(0.,0.,1.));
#35225=DIRECTION('ref_axis',(1.,0.,0.));
#35226=DIRECTION('center_axis',(0.,0.,1.));
#35227=DIRECTION('ref_axis',(1.,0.,0.));
#35228=DIRECTION('center_axis',(0.,0.,1.));
#35229=DIRECTION('ref_axis',(1.,0.,0.));
#35230=DIRECTION('center_axis',(0.,0.,1.));
#35231=DIRECTION('ref_axis',(1.,0.,0.));
#35232=DIRECTION('center_axis',(0.,0.,1.));
#35233=DIRECTION('ref_axis',(1.,0.,0.));
#35234=DIRECTION('center_axis',(0.,0.,1.));
#35235=DIRECTION('ref_axis',(1.,0.,0.));
#35236=DIRECTION('center_axis',(0.,0.,1.));
#35237=DIRECTION('ref_axis',(1.,0.,0.));
#35238=DIRECTION('center_axis',(0.,0.,1.));
#35239=DIRECTION('ref_axis',(1.,0.,0.));
#35240=DIRECTION('center_axis',(0.,0.,1.));
#35241=DIRECTION('ref_axis',(1.,0.,0.));
#35242=DIRECTION('center_axis',(0.,0.,1.));
#35243=DIRECTION('ref_axis',(1.,0.,0.));
#35244=DIRECTION('center_axis',(0.,0.,1.));
#35245=DIRECTION('ref_axis',(1.,0.,0.));
#35246=DIRECTION('center_axis',(0.,0.,-1.));
#35247=DIRECTION('ref_axis',(1.,9.16593808558309E-14,0.));
#35248=DIRECTION('center_axis',(0.,0.,1.));
#35249=DIRECTION('ref_axis',(0.888987483758174,0.457931494572398,0.));
#35250=DIRECTION('center_axis',(0.,0.,-1.));
#35251=DIRECTION('ref_axis',(-1.,0.,0.));
#35252=DIRECTION('center_axis',(0.,0.,-1.));
#35253=DIRECTION('ref_axis',(1.,0.,0.));
#35254=DIRECTION('center_axis',(-1.22464679914735E-16,-1.,0.));
#35255=DIRECTION('ref_axis',(1.,-1.22464679914735E-16,0.));
#35256=DIRECTION('center_axis',(0.,0.,1.));
#35257=DIRECTION('ref_axis',(1.,0.,0.));
#35258=DIRECTION('center_axis',(0.,0.,1.));
#35259=DIRECTION('ref_axis',(1.,0.,0.));
#35260=DIRECTION('',(3.20493781063927E-16,1.,0.));
#35261=DIRECTION('',(0.866025403784439,0.5,0.));
#35262=DIRECTION('',(0.866025403784439,-0.5,0.));
#35263=DIRECTION('',(1.60246890531964E-16,-1.,0.));
#35264=DIRECTION('',(-0.866025403784439,-0.5,0.));
#35265=DIRECTION('',(-0.866025403784439,0.5,0.));
#35266=DIRECTION('center_axis',(0.,0.,1.));
#35267=DIRECTION('ref_axis',(-0.978794305969862,-0.204845567686921,0.));
#35268=DIRECTION('center_axis',(0.,0.,-1.));
#35269=DIRECTION('ref_axis',(1.,0.,0.));
#35270=DIRECTION('',(0.866025403784438,1.06057523872491E-16,0.5));
#35271=DIRECTION('center_axis',(0.,0.,1.));
#35272=DIRECTION('ref_axis',(1.,0.,0.));
#35273=DIRECTION('center_axis',(-0.5,0.866025403784439,0.));
#35274=DIRECTION('ref_axis',(-0.866025403784439,-0.5,0.));
#35275=DIRECTION('',(0.,0.,1.));
#35276=DIRECTION('',(0.,0.,1.));
#35277=DIRECTION('center_axis',(0.5,0.866025403784439,0.));
#35278=DIRECTION('ref_axis',(-0.866025403784439,0.5,0.));
#35279=DIRECTION('',(0.,0.,1.));
#35280=DIRECTION('center_axis',(1.,-3.20493781063927E-16,0.));
#35281=DIRECTION('ref_axis',(3.20493781063927E-16,1.,0.));
#35282=DIRECTION('',(0.,0.,1.));
#35283=DIRECTION('center_axis',(0.5,-0.866025403784439,0.));
#35284=DIRECTION('ref_axis',(0.866025403784439,0.5,0.));
#35285=DIRECTION('',(0.,0.,1.));
#35286=DIRECTION('center_axis',(-0.5,-0.866025403784439,0.));
#35287=DIRECTION('ref_axis',(0.866025403784439,-0.5,0.));
#35288=DIRECTION('',(0.,0.,1.));
#35289=DIRECTION('center_axis',(-1.,-1.60246890531964E-16,0.));
#35290=DIRECTION('ref_axis',(1.60246890531964E-16,-1.,0.));
#35291=DIRECTION('center_axis',(0.,0.,1.));
#35292=DIRECTION('ref_axis',(1.,0.,0.));
#35293=DIRECTION('center_axis',(0.,0.,-1.));
#35294=DIRECTION('ref_axis',(-1.,0.,0.));
#35295=DIRECTION('center_axis',(0.,0.,1.));
#35296=DIRECTION('ref_axis',(1.,0.,0.));
#35297=DIRECTION('center_axis',(0.,0.,1.));
#35298=DIRECTION('ref_axis',(1.,0.,0.));
#35299=DIRECTION('',(0.707106781186548,8.65956056235493E-17,-0.707106781186547));
#35300=DIRECTION('',(0.,0.,1.));
#35301=DIRECTION('',(1.,0.,0.));
#35302=DIRECTION('',(-0.342020143325669,0.,0.939692620785908));
#35303=DIRECTION('',(0.939692620785908,0.,0.342020143325669));
#35304=DIRECTION('',(0.,0.,1.));
#35305=DIRECTION('',(1.,0.,0.));
#35306=DIRECTION('',(0.,0.,1.));
#35307=DIRECTION('',(1.,0.,0.));
#35308=DIRECTION('',(0.,0.,1.));
#35309=DIRECTION('',(1.,0.,0.));
#35310=DIRECTION('',(0.,0.,1.));
#35311=DIRECTION('',(1.,0.,0.));
#35312=DIRECTION('',(-1.,0.,-2.22044604925031E-16));
#35313=DIRECTION('',(-2.22044604925031E-16,0.,1.));
#35314=DIRECTION('',(-1.,0.,-2.22044604925031E-16));
#35315=DIRECTION('',(-2.22044604925031E-16,0.,1.));
#35316=DIRECTION('',(0.939692620785909,0.,0.342020143325669));
#35317=DIRECTION('',(0.342020143325669,0.,-0.939692620785908));
#35318=DIRECTION('',(0.,-1.,-2.22044604925031E-16));
#35319=DIRECTION('',(1.,0.,0.));
#35320=DIRECTION('',(0.,0.,1.));
#35321=DIRECTION('',(1.,0.,0.));
#35322=DIRECTION('',(-1.,0.,-2.22044604925031E-16));
#35323=DIRECTION('',(-2.22044604925031E-16,0.,1.));
#35324=DIRECTION('',(-1.,0.,-2.22044604925031E-16));
#35325=DIRECTION('',(-2.22044604925031E-16,0.,1.));
#35326=DIRECTION('',(-1.,0.,-2.22044604925031E-16));
#35327=DIRECTION('',(-2.22044604925031E-16,0.,1.));
#35328=DIRECTION('',(-1.,0.,-2.22044604925031E-16));
#35329=DIRECTION('',(-2.22044604925031E-16,0.,1.));
#35330=DIRECTION('',(-1.,0.,-2.22044604925031E-16));
#35331=DIRECTION('',(-2.22044604925031E-16,0.,1.));
#35332=DIRECTION('',(-1.,0.,-2.22044604925031E-16));
#35333=DIRECTION('',(-2.22044604925031E-16,0.,1.));
#35334=DIRECTION('',(0.,0.,1.));
#35335=DIRECTION('',(1.,0.,0.));
#35336=DIRECTION('',(0.,0.,1.));
#35337=DIRECTION('',(1.,0.,0.));
#35338=DIRECTION('',(0.,0.,1.));
#35339=DIRECTION('',(1.,0.,0.));
#35340=DIRECTION('',(-0.342020143325669,0.,0.939692620785908));
#35341=DIRECTION('',(0.939692620785908,0.,0.342020143325669));
#35342=DIRECTION('',(0.,0.,1.));
#35343=DIRECTION('',(1.,0.,0.));
#35344=DIRECTION('',(0.,-1.,-2.22044604925031E-16));
#35345=DIRECTION('',(1.,0.,0.));
#35346=CARTESIAN_POINT('',(0.,0.,0.));
#35347=CARTESIAN_POINT('',(0.,0.,0.));
#35348=CARTESIAN_POINT('Origin',(9.31,-4.875,78.));
#35349=CARTESIAN_POINT('',(15.56,-4.95,78.));
#35350=CARTESIAN_POINT('',(3.06,-4.95,78.));
#35351=CARTESIAN_POINT('Origin',(9.31,-4.95,78.));
#35352=CARTESIAN_POINT('Origin',(9.31,-4.95,78.));
#35353=CARTESIAN_POINT('',(15.41,-4.8,78.));
#35354=CARTESIAN_POINT('',(15.485,-4.875,78.));
#35355=CARTESIAN_POINT('Origin',(9.31,-4.8,78.));
#35356=CARTESIAN_POINT('Origin',(15.56,-4.8,78.));
#35357=CARTESIAN_POINT('',(4.2616449875437,-4.8,78.5128739112901));
#35358=CARTESIAN_POINT('',(3.31329278848646,-4.8,78.1987526588035));
#35359=CARTESIAN_POINT('Ctrl Pts',(4.2616449875437,-4.8,78.5128739112901));
#35360=CARTESIAN_POINT('Ctrl Pts',(4.21748868989439,-4.8,78.5162020803145));
#35361=CARTESIAN_POINT('Ctrl Pts',(4.15767750006772,-4.8,78.5102954843629));
#35362=CARTESIAN_POINT('Ctrl Pts',(3.96449151342978,-4.8,78.4820870104176));
#35363=CARTESIAN_POINT('Ctrl Pts',(3.82580660796765,-4.8,78.4380535018334));
#35364=CARTESIAN_POINT('Ctrl Pts',(3.56890774120608,-4.8,78.3375379190907));
#35365=CARTESIAN_POINT('Ctrl Pts',(3.43851411968528,-4.8,78.2720997066612));
#35366=CARTESIAN_POINT('Ctrl Pts',(3.31329278848645,-4.8,78.1987526588035));
#35367=CARTESIAN_POINT('',(3.31329278849671,-4.8,77.8012473408872));
#35368=CARTESIAN_POINT('Origin',(9.31,-4.8,78.));
#35369=CARTESIAN_POINT('',(4.2616449875437,-4.8,77.4871260887099));
#35370=CARTESIAN_POINT('Ctrl Pts',(3.3132927884967,-4.8,77.8012473408872));
#35371=CARTESIAN_POINT('Ctrl Pts',(3.35889085631205,-4.8,77.774538763147));
#35372=CARTESIAN_POINT('Ctrl Pts',(3.40424018038843,-4.8,77.7494140892238));
#35373=CARTESIAN_POINT('Ctrl Pts',(3.44932023931853,-4.8,77.7259332918199));
#35374=CARTESIAN_POINT('Ctrl Pts',(3.48535154467789,-4.8,77.7071657080717));
#35375=CARTESIAN_POINT('Ctrl Pts',(3.52121323519527,-4.8,77.6894485799316));
#35376=CARTESIAN_POINT('Ctrl Pts',(3.55687519269613,-4.8,77.6727963528265));
#35377=CARTESIAN_POINT('Ctrl Pts',(3.58544218901406,-4.8,77.6594570931859));
#35378=CARTESIAN_POINT('Ctrl Pts',(3.61388191592754,-4.8,77.6468005097403));
#35379=CARTESIAN_POINT('Ctrl Pts',(3.64214093417943,-4.8,77.6348321699585));
#35380=CARTESIAN_POINT('Ctrl Pts',(3.67299487491485,-4.8,77.6217648212262));
#35381=CARTESIAN_POINT('Ctrl Pts',(3.70363431536384,-4.8,77.609517604295));
#35382=CARTESIAN_POINT('Ctrl Pts',(3.73391380774594,-4.8,77.5981023686591));
#35383=CARTESIAN_POINT('Ctrl Pts',(3.76023545579461,-4.8,77.5881792229534));
#35384=CARTESIAN_POINT('Ctrl Pts',(3.78627885577575,-4.8,77.5788849711814));
#35385=CARTESIAN_POINT('Ctrl Pts',(3.81195344757976,-4.8,77.5702305821903));
#35386=CARTESIAN_POINT('Ctrl Pts',(3.83288569746951,-4.8,77.5631747413657));
#35387=CARTESIAN_POINT('Ctrl Pts',(3.85357165256806,-4.8,77.5565443368315));
#35388=CARTESIAN_POINT('Ctrl Pts',(3.87400245730923,-4.8,77.5503456729673));
#35389=CARTESIAN_POINT('Ctrl Pts',(3.89634471953046,-4.8,77.5435670768605));
#35390=CARTESIAN_POINT('Ctrl Pts',(3.91838596197266,-4.8,77.5373047098573));
#35391=CARTESIAN_POINT('Ctrl Pts',(3.94016536091701,-4.8,77.5315664445101));
#35392=CARTESIAN_POINT('Ctrl Pts',(3.95632811812935,-4.8,77.5273080079084));
#35393=CARTESIAN_POINT('Ctrl Pts',(3.97234882666259,-4.8,77.5233381875081));
#35394=CARTESIAN_POINT('Ctrl Pts',(3.98822206424162,-4.8,77.5196608232975));
#35395=CARTESIAN_POINT('Ctrl Pts',(4.0027286437008,-4.8,77.5163000737431));
#35396=CARTESIAN_POINT('Ctrl Pts',(4.01711313080281,-4.8,77.5131835791406));
#35397=CARTESIAN_POINT('Ctrl Pts',(4.03133253269136,-4.8,77.5103150376875));
#35398=CARTESIAN_POINT('Ctrl Pts',(4.04574667531631,-4.8,77.5074072103433));
#35399=CARTESIAN_POINT('Ctrl Pts',(4.05999158764115,-4.8,77.50475418481));
#35400=CARTESIAN_POINT('Ctrl Pts',(4.073966587985,-4.8,77.5023606915013));
#35401=CARTESIAN_POINT('Ctrl Pts',(4.09342501070055,-4.8,77.499028054405));
#35402=CARTESIAN_POINT('Ctrl Pts',(4.11235622185552,-4.8,77.4961988311417));
#35403=CARTESIAN_POINT('Ctrl Pts',(4.130391951486,-4.8,77.4938857626853));
#35404=CARTESIAN_POINT('Ctrl Pts',(4.14391874870886,-4.8,77.492150961343));
#35405=CARTESIAN_POINT('Ctrl Pts',(4.15693803977231,-4.8,77.4907065511493));
#35406=CARTESIAN_POINT('Ctrl Pts',(4.16931232039428,-4.8,77.4895559928397));
#35407=CARTESIAN_POINT('Ctrl Pts',(4.1812650340981,-4.8,77.4884446317437));
#35408=CARTESIAN_POINT('Ctrl Pts',(4.19261487926314,-4.8,77.48760745091));
#35409=CARTESIAN_POINT('Ctrl Pts',(4.20329220748563,-4.8,77.4870447436042));
#35410=CARTESIAN_POINT('Ctrl Pts',(4.21554028423639,-4.8,77.4863992560696));
#35411=CARTESIAN_POINT('Ctrl Pts',(4.22690460313112,-4.8,77.4861147687392));
#35412=CARTESIAN_POINT('Ctrl Pts',(4.23735441716533,-4.8,77.48618908429));
#35413=CARTESIAN_POINT('Ctrl Pts',(4.24608785219741,-4.8,77.4862511935327));
#35414=CARTESIAN_POINT('Ctrl Pts',(4.25418482587244,-4.8,77.4865637978906));
#35415=CARTESIAN_POINT('Ctrl Pts',(4.2616449875437,-4.8,77.4871260887099));
#35416=CARTESIAN_POINT('',(4.67850553742098,-4.8,77.5855617740846));
#35417=CARTESIAN_POINT('',(6.70986352030667,-4.8,78.0652380479502));
#35418=CARTESIAN_POINT('',(4.81607260887647,-4.8,76.805380142761));
#35419=CARTESIAN_POINT('Origin',(9.3100000000004,-4.8,78.0000000000001));
#35420=CARTESIAN_POINT('',(4.39068483903982,-4.8,76.7553047249138));
#35421=CARTESIAN_POINT('',(7.10167754842447,-4.8,77.0744349452193));
#35422=CARTESIAN_POINT('',(3.60696107145242,-4.8,76.1357717469497));
#35423=CARTESIAN_POINT('Ctrl Pts',(4.39068483903982,-4.8,76.7553047249138));
#35424=CARTESIAN_POINT('Ctrl Pts',(4.34805318890719,-4.8,76.743329836952));
#35425=CARTESIAN_POINT('Ctrl Pts',(4.29386922796023,-4.8,76.7173228188007));
#35426=CARTESIAN_POINT('Ctrl Pts',(4.12525248244484,-4.8,76.6265037376292));
#35427=CARTESIAN_POINT('Ctrl Pts',(4.00650765748837,-4.8,76.5376601133753));
#35428=CARTESIAN_POINT('Ctrl Pts',(3.79828001734992,-4.8,76.3505159793066));
#35429=CARTESIAN_POINT('Ctrl Pts',(3.70426215481285,-4.8,76.2532180870415));
#35430=CARTESIAN_POINT('Ctrl Pts',(3.60696107145241,-4.8,76.1357717469497));
#35431=CARTESIAN_POINT('',(3.74291589727828,-4.8,75.7622389329459));
#35432=CARTESIAN_POINT('Origin',(9.31,-4.8,78.));
#35433=CARTESIAN_POINT('',(4.7415112563347,-4.8,75.7914170652479));
#35434=CARTESIAN_POINT('Ctrl Pts',(3.74291589727827,-4.8,75.7622389329459));
#35435=CARTESIAN_POINT('Ctrl Pts',(3.79489893671569,-4.8,75.752736537219));
#35436=CARTESIAN_POINT('Ctrl Pts',(3.8461065065151,-4.8,75.7446374488288));
#35437=CARTESIAN_POINT('Ctrl Pts',(3.89649881094588,-4.8,75.7379910049808));
#35438=CARTESIAN_POINT('Ctrl Pts',(3.93677605596246,-4.8,75.7326786770295));
#35439=CARTESIAN_POINT('Ctrl Pts',(3.97653463813689,-4.8,75.7282954428482));
#35440=CARTESIAN_POINT('Ctrl Pts',(4.0157413150127,-4.8,75.7248445756745));
#35441=CARTESIAN_POINT('Ctrl Pts',(4.04714780575629,-4.8,75.7220802600889));
#35442=CARTESIAN_POINT('Ctrl Pts',(4.0782012133719,-4.8,75.7199139215761));
#35443=CARTESIAN_POINT('Ctrl Pts',(4.1088494172024,-4.8,75.7183325145388));
#35444=CARTESIAN_POINT('Ctrl Pts',(4.14231193316861,-4.8,75.7166058926941));
#35445=CARTESIAN_POINT('Ctrl Pts',(4.17529238322651,-4.8,75.7155765791924));
#35446=CARTESIAN_POINT('Ctrl Pts',(4.20765003841591,-4.8,75.7152059628458));
#35447=CARTESIAN_POINT('Ctrl Pts',(4.23577821253443,-4.8,75.7148837898989));
#35448=CARTESIAN_POINT('Ctrl Pts',(4.26342982460602,-4.8,75.7150574174935));
#35449=CARTESIAN_POINT('Ctrl Pts',(4.29051602439583,-4.8,75.7157061795936));
#35450=CARTESIAN_POINT('Ctrl Pts',(4.31259914472419,-4.8,75.7162351091457));
#35451=CARTESIAN_POINT('Ctrl Pts',(4.33430531587732,-4.8,75.7170795802567));
#35452=CARTESIAN_POINT('Ctrl Pts',(4.3556240601199,-4.8,75.7182424883248));
#35453=CARTESIAN_POINT('Ctrl Pts',(4.37893733544232,-4.8,75.7195141953099));
#35454=CARTESIAN_POINT('Ctrl Pts',(4.40179118394796,-4.8,75.7211680441458));
#35455=CARTESIAN_POINT('Ctrl Pts',(4.42421972672823,-4.8,75.7232248316902));
#35456=CARTESIAN_POINT('Ctrl Pts',(4.44086422150209,-4.8,75.7247511987782));
#35457=CARTESIAN_POINT('Ctrl Pts',(4.45727652162596,-4.8,75.7265001928719));
#35458=CARTESIAN_POINT('Ctrl Pts',(4.47345021847494,-4.8,75.7284735678523));
#35459=CARTESIAN_POINT('Ctrl Pts',(4.48823138815577,-4.8,75.7302770386792));
#35460=CARTESIAN_POINT('Ctrl Pts',(4.502814288437,-4.8,75.732268276036));
#35461=CARTESIAN_POINT('Ctrl Pts',(4.51715725439111,-4.8,75.7344360506685));
#35462=CARTESIAN_POINT('Ctrl Pts',(4.53169665335291,-4.8,75.7366335138949));
#35463=CARTESIAN_POINT('Ctrl Pts',(4.54598988049976,-4.8,75.7390125323308));
#35464=CARTESIAN_POINT('Ctrl Pts',(4.5599407081024,-4.8,75.7415431159479));
#35465=CARTESIAN_POINT('Ctrl Pts',(4.57936547336537,-4.8,75.7450666339885));
#35466=CARTESIAN_POINT('Ctrl Pts',(4.59812264414369,-4.8,75.7488828893195));
#35467=CARTESIAN_POINT('Ctrl Pts',(4.61586180219855,-4.8,75.752877898793));
#35468=CARTESIAN_POINT('Ctrl Pts',(4.62916617073969,-4.8,75.7558741558981));
#35469=CARTESIAN_POINT('Ctrl Pts',(4.64189431986447,-4.8,75.7589697140927));
#35470=CARTESIAN_POINT('Ctrl Pts',(4.65391585417251,-4.8,75.7621207961701));
#35471=CARTESIAN_POINT('Ctrl Pts',(4.66552783887808,-4.8,75.7651645271907));
#35472=CARTESIAN_POINT('Ctrl Pts',(4.67647953729782,-4.8,75.7682597101957));
#35473=CARTESIAN_POINT('Ctrl Pts',(4.68670540103973,-4.8,75.7713827996084));
#35474=CARTESIAN_POINT('Ctrl Pts',(4.69843559818659,-4.8,75.7749653287174));
#35475=CARTESIAN_POINT('Ctrl Pts',(4.70921186524681,-4.8,75.7785848240668));
#35476=CARTESIAN_POINT('Ctrl Pts',(4.71900606101744,-4.8,75.7822287047553));
#35477=CARTESIAN_POINT('Ctrl Pts',(4.72719156284253,-4.8,75.7852740790489));
#35478=CARTESIAN_POINT('Ctrl Pts',(4.7346933122562,-4.8,75.788337159151));
#35479=CARTESIAN_POINT('Ctrl Pts',(4.7415112563347,-4.8,75.7914170652479));
#35480=CARTESIAN_POINT('',(5.09956505173093,-4.8,76.0264910574324));
#35481=CARTESIAN_POINT('',(6.84435821048571,-4.8,77.1720046608023));
#35482=CARTESIAN_POINT('',(5.49567364700612,-4.8,75.340410845101));
#35483=CARTESIAN_POINT('Origin',(9.30999999999911,-4.8,77.9999999999995));
#35484=CARTESIAN_POINT('',(5.11306670030725,-4.8,75.1478641584586));
#35485=CARTESIAN_POINT('',(7.55141758063195,-4.8,76.3749625865681));
#35486=CARTESIAN_POINT('',(4.58850001706627,-4.8,74.2976442754434));
#35487=CARTESIAN_POINT('Ctrl Pts',(5.11306670030725,-4.8,75.1478641584586));
#35488=CARTESIAN_POINT('Ctrl Pts',(5.07710170456016,-4.8,75.122030560416));
#35489=CARTESIAN_POINT('Ctrl Pts',(5.03508035930635,-4.8,75.0790599492463));
#35490=CARTESIAN_POINT('Ctrl Pts',(4.9076944069207,-4.8,74.9360476103334));
#35491=CARTESIAN_POINT('Ctrl Pts',(4.82649707995744,-4.8,74.8119487900272));
#35492=CARTESIAN_POINT('Ctrl Pts',(4.69483416636455,-4.8,74.5648727807342));
#35493=CARTESIAN_POINT('Ctrl Pts',(4.63976411326715,-4.8,74.4412866656976));
#35494=CARTESIAN_POINT('Ctrl Pts',(4.58850001706627,-4.8,74.2976442754434));
#35495=CARTESIAN_POINT('',(4.84401151027683,-4.8,73.9931375354699));
#35496=CARTESIAN_POINT('Origin',(9.31,-4.8,78.));
#35497=CARTESIAN_POINT('',(5.77240469132477,-4.8,74.3620957389297));
#35498=CARTESIAN_POINT('Ctrl Pts',(4.84401151027683,-4.8,73.9931375354699));
#35499=CARTESIAN_POINT('Ctrl Pts',(5.02013219956813,-4.8,74.0230552009928));
#35500=CARTESIAN_POINT('Ctrl Pts',(5.19307522703524,-4.8,74.0670863794806));
#35501=CARTESIAN_POINT('Ctrl Pts',(5.45666781109844,-4.8,74.1681448115599));
#35502=CARTESIAN_POINT('Ctrl Pts',(5.53752890906739,-4.8,74.2065364265515));
#35503=CARTESIAN_POINT('Ctrl Pts',(5.67001324763651,-4.8,74.2823453026591));
#35504=CARTESIAN_POINT('Ctrl Pts',(5.735048362443,-4.8,74.3256280169092));
#35505=CARTESIAN_POINT('Ctrl Pts',(5.77240469132477,-4.8,74.3620957389297));
#35506=CARTESIAN_POINT('',(6.02846516020394,-4.8,74.7054546451438));
#35507=CARTESIAN_POINT('',(7.27624568947745,-4.8,76.3786397314713));
#35508=CARTESIAN_POINT('',(6.63533873676838,-4.8,74.1962272508773));
#35509=CARTESIAN_POINT('Origin',(9.30999999999964,-4.8,77.9999999999996));
#35510=CARTESIAN_POINT('',(6.34166065765632,-4.8,73.8844332675354));
#35511=CARTESIAN_POINT('',(8.21326860652757,-4.8,75.8714937229748));
#35512=CARTESIAN_POINT('',(6.13952154251132,-4.8,72.9060755452598));
#35513=CARTESIAN_POINT('Ctrl Pts',(6.34166065765632,-4.8,73.8844332675354));
#35514=CARTESIAN_POINT('Ctrl Pts',(6.31670022667317,-4.8,73.8478568720211));
#35515=CARTESIAN_POINT('Ctrl Pts',(6.29190989306677,-4.8,73.7931055577262));
#35516=CARTESIAN_POINT('Ctrl Pts',(6.22111935580918,-4.8,73.6151493613585));
#35517=CARTESIAN_POINT('Ctrl Pts',(6.18726312290577,-4.8,73.4707634940155));
#35518=CARTESIAN_POINT('Ctrl Pts',(6.14804542650294,-4.8,73.1935566226426));
#35519=CARTESIAN_POINT('Ctrl Pts',(6.13856544452442,-4.8,73.0585885938589));
#35520=CARTESIAN_POINT('Ctrl Pts',(6.13952154251132,-4.8,72.9060755452598));
#35521=CARTESIAN_POINT('',(6.48377124607659,-4.8,72.7073228862421));
#35522=CARTESIAN_POINT('Origin',(9.31,-4.8,78.));
#35523=CARTESIAN_POINT('',(7.22998432988738,-4.8,73.3715593562453));
#35524=CARTESIAN_POINT('Ctrl Pts',(6.4837712460766,-4.8,72.7073228862421));
#35525=CARTESIAN_POINT('Ctrl Pts',(6.63903811401181,-4.8,72.7956731192056));
#35526=CARTESIAN_POINT('Ctrl Pts',(6.78649185057934,-4.8,72.8961988916076));
#35527=CARTESIAN_POINT('Ctrl Pts',(6.99962383745534,-4.8,73.081316728015));
#35528=CARTESIAN_POINT('Ctrl Pts',(7.06247770883292,-4.8,73.1450491696213));
#35529=CARTESIAN_POINT('Ctrl Pts',(7.16104410153789,-4.8,73.2615985236155));
#35530=CARTESIAN_POINT('Ctrl Pts',(7.20735355880619,-4.8,73.3245142900275));
#35531=CARTESIAN_POINT('Ctrl Pts',(7.22998432988738,-4.8,73.3715593562453));
#35532=CARTESIAN_POINT('',(7.3531668006526,-4.8,73.7817890249619));
#35533=CARTESIAN_POINT('',(7.95343395333514,-4.8,75.7808347792541));
#35534=CARTESIAN_POINT('',(8.09760744867254,-4.8,73.5108347879048));
#35535=CARTESIAN_POINT('Origin',(9.30999999999986,-4.8,77.9999999999997));
#35536=CARTESIAN_POINT('',(7.92828014771504,-4.8,73.1174004638434));
#35537=CARTESIAN_POINT('',(9.00740162450745,-4.8,75.6247541297977));
#35538=CARTESIAN_POINT('',(8.07294956118024,-4.8,72.1289092826106));
#35539=CARTESIAN_POINT('Ctrl Pts',(7.92828014771504,-4.8,73.1174004638434));
#35540=CARTESIAN_POINT('Ctrl Pts',(7.91733487859675,-4.8,73.0744929233038));
#35541=CARTESIAN_POINT('Ctrl Pts',(7.91276563762517,-4.8,73.0145647221345));
#35542=CARTESIAN_POINT('Ctrl Pts',(7.90710889613904,-4.8,72.823128810336));
#35543=CARTESIAN_POINT('Ctrl Pts',(7.92467731891725,-4.8,72.6758709627745));
#35544=CARTESIAN_POINT('Ctrl Pts',(7.98263507276294,-4.8,72.4019684701976));
#35545=CARTESIAN_POINT('Ctrl Pts',(8.0198885882389,-4.8,72.2718976641637));
#35546=CARTESIAN_POINT('Ctrl Pts',(8.07294956118024,-4.8,72.1289092826106));
#35547=CARTESIAN_POINT('',(8.46441588028026,-4.8,72.0598832085154));
#35548=CARTESIAN_POINT('Origin',(9.31,-4.8,78.));
#35549=CARTESIAN_POINT('',(8.93844455602745,-4.8,72.9392812237066));
#35550=CARTESIAN_POINT('Ctrl Pts',(8.46441588028027,-4.8,72.0598832085154));
#35551=CARTESIAN_POINT('Ctrl Pts',(8.49863671609865,-4.8,72.1001506433736));
#35552=CARTESIAN_POINT('Ctrl Pts',(8.5312545173476,-4.8,72.1404481555372));
#35553=CARTESIAN_POINT('Ctrl Pts',(8.56220665880833,-4.8,72.1807659494296));
#35554=CARTESIAN_POINT('Ctrl Pts',(8.58694589561962,-4.8,72.2129909071785));
#35555=CARTESIAN_POINT('Ctrl Pts',(8.61062118189946,-4.8,72.2452312366064));
#35556=CARTESIAN_POINT('Ctrl Pts',(8.63321306170843,-4.8,72.2774597855078));
#35557=CARTESIAN_POINT('Ctrl Pts',(8.65131027380309,-4.8,72.3032764457372));
#35558=CARTESIAN_POINT('Ctrl Pts',(8.66871308103186,-4.8,72.3290863155335));
#35559=CARTESIAN_POINT('Ctrl Pts',(8.68540672089436,-4.8,72.3548377342902));
#35560=CARTESIAN_POINT('Ctrl Pts',(8.70363327657302,-4.8,72.3829538115291));
#35561=CARTESIAN_POINT('Ctrl Pts',(8.72101491260155,-4.8,72.4110010616084));
#35562=CARTESIAN_POINT('Ctrl Pts',(8.73751470277175,-4.8,72.4388383040863));
#35563=CARTESIAN_POINT('Ctrl Pts',(8.75185779942539,-4.8,72.4630369305726));
#35564=CARTESIAN_POINT('Ctrl Pts',(8.76553323921084,-4.8,72.4870707424861));
#35565=CARTESIAN_POINT('Ctrl Pts',(8.77851449432001,-4.8,72.5108524602548));
#35566=CARTESIAN_POINT('Ctrl Pts',(8.7890979878147,-4.8,72.5302414679572));
#35567=CARTESIAN_POINT('Ctrl Pts',(8.79921973972455,-4.8,72.5494617988781));
#35568=CARTESIAN_POINT('Ctrl Pts',(8.80887200369403,-4.8,72.5685058267365));
#35569=CARTESIAN_POINT('Ctrl Pts',(8.81942731012063,-4.8,72.5893315677521));
#35570=CARTESIAN_POINT('Ctrl Pts',(8.82942195864573,-4.8,72.6099505044235));
#35571=CARTESIAN_POINT('Ctrl Pts',(8.83885499921122,-4.8,72.6304025849049));
#35572=CARTESIAN_POINT('Ctrl Pts',(8.84585537382384,-4.8,72.6455803236184));
#35573=CARTESIAN_POINT('Ctrl Pts',(8.85254685047463,-4.8,72.6606682893708));
#35574=CARTESIAN_POINT('Ctrl Pts',(8.85892470594634,-4.8,72.6756618090688));
#35575=CARTESIAN_POINT('Ctrl Pts',(8.86475343918438,-4.8,72.6893644128682));
#35576=CARTESIAN_POINT('Ctrl Pts',(8.87032042714041,-4.8,72.7029891935948));
#35577=CARTESIAN_POINT('Ctrl Pts',(8.87561456216956,-4.8,72.7164944537335));
#35578=CARTESIAN_POINT('Ctrl Pts',(8.88098120268016,-4.8,72.7301846742829));
#35579=CARTESIAN_POINT('Ctrl Pts',(8.88606752585608,-4.8,72.7437524813858));
#35580=CARTESIAN_POINT('Ctrl Pts',(8.89085138995626,-4.8,72.7570995443649));
#35581=CARTESIAN_POINT('Ctrl Pts',(8.8975123163246,-4.8,72.7756836433015));
#35582=CARTESIAN_POINT('Ctrl Pts',(8.90358592752971,-4.8,72.7938359570949));
#35583=CARTESIAN_POINT('Ctrl Pts',(8.90899572675103,-4.8,72.8111960230857));
#35584=CARTESIAN_POINT('Ctrl Pts',(8.91305307616702,-4.8,72.8242160725788));
#35585=CARTESIAN_POINT('Ctrl Pts',(8.91673631861236,-4.8,72.8367867519676));
#35586=CARTESIAN_POINT('Ctrl Pts',(8.92001816856195,-4.8,72.848773246926));
#35587=CARTESIAN_POINT('Ctrl Pts',(8.92318821249884,-4.8,72.8603513861618));
#35588=CARTESIAN_POINT('Ctrl Pts',(8.9259835545623,-4.8,72.8713834266871));
#35589=CARTESIAN_POINT('Ctrl Pts',(8.92839181162883,-4.8,72.8818008291423));
#35590=CARTESIAN_POINT('Ctrl Pts',(8.93115434897723,-4.8,72.8937507425281));
#35591=CARTESIAN_POINT('Ctrl Pts',(8.93340790756747,-4.8,72.9048930113212));
#35592=CARTESIAN_POINT('Ctrl Pts',(8.93514931218717,-4.8,72.9151969740743));
#35593=CARTESIAN_POINT('Ctrl Pts',(8.93660469147692,-4.8,72.9238085131869));
#35594=CARTESIAN_POINT('Ctrl Pts',(8.93770286092992,-4.8,72.9318367583111));
#35595=CARTESIAN_POINT('Ctrl Pts',(8.93844455602745,-4.8,72.9392812237066));
#35596=CARTESIAN_POINT('',(8.91389140472481,-4.8,73.3669019025333));
#35597=CARTESIAN_POINT('',(8.79424410320319,-4.8,75.4506939040492));
#35598=CARTESIAN_POINT('',(9.70610859527519,-4.8,73.3669019025333));
#35599=CARTESIAN_POINT('Origin',(9.31,-4.8,77.9999999999998));
#35600=CARTESIAN_POINT('',(9.68155544397255,-4.8,72.9392812237066));
#35601=CARTESIAN_POINT('',(9.83803247244813,-4.8,75.6645042434626));
#35602=CARTESIAN_POINT('',(10.1555841196959,-4.8,72.059883208512));
#35603=CARTESIAN_POINT('Ctrl Pts',(9.68155544397255,-4.8,72.9392812237066));
#35604=CARTESIAN_POINT('Ctrl Pts',(9.68594549850892,-4.8,72.8952178217337));
#35605=CARTESIAN_POINT('Ctrl Pts',(9.70214846866658,-4.8,72.8373409606809));
#35606=CARTESIAN_POINT('Ctrl Pts',(9.76230780748678,-4.8,72.6555153293997));
#35607=CARTESIAN_POINT('Ctrl Pts',(9.82918187492197,-4.8,72.5231469708476));
#35608=CARTESIAN_POINT('Ctrl Pts',(9.97732451803297,-4.8,72.2855855392203));
#35609=CARTESIAN_POINT('Ctrl Pts',(10.0568182077383,-4.8,72.1761004145255));
#35610=CARTESIAN_POINT('Ctrl Pts',(10.1555841196959,-4.8,72.059883208512));
#35611=CARTESIAN_POINT('',(10.5470504387829,-4.8,72.1289092826028));
#35612=CARTESIAN_POINT('Origin',(9.31,-4.8,78.));
#35613=CARTESIAN_POINT('',(10.691719852285,-4.8,73.1174004638434));
#35614=CARTESIAN_POINT('Ctrl Pts',(10.5470504387829,-4.8,72.1289092826028));
#35615=CARTESIAN_POINT('Ctrl Pts',(10.5654352318417,-4.8,72.1784525091694));
#35616=CARTESIAN_POINT('Ctrl Pts',(10.5823033781278,-4.8,72.2274757290437));
#35617=CARTESIAN_POINT('Ctrl Pts',(10.5975993794282,-4.8,72.2759483183091));
#35618=CARTESIAN_POINT('Ctrl Pts',(10.6098250724357,-4.8,72.3146911886841));
#35619=CARTESIAN_POINT('Ctrl Pts',(10.6210457216483,-4.8,72.3530846112338));
#35620=CARTESIAN_POINT('Ctrl Pts',(10.6312523310667,-4.8,72.3910964169147));
#35621=CARTESIAN_POINT('Ctrl Pts',(10.6394283300246,-4.8,72.4215457533097));
#35622=CARTESIAN_POINT('Ctrl Pts',(10.6469541243075,-4.8,72.4517512083325));
#35623=CARTESIAN_POINT('Ctrl Pts',(10.6538335106752,-4.8,72.4816591878217));
#35624=CARTESIAN_POINT('Ctrl Pts',(10.6613446055808,-4.8,72.5143135061535));
#35625=CARTESIAN_POINT('Ctrl Pts',(10.6680852760586,-4.8,72.5466141686034));
#35626=CARTESIAN_POINT('Ctrl Pts',(10.674069109378,-4.8,72.5784158794642));
#35627=CARTESIAN_POINT('Ctrl Pts',(10.6792707939463,-4.8,72.6060607786114));
#35628=CARTESIAN_POINT('Ctrl Pts',(10.6839014561727,-4.8,72.6333224506243));
#35629=CARTESIAN_POINT('Ctrl Pts',(10.6879660194427,-4.8,72.6601098064801));
#35630=CARTESIAN_POINT('Ctrl Pts',(10.6912798190807,-4.8,72.6819492820257));
#35631=CARTESIAN_POINT('Ctrl Pts',(10.6942174144141,-4.8,72.703472328323));
#35632=CARTESIAN_POINT('Ctrl Pts',(10.6967741345915,-4.8,72.7246691295972));
#35633=CARTESIAN_POINT('Ctrl Pts',(10.6995700554658,-4.8,72.7478490534988));
#35634=CARTESIAN_POINT('Ctrl Pts',(10.7019098614498,-4.8,72.7706428885429));
#35635=CARTESIAN_POINT('Ctrl Pts',(10.7037789967056,-4.8,72.7930878487832));
#35636=CARTESIAN_POINT('Ctrl Pts',(10.7051661047424,-4.8,72.8097445271263));
#35637=CARTESIAN_POINT('Ctrl Pts',(10.7062936478012,-4.8,72.8262111971522));
#35638=CARTESIAN_POINT('Ctrl Pts',(10.7071587858016,-4.8,72.8424818521564));
#35639=CARTESIAN_POINT('Ctrl Pts',(10.7079494369223,-4.8,72.8573516320174));
#35640=CARTESIAN_POINT('Ctrl Pts',(10.708520744992,-4.8,72.8720587599544));
#35641=CARTESIAN_POINT('Ctrl Pts',(10.7088765336285,-4.8,72.8865602540843));
#35642=CARTESIAN_POINT('Ctrl Pts',(10.7092371949417,-4.8,72.901260352345));
#35643=CARTESIAN_POINT('Ctrl Pts',(10.7093763119928,-4.8,72.9157495454271));
#35644=CARTESIAN_POINT('Ctrl Pts',(10.7093067094224,-4.8,72.9299278598028));
#35645=CARTESIAN_POINT('Ctrl Pts',(10.7092097966346,-4.8,72.9496693717271));
#35646=CARTESIAN_POINT('Ctrl Pts',(10.7087086673265,-4.8,72.9688042647236));
#35647=CARTESIAN_POINT('Ctrl Pts',(10.7078547234915,-4.8,72.9869676512239));
#35648=CARTESIAN_POINT('Ctrl Pts',(10.7072142656153,-4.8,73.0005901910992));
#35649=CARTESIAN_POINT('Ctrl Pts',(10.7063759558006,-4.8,73.0136625090764));
#35650=CARTESIAN_POINT('Ctrl Pts',(10.7053602632569,-4.8,73.0260485889224));
#35651=CARTESIAN_POINT('Ctrl Pts',(10.7043791733311,-4.8,73.0380126997465));
#35652=CARTESIAN_POINT('Ctrl Pts',(10.7032327555811,-4.8,73.0493354900672));
#35653=CARTESIAN_POINT('Ctrl Pts',(10.7019328155191,-4.8,73.0599483186778));
#35654=CARTESIAN_POINT('Ctrl Pts',(10.7004416404183,-4.8,73.0721224074963));
#35655=CARTESIAN_POINT('Ctrl Pts',(10.6987484124568,-4.8,73.0833634776816));
#35656=CARTESIAN_POINT('Ctrl Pts',(10.6968606347447,-4.8,73.0936416309137));
#35657=CARTESIAN_POINT('Ctrl Pts',(10.6952829240073,-4.8,73.1022316002785));
#35658=CARTESIAN_POINT('Ctrl Pts',(10.6935690441008,-4.8,73.1101512795537));
#35659=CARTESIAN_POINT('Ctrl Pts',(10.691719852285,-4.8,73.1174004638434));
#35660=CARTESIAN_POINT('',(10.5223925513275,-4.8,73.5108347879048));
#35661=CARTESIAN_POINT('',(9.6972620259713,-4.8,75.428036967767));
#35662=CARTESIAN_POINT('',(11.2668331993474,-4.8,73.7817890249619));
#35663=CARTESIAN_POINT('Origin',(9.31000000000015,-4.8,77.9999999999997));
#35664=CARTESIAN_POINT('',(11.3900156701126,-4.8,73.3715593562453));
#35665=CARTESIAN_POINT('',(10.6049748112822,-4.8,75.9859496136124));
#35666=CARTESIAN_POINT('',(12.1362287539072,-4.8,72.7073228862334));
#35667=CARTESIAN_POINT('Ctrl Pts',(11.3900156701126,-4.8,73.3715593562453));
#35668=CARTESIAN_POINT('Ctrl Pts',(11.4092115433894,-4.8,73.3316547888187));
#35669=CARTESIAN_POINT('Ctrl Pts',(11.4442324080663,-4.8,73.2828100711267));
#35670=CARTESIAN_POINT('Ctrl Pts',(11.5629517209604,-4.8,73.1325255753574));
#35671=CARTESIAN_POINT('Ctrl Pts',(11.6710654337471,-4.8,73.0310122834859));
#35672=CARTESIAN_POINT('Ctrl Pts',(11.8915247771686,-4.8,72.8584453271068));
#35673=CARTESIAN_POINT('Ctrl Pts',(12.0036705291132,-4.8,72.7827514061615));
#35674=CARTESIAN_POINT('Ctrl Pts',(12.1362287539072,-4.8,72.7073228862334));
#35675=CARTESIAN_POINT('',(12.4804784574649,-4.8,72.906075545245));
#35676=CARTESIAN_POINT('Origin',(9.31,-4.8,78.));
#35677=CARTESIAN_POINT('',(12.2783393423437,-4.8,73.8844332675354));
#35678=CARTESIAN_POINT('Ctrl Pts',(12.4804784574649,-4.8,72.906075545245));
#35679=CARTESIAN_POINT('Ctrl Pts',(12.4808097303897,-4.8,72.9589189192183));
#35680=CARTESIAN_POINT('Ctrl Pts',(12.4798936743185,-4.8,73.0107549230007));
#35681=CARTESIAN_POINT('Ctrl Pts',(12.4776886119537,-4.8,73.0615357980059));
#35682=CARTESIAN_POINT('Ctrl Pts',(12.4759261634347,-4.8,73.1021236196345));
#35683=CARTESIAN_POINT('Ctrl Pts',(12.473338800909,-4.8,73.1420393225299));
#35684=CARTESIAN_POINT('Ctrl Pts',(12.4699290733643,-4.8,73.1812496008697));
#35685=CARTESIAN_POINT('Ctrl Pts',(12.467197712867,-4.8,73.2126589741824));
#35686=CARTESIAN_POINT('Ctrl Pts',(12.4639387721653,-4.8,73.2436167908666));
#35687=CARTESIAN_POINT('Ctrl Pts',(12.4601741493332,-4.8,73.2740739874536));
#35688=CARTESIAN_POINT('Ctrl Pts',(12.4560638351902,-4.8,73.3073279551069));
#35689=CARTESIAN_POINT('Ctrl Pts',(12.4513505163371,-4.8,73.3399860942704));
#35690=CARTESIAN_POINT('Ctrl Pts',(12.4460966546888,-4.8,73.3719165187634));
#35691=CARTESIAN_POINT('Ctrl Pts',(12.4415295269319,-4.8,73.399673307532));
#35692=CARTESIAN_POINT('Ctrl Pts',(12.4365568850902,-4.8,73.4268746794466));
#35693=CARTESIAN_POINT('Ctrl Pts',(12.4312145099132,-4.8,73.4534367227204));
#35694=CARTESIAN_POINT('Ctrl Pts',(12.4268589224052,-4.8,73.4750925031618));
#35695=CARTESIAN_POINT('Ctrl Pts',(12.4222580436605,-4.8,73.4963222679185));
#35696=CARTESIAN_POINT('Ctrl Pts',(12.4174108417078,-4.8,73.5171151956521));
#35697=CARTESIAN_POINT('Ctrl Pts',(12.4121101469542,-4.8,73.5398534607422));
#35698=CARTESIAN_POINT('Ctrl Pts',(12.4065128945608,-4.8,73.5620729204852));
#35699=CARTESIAN_POINT('Ctrl Pts',(12.4005926785574,-4.8,73.5838035662621));
#35700=CARTESIAN_POINT('Ctrl Pts',(12.3961992142276,-4.8,73.5999301428989));
#35701=CARTESIAN_POINT('Ctrl Pts',(12.3916268252751,-4.8,73.6157893936696));
#35702=CARTESIAN_POINT('Ctrl Pts',(12.3868748973112,-4.8,73.6313747027535));
#35703=CARTESIAN_POINT('Ctrl Pts',(12.3825321020783,-4.8,73.6456181438387));
#35704=CARTESIAN_POINT('Ctrl Pts',(12.3780388220321,-4.8,73.6596337223663));
#35705=CARTESIAN_POINT('Ctrl Pts',(12.3734133508682,-4.8,73.6733823563325));
#35706=CARTESIAN_POINT('Ctrl Pts',(12.3687245319211,-4.8,73.6873192836534));
#35707=CARTESIAN_POINT('Ctrl Pts',(12.3638996632849,-4.8,73.7009822523324));
#35708=CARTESIAN_POINT('Ctrl Pts',(12.3589849891398,-4.8,73.7142817042695));
#35709=CARTESIAN_POINT('Ctrl Pts',(12.3521419261712,-4.8,73.7327995112222));
#35710=CARTESIAN_POINT('Ctrl Pts',(12.3451264998134,-4.8,73.750609032654));
#35711=CARTESIAN_POINT('Ctrl Pts',(12.3381118110373,-4.8,73.7673849669295));
#35712=CARTESIAN_POINT('Ctrl Pts',(12.3328507944552,-4.8,73.7799669176362));
#35713=CARTESIAN_POINT('Ctrl Pts',(12.3275920448378,-4.8,73.7919641595396));
#35714=CARTESIAN_POINT('Ctrl Pts',(12.322401317242,-4.8,73.8032558800705));
#35715=CARTESIAN_POINT('Ctrl Pts',(12.317387427334,-4.8,73.8141629143099));
#35716=CARTESIAN_POINT('Ctrl Pts',(12.3124375246201,-4.8,73.824410758949));
#35717=CARTESIAN_POINT('Ctrl Pts',(12.3075861793309,-4.8,73.833938950071));
#35718=CARTESIAN_POINT('Ctrl Pts',(12.3020211495231,-4.8,73.8448688395031));
#35719=CARTESIAN_POINT('Ctrl Pts',(12.2965853632991,-4.8,73.8548528720717));
#35720=CARTESIAN_POINT('Ctrl Pts',(12.2912960971058,-4.8,73.8638655187556));
#35721=CARTESIAN_POINT('Ctrl Pts',(12.2868755914205,-4.8,73.8713978407167));
#35722=CARTESIAN_POINT('Ctrl Pts',(12.2825563812865,-4.8,73.8782537234236));
#35723=CARTESIAN_POINT('Ctrl Pts',(12.2783393423437,-4.8,73.8844332675354));
#35724=CARTESIAN_POINT('',(11.9846612632316,-4.8,74.1962272508773));
#35725=CARTESIAN_POINT('',(10.5535704330285,-4.8,75.7155967313038));
#35726=CARTESIAN_POINT('',(12.5915348397961,-4.8,74.7054546451438));
#35727=CARTESIAN_POINT('Origin',(9.3099999999996,-4.8,78.0000000000005));
#35728=CARTESIAN_POINT('',(12.8475953086752,-4.8,74.3620957389297));
#35729=CARTESIAN_POINT('',(11.215724076083,-4.8,76.5503191845784));
#35730=CARTESIAN_POINT('',(13.7759884897161,-4.8,73.993137535462));
#35731=CARTESIAN_POINT('Ctrl Pts',(12.8475953086752,-4.8,74.3620957389297));
#35732=CARTESIAN_POINT('Ctrl Pts',(12.879281694861,-4.8,74.3311630868456));
#35733=CARTESIAN_POINT('Ctrl Pts',(12.9288964200912,-4.8,74.2972419073571));
#35734=CARTESIAN_POINT('Ctrl Pts',(13.0918564069193,-4.8,74.1966250720879));
#35735=CARTESIAN_POINT('Ctrl Pts',(13.2281696557251,-4.8,74.1382108482666));
#35736=CARTESIAN_POINT('Ctrl Pts',(13.4943550490169,-4.8,74.0514524889784));
#35737=CARTESIAN_POINT('Ctrl Pts',(13.6256264304604,-4.8,74.0186795760604));
#35738=CARTESIAN_POINT('Ctrl Pts',(13.7759884897161,-4.8,73.993137535462));
#35739=CARTESIAN_POINT('',(14.0314999829165,-4.8,74.2976442754215));
#35740=CARTESIAN_POINT('Origin',(9.31,-4.8,78.));
#35741=CARTESIAN_POINT('',(13.5069332996928,-4.8,75.1478641584586));
#35742=CARTESIAN_POINT('Ctrl Pts',(14.0314999829165,-4.8,74.2976442754215));
#35743=CARTESIAN_POINT('Ctrl Pts',(14.0137377793038,-4.8,74.3474141060163));
#35744=CARTESIAN_POINT('Ctrl Pts',(13.9951480107643,-4.8,74.3958107066136));
#35745=CARTESIAN_POINT('Ctrl Pts',(13.9757078478022,-4.8,74.4427749443781));
#35746=CARTESIAN_POINT('Ctrl Pts',(13.9601698370925,-4.8,74.4803122238127));
#35747=CARTESIAN_POINT('Ctrl Pts',(13.9440865390346,-4.8,74.5169357812344));
#35748=CARTESIAN_POINT('Ctrl Pts',(13.9274717401505,-4.8,74.5526151912231));
#35749=CARTESIAN_POINT('Ctrl Pts',(13.9141624622321,-4.8,74.5811961681471));
#35750=CARTESIAN_POINT('Ctrl Pts',(13.9005118625272,-4.8,74.6091723775572));
#35751=CARTESIAN_POINT('Ctrl Pts',(13.8865572991921,-4.8,74.6365052044542));
#35752=CARTESIAN_POINT('Ctrl Pts',(13.8713213407319,-4.8,74.6663479021583));
#35753=CARTESIAN_POINT('Ctrl Pts',(13.8557225285405,-4.8,74.6954244644896));
#35754=CARTESIAN_POINT('Ctrl Pts',(13.8398646653426,-4.8,74.7236323222161));
#35755=CARTESIAN_POINT('Ctrl Pts',(13.826079588047,-4.8,74.7481531226702));
#35756=CARTESIAN_POINT('Ctrl Pts',(13.8121034158961,-4.8,74.7720133080073));
#35757=CARTESIAN_POINT('Ctrl Pts',(13.797998471323,-4.8,74.7951462646713));
#35758=CARTESIAN_POINT('Ctrl Pts',(13.7864988446753,-4.8,74.8140063433844));
#35759=CARTESIAN_POINT('Ctrl Pts',(13.7749144256038,-4.8,74.8323822037526));
#35760=CARTESIAN_POINT('Ctrl Pts',(13.7632479454926,-4.8,74.8502633240851));
#35761=CARTESIAN_POINT('Ctrl Pts',(13.7504899762601,-4.8,74.8698173610244));
#35762=CARTESIAN_POINT('Ctrl Pts',(13.7376307758707,-4.8,74.8887824516424));
#35763=CARTESIAN_POINT('Ctrl Pts',(13.7246352731669,-4.8,74.9071777472498));
#35764=CARTESIAN_POINT('Ctrl Pts',(13.7149911530288,-4.8,74.9208291191789));
#35765=CARTESIAN_POINT('Ctrl Pts',(13.7052703295732,-4.8,74.934168091134));
#35766=CARTESIAN_POINT('Ctrl Pts',(13.6954744882065,-4.8,74.9471882361456));
#35767=CARTESIAN_POINT('Ctrl Pts',(13.6865220518115,-4.8,74.9590873692274));
#35768=CARTESIAN_POINT('Ctrl Pts',(13.6775061395318,-4.8,74.9707209127091));
#35769=CARTESIAN_POINT('Ctrl Pts',(13.6684573086483,-4.8,74.9820583983343));
#35770=CARTESIAN_POINT('Ctrl Pts',(13.6592845502886,-4.8,74.9935511555076));
#35771=CARTESIAN_POINT('Ctrl Pts',(13.6500776464114,-4.8,75.0047399440415));
#35772=CARTESIAN_POINT('Ctrl Pts',(13.6409106830007,-4.8,75.0155564232949));
#35773=CARTESIAN_POINT('Ctrl Pts',(13.6281468440578,-4.8,75.0306170047475));
#35774=CARTESIAN_POINT('Ctrl Pts',(13.6154632844137,-4.8,75.0449530637636));
#35775=CARTESIAN_POINT('Ctrl Pts',(13.6031339254938,-4.8,75.0583181208055));
#35776=CARTESIAN_POINT('Ctrl Pts',(13.5938869063039,-4.8,75.0683419135868));
#35777=CARTESIAN_POINT('Ctrl Pts',(13.5848419995513,-4.8,75.0778170351574));
#35778=CARTESIAN_POINT('Ctrl Pts',(13.5761023151156,-4.8,75.0866524483868));
#35779=CARTESIAN_POINT('Ctrl Pts',(13.5676603743603,-4.8,75.095186856646));
#35780=CARTESIAN_POINT('Ctrl Pts',(13.5595040180152,-4.8,75.1031237142177));
#35781=CARTESIAN_POINT('Ctrl Pts',(13.5516864113499,-4.8,75.1104180273209));
#35782=CARTESIAN_POINT('Ctrl Pts',(13.5427187516189,-4.8,75.1187854114427));
#35783=CARTESIAN_POINT('Ctrl Pts',(13.5341960432185,-4.8,75.1263081847801));
#35784=CARTESIAN_POINT('Ctrl Pts',(13.5261432521403,-4.8,75.1329682667954));
#35785=CARTESIAN_POINT('Ctrl Pts',(13.5194131292823,-4.8,75.1385344325844));
#35786=CARTESIAN_POINT('Ctrl Pts',(13.513009548998,-4.8,75.1434995984469));
#35787=CARTESIAN_POINT('Ctrl Pts',(13.5069332996928,-4.8,75.1478641584586));
#35788=CARTESIAN_POINT('',(13.1243263529939,-4.8,75.340410845101));
#35789=CARTESIAN_POINT('',(11.2598858927175,-4.8,76.278689243247));
#35790=CARTESIAN_POINT('',(13.5204349482691,-4.8,76.0264910574324));
#35791=CARTESIAN_POINT('Origin',(9.31000000000134,-4.8,77.9999999999992));
#35792=CARTESIAN_POINT('',(13.8784887436653,-4.8,75.7914170652479));
#35793=CARTESIAN_POINT('',(11.5966148918162,-4.8,77.2895416568946));
#35794=CARTESIAN_POINT('',(14.8770841027247,-4.8,75.7622389329533));
#35795=CARTESIAN_POINT('Ctrl Pts',(13.8784887436653,-4.8,75.7914170652479));
#35796=CARTESIAN_POINT('Ctrl Pts',(13.9188438003731,-4.8,75.7731872611009));
#35797=CARTESIAN_POINT('Ctrl Pts',(13.9770681225745,-4.8,75.7582810146635));
#35798=CARTESIAN_POINT('Ctrl Pts',(14.1646133920406,-4.8,75.7194677169264));
#35799=CARTESIAN_POINT('Ctrl Pts',(14.3126847875687,-4.8,75.7111981783716));
#35800=CARTESIAN_POINT('Ctrl Pts',(14.5924903467623,-4.8,75.7207127544627));
#35801=CARTESIAN_POINT('Ctrl Pts',(14.7270540920481,-4.8,75.7348137468176));
#35802=CARTESIAN_POINT('Ctrl Pts',(14.8770841027247,-4.8,75.7622389329533));
#35803=CARTESIAN_POINT('',(15.0130389285309,-4.8,76.1357717468986));
#35804=CARTESIAN_POINT('Origin',(9.31,-4.8,78.));
#35805=CARTESIAN_POINT('',(14.2293151609602,-4.8,76.7553047249138));
#35806=CARTESIAN_POINT('Ctrl Pts',(15.0130389285309,-4.8,76.1357717468986));
#35807=CARTESIAN_POINT('Ctrl Pts',(14.9793256322769,-4.8,76.1764650580252));
#35808=CARTESIAN_POINT('Ctrl Pts',(14.9453043517147,-4.8,76.2155849111935));
#35809=CARTESIAN_POINT('Ctrl Pts',(14.9109738587163,-4.8,76.2530679315487));
#35810=CARTESIAN_POINT('Ctrl Pts',(14.8835344011301,-4.8,76.2830271211033));
#35811=CARTESIAN_POINT('Ctrl Pts',(14.8558950524031,-4.8,76.3119411937235));
#35812=CARTESIAN_POINT('Ctrl Pts',(14.8280791737289,-4.8,76.3397862741419));
#35813=CARTESIAN_POINT('Ctrl Pts',(14.8057972733803,-4.8,76.362091566538));
#35814=CARTESIAN_POINT('Ctrl Pts',(14.7834014781299,-4.8,76.3837118244195));
#35815=CARTESIAN_POINT('Ctrl Pts',(14.7609401002719,-4.8,76.4046235388012));
#35816=CARTESIAN_POINT('Ctrl Pts',(14.7364161792257,-4.8,76.4274554966482));
#35817=CARTESIAN_POINT('Ctrl Pts',(14.7118133209326,-4.8,76.4494434194877));
#35818=CARTESIAN_POINT('Ctrl Pts',(14.6872641487802,-4.8,76.4705264263976));
#35819=CARTESIAN_POINT('Ctrl Pts',(14.6659238053871,-4.8,76.4888536679202));
#35820=CARTESIAN_POINT('Ctrl Pts',(14.6446298352381,-4.8,76.5064947759896));
#35821=CARTESIAN_POINT('Ctrl Pts',(14.6234635854471,-4.8,76.5234084698624));
#35822=CARTESIAN_POINT('Ctrl Pts',(14.6062069441493,-4.8,76.537198042936));
#35823=CARTESIAN_POINT('Ctrl Pts',(14.5890362364622,-4.8,76.5505035988803));
#35824=CARTESIAN_POINT('Ctrl Pts',(14.5719576276826,-4.8,76.5633161847262));
#35825=CARTESIAN_POINT('Ctrl Pts',(14.5532811825371,-4.8,76.5773274873921));
#35826=CARTESIAN_POINT('Ctrl Pts',(14.5347110427406,-4.8,76.5907507383831));
#35827=CARTESIAN_POINT('Ctrl Pts',(14.5162077020452,-4.8,76.6035919390039));
#35828=CARTESIAN_POINT('Ctrl Pts',(14.5024761492368,-4.8,76.613121549216));
#35829=CARTESIAN_POINT('Ctrl Pts',(14.4887793659718,-4.8,76.622331365394));
#35830=CARTESIAN_POINT('Ctrl Pts',(14.475121134166,-4.8,76.6312159246056));
#35831=CARTESIAN_POINT('Ctrl Pts',(14.4626388525233,-4.8,76.6393355386176));
#35832=CARTESIAN_POINT('Ctrl Pts',(14.4501877600528,-4.8,76.647183870011));
#35833=CARTESIAN_POINT('Ctrl Pts',(14.437806991961,-4.8,76.6547427391965));
#35834=CARTESIAN_POINT('Ctrl Pts',(14.4252566642583,-4.8,76.6624051301431));
#35835=CARTESIAN_POINT('Ctrl Pts',(14.4127782136582,-4.8,76.6697702055542));
#35836=CARTESIAN_POINT('Ctrl Pts',(14.4004646320838,-4.8,76.676799085134));
#35837=CARTESIAN_POINT('Ctrl Pts',(14.3833195243853,-4.8,76.6865859125219));
#35838=CARTESIAN_POINT('Ctrl Pts',(14.3664976558123,-4.8,76.6957193686518));
#35839=CARTESIAN_POINT('Ctrl Pts',(14.3503407292824,-4.8,76.7040615251609));
#35840=CARTESIAN_POINT('Ctrl Pts',(14.3382230343849,-4.8,76.7103181425427));
#35841=CARTESIAN_POINT('Ctrl Pts',(14.3264829196606,-4.8,76.7161283041536));
#35842=CARTESIAN_POINT('Ctrl Pts',(14.3152484132406,-4.8,76.7214417287278));
#35843=CARTESIAN_POINT('Ctrl Pts',(14.3043966442584,-4.8,76.7265741354244));
#35844=CARTESIAN_POINT('Ctrl Pts',(14.2940176112058,-4.8,76.7312427037723));
#35845=CARTESIAN_POINT('Ctrl Pts',(14.284176661876,-4.8,76.7354233370412));
#35846=CARTESIAN_POINT('Ctrl Pts',(14.2728880043614,-4.8,76.740218985874));
#35847=CARTESIAN_POINT('Ctrl Pts',(14.262306338214,-4.8,76.7443731425178));
#35848=CARTESIAN_POINT('Ctrl Pts',(14.252461307702,-4.8,76.7478773556981));
#35849=CARTESIAN_POINT('Ctrl Pts',(14.2442333196509,-4.8,76.7508060032163));
#35850=CARTESIAN_POINT('Ctrl Pts',(14.2365177353778,-4.8,76.7532815796345));
#35851=CARTESIAN_POINT('Ctrl Pts',(14.2293151609602,-4.8,76.7553047249138));
#35852=CARTESIAN_POINT('',(13.8039273911235,-4.8,76.805380142761));
#35853=CARTESIAN_POINT('',(11.7310163364939,-4.8,77.0493972362957));
#35854=CARTESIAN_POINT('',(13.941494462579,-4.8,77.5855617740846));
#35855=CARTESIAN_POINT('Origin',(9.30999999999972,-4.8,78.0000000000001));
#35856=CARTESIAN_POINT('',(14.3583550124563,-4.8,77.4871260887099));
#35857=CARTESIAN_POINT('',(11.7017062047547,-4.8,78.1144558906375));
#35858=CARTESIAN_POINT('',(15.3067072115039,-4.8,77.8012473409061));
#35859=CARTESIAN_POINT('Ctrl Pts',(14.3583550124563,-4.8,77.4871260887099));
#35860=CARTESIAN_POINT('Ctrl Pts',(14.4025113203035,-4.8,77.4837979186678));
#35861=CARTESIAN_POINT('Ctrl Pts',(14.4623225212488,-4.8,77.4897045193554));
#35862=CARTESIAN_POINT('Ctrl Pts',(14.6555084752939,-4.8,77.5179129863291));
#35863=CARTESIAN_POINT('Ctrl Pts',(14.7941933832081,-4.8,77.5619464951834));
#35864=CARTESIAN_POINT('Ctrl Pts',(15.0510922509005,-4.8,77.6624620772393));
#35865=CARTESIAN_POINT('Ctrl Pts',(15.1814858790588,-4.8,77.7279002923833));
#35866=CARTESIAN_POINT('Ctrl Pts',(15.3067072115039,-4.8,77.8012473409061));
#35867=CARTESIAN_POINT('',(15.306707211514,-4.8,78.1987526587886));
#35868=CARTESIAN_POINT('Origin',(9.31,-4.8,78.));
#35869=CARTESIAN_POINT('',(14.3583550124563,-4.8,78.5128739112901));
#35870=CARTESIAN_POINT('Ctrl Pts',(15.306707211514,-4.8,78.1987526587886));
#35871=CARTESIAN_POINT('Ctrl Pts',(15.1815741357754,-4.8,78.2720480119657));
#35872=CARTESIAN_POINT('Ctrl Pts',(14.9949210075704,-4.8,78.369958518309));
#35873=CARTESIAN_POINT('Ctrl Pts',(14.5626620354579,-4.8,78.5088509137435));
#35874=CARTESIAN_POINT('Ctrl Pts',(14.4186035570618,-4.8,78.5174149926455));
#35875=CARTESIAN_POINT('Ctrl Pts',(14.3583550124563,-4.8,78.5128739112901));
#35876=CARTESIAN_POINT('',(13.941494462579,-4.8,78.4144382259154));
#35877=CARTESIAN_POINT('',(11.9101364796933,-4.8,77.9347619520498));
#35878=CARTESIAN_POINT('',(13.8039273911235,-4.8,79.194619857239));
#35879=CARTESIAN_POINT('Origin',(9.30999999999925,-4.8,77.9999999999999));
#35880=CARTESIAN_POINT('',(14.2293151609602,-4.8,79.2446952750862));
#35881=CARTESIAN_POINT('',(11.5183224515755,-4.8,78.9255650547807));
#35882=CARTESIAN_POINT('',(15.0130389285914,-4.8,79.8642282529162));
#35883=CARTESIAN_POINT('Ctrl Pts',(14.2293151609602,-4.8,79.2446952750862));
#35884=CARTESIAN_POINT('Ctrl Pts',(14.2719468183276,-4.8,79.2566701648679));
#35885=CARTESIAN_POINT('Ctrl Pts',(14.3261307856426,-4.8,79.2826771890912));
#35886=CARTESIAN_POINT('Ctrl Pts',(14.4947475082523,-4.8,79.37349625589));
#35887=CARTESIAN_POINT('Ctrl Pts',(14.6134923348285,-4.8,79.462339880326));
#35888=CARTESIAN_POINT('Ctrl Pts',(14.8217199770457,-4.8,79.649484015153));
#35889=CARTESIAN_POINT('Ctrl Pts',(14.9157378424995,-4.8,79.7467819095626));
#35890=CARTESIAN_POINT('Ctrl Pts',(15.0130389285914,-4.8,79.8642282529162));
#35891=CARTESIAN_POINT('',(14.877084102819,-4.8,80.237761066812));
#35892=CARTESIAN_POINT('Origin',(9.31,-4.8,78.));
#35893=CARTESIAN_POINT('',(13.8784887436653,-4.8,80.2085829347521));
#35894=CARTESIAN_POINT('Ctrl Pts',(14.877084102819,-4.8,80.237761066812));
#35895=CARTESIAN_POINT('Ctrl Pts',(14.7013523439929,-4.8,80.2698844812177));
#35896=CARTESIAN_POINT('Ctrl Pts',(14.5237795116491,-4.8,80.28765870646));
#35897=CARTESIAN_POINT('Ctrl Pts',(14.2415194834978,-4.8,80.2828488169659));
#35898=CARTESIAN_POINT('Ctrl Pts',(14.152404201208,-4.8,80.2744286239328));
#35899=CARTESIAN_POINT('Ctrl Pts',(14.0019814789273,-4.8,80.2485038942336));
#35900=CARTESIAN_POINT('Ctrl Pts',(13.9260649040323,-4.8,80.2300747661684));
#35901=CARTESIAN_POINT('Ctrl Pts',(13.8784887436653,-4.8,80.2085829347521));
#35902=CARTESIAN_POINT('',(13.5204349482691,-4.8,79.9735089425676));
#35903=CARTESIAN_POINT('',(11.7756417895143,-4.8,78.8279953391977));
#35904=CARTESIAN_POINT('',(13.1243263529939,-4.8,80.659589154899));
#35905=CARTESIAN_POINT('Origin',(9.31000000000061,-4.8,78.0000000000004));
#35906=CARTESIAN_POINT('',(13.5069332996928,-4.8,80.8521358415414));
#35907=CARTESIAN_POINT('',(11.0685824193681,-4.8,79.6250374134319));
#35908=CARTESIAN_POINT('',(14.0314999829639,-4.8,81.7023557245181));
#35909=CARTESIAN_POINT('Ctrl Pts',(13.5069332996928,-4.8,80.8521358415414));
#35910=CARTESIAN_POINT('Ctrl Pts',(13.5428982988443,-4.8,80.8779694418353));
#35911=CARTESIAN_POINT('Ctrl Pts',(13.5849196460621,-4.8,80.9209400573754));
#35912=CARTESIAN_POINT('Ctrl Pts',(13.7123055878643,-4.8,81.0639523822528));
#35913=CARTESIAN_POINT('Ctrl Pts',(13.7935029159474,-4.8,81.1880512030957));
#35914=CARTESIAN_POINT('Ctrl Pts',(13.925165831458,-4.8,81.4351272145176));
#35915=CARTESIAN_POINT('Ctrl Pts',(13.980235885705,-4.8,81.5587133313075));
#35916=CARTESIAN_POINT('Ctrl Pts',(14.0314999829639,-4.8,81.7023557245181));
#35917=CARTESIAN_POINT('',(13.7759884899248,-4.8,82.0068624643054));
#35918=CARTESIAN_POINT('Origin',(9.31,-4.8,78.));
#35919=CARTESIAN_POINT('',(12.8475953086752,-4.8,81.6379042610703));
#35920=CARTESIAN_POINT('Ctrl Pts',(13.7759884899248,-4.8,82.0068624643054));
#35921=CARTESIAN_POINT('Ctrl Pts',(13.7238904006001,-4.8,81.998012548872));
#35922=CARTESIAN_POINT('Ctrl Pts',(13.6730009737443,-4.8,81.9881091822482));
#35923=CARTESIAN_POINT('Ctrl Pts',(13.6233744794367,-4.8,81.9771196133808));
#35924=CARTESIAN_POINT('Ctrl Pts',(13.5837093382832,-4.8,81.9683359423513));
#35925=CARTESIAN_POINT('Ctrl Pts',(13.5448493490778,-4.8,81.9588566022824));
#35926=CARTESIAN_POINT('Ctrl Pts',(13.5068268689897,-4.8,81.94868988692));
#35927=CARTESIAN_POINT('Ctrl Pts',(13.476368967432,-4.8,81.9405458412145));
#35928=CARTESIAN_POINT('Ctrl Pts',(13.446447375747,-4.8,81.9319606423288));
#35929=CARTESIAN_POINT('Ctrl Pts',(13.417106609469,-4.8,81.9229643754468));
#35930=CARTESIAN_POINT('Ctrl Pts',(13.3850715928299,-4.8,81.9131420157808));
#35931=CARTESIAN_POINT('Ctrl Pts',(13.3537280633307,-4.8,81.9028292769294));
#35932=CARTESIAN_POINT('Ctrl Pts',(13.3231950570889,-4.8,81.8921105736537));
#35933=CARTESIAN_POINT('Ctrl Pts',(13.2966530278779,-4.8,81.8827929148161));
#35934=CARTESIAN_POINT('Ctrl Pts',(13.2707283943044,-4.8,81.8731723496375));
#35935=CARTESIAN_POINT('Ctrl Pts',(13.2454975801038,-4.8,81.8632986864201));
#35936=CARTESIAN_POINT('Ctrl Pts',(13.2249271382615,-4.8,81.8552487831007));
#35937=CARTESIAN_POINT('Ctrl Pts',(13.2048188343683,-4.8,81.8470312918966));
#35938=CARTESIAN_POINT('Ctrl Pts',(13.1851835045775,-4.8,81.8386470756315));
#35939=CARTESIAN_POINT('Ctrl Pts',(13.1637111360262,-4.8,81.8294784503231));
#35940=CARTESIAN_POINT('Ctrl Pts',(13.1428011879323,-4.8,81.8201078622799));
#35941=CARTESIAN_POINT('Ctrl Pts',(13.1224287098858,-4.8,81.8105040987335));
#35942=CARTESIAN_POINT('Ctrl Pts',(13.1073100487301,-4.8,81.8033770302175));
#35943=CARTESIAN_POINT('Ctrl Pts',(13.0924857221107,-4.8,81.7961201759903));
#35944=CARTESIAN_POINT('Ctrl Pts',(13.0779623520226,-4.8,81.7887340798196));
#35945=CARTESIAN_POINT('Ctrl Pts',(13.0646894190553,-4.8,81.7819839137929));
#35946=CARTESIAN_POINT('Ctrl Pts',(13.0516670183166,-4.8,81.7751251170702));
#35947=CARTESIAN_POINT('Ctrl Pts',(13.038930461394,-4.8,81.7681824919383));
#35948=CARTESIAN_POINT('Ctrl Pts',(13.0260194723549,-4.8,81.7611447848463));
#35949=CARTESIAN_POINT('Ctrl Pts',(13.0134019046673,-4.8,81.7540206673816));
#35950=CARTESIAN_POINT('Ctrl Pts',(13.0011579256109,-4.8,81.7468712327598));
#35951=CARTESIAN_POINT('Ctrl Pts',(12.9841097302923,-4.8,81.7369165474986));
#35952=CARTESIAN_POINT('Ctrl Pts',(12.9677889906484,-4.8,81.7269151098885));
#35953=CARTESIAN_POINT('Ctrl Pts',(12.9524860076116,-4.8,81.7170938791618));
#35954=CARTESIAN_POINT('Ctrl Pts',(12.941008770334,-4.8,81.7097279561167));
#35955=CARTESIAN_POINT('Ctrl Pts',(12.9301069651891,-4.8,81.7024657992042));
#35956=CARTESIAN_POINT('Ctrl Pts',(12.9198881511031,-4.8,81.6953931434104));
#35957=CARTESIAN_POINT('Ctrl Pts',(12.910017471913,-4.8,81.6885614390878));
#35958=CARTESIAN_POINT('Ctrl Pts',(12.9007848564824,-4.8,81.6819072169133));
#35959=CARTESIAN_POINT('Ctrl Pts',(12.8922438470947,-4.8,81.6754750213747));
#35960=CARTESIAN_POINT('Ctrl Pts',(12.8824463647866,-4.8,81.6680965817627));
#35961=CARTESIAN_POINT('Ctrl Pts',(12.8735579266505,-4.8,81.6610096685258));
#35962=CARTESIAN_POINT('Ctrl Pts',(12.8656006738454,-4.8,81.6542357287195));
#35963=CARTESIAN_POINT('Ctrl Pts',(12.8589503961148,-4.8,81.6485744053777));
#35964=CARTESIAN_POINT('Ctrl Pts',(12.8529486914522,-4.8,81.6431303012078));
#35965=CARTESIAN_POINT('Ctrl Pts',(12.8475953086752,-4.8,81.6379042610703));
#35966=CARTESIAN_POINT('',(12.5915348397961,-4.8,81.2945453548562));
#35967=CARTESIAN_POINT('',(11.3437543105226,-4.8,79.6213602685287));
#35968=CARTESIAN_POINT('',(11.9846612632316,-4.8,81.8037727491227));
#35969=CARTESIAN_POINT('Origin',(9.31000000000031,-4.8,78.0000000000004));
#35970=CARTESIAN_POINT('',(12.2783393423437,-4.8,82.1155667324646));
#35971=CARTESIAN_POINT('',(10.4067313934724,-4.8,80.1285062770252));
#35972=CARTESIAN_POINT('',(12.4804784574569,-4.8,83.09392445476));
#35973=CARTESIAN_POINT('Ctrl Pts',(12.2783393423437,-4.8,82.1155667324646));
#35974=CARTESIAN_POINT('Ctrl Pts',(12.3032997740142,-4.8,82.1521431288428));
#35975=CARTESIAN_POINT('Ctrl Pts',(12.3280901075719,-4.8,82.2068944444417));
#35976=CARTESIAN_POINT('Ctrl Pts',(12.3988806429637,-4.8,82.3848506340573));
#35977=CARTESIAN_POINT('Ctrl Pts',(12.4327368762941,-4.8,82.5292365018844));
#35978=CARTESIAN_POINT('Ctrl Pts',(12.4719545734303,-4.8,82.8064433756322));
#35979=CARTESIAN_POINT('Ctrl Pts',(12.4814345554706,-4.8,82.9414114045802));
#35980=CARTESIAN_POINT('Ctrl Pts',(12.4804784574569,-4.8,83.0939244547599));
#35981=CARTESIAN_POINT('',(12.1362287541399,-4.8,83.2926771136423));
#35982=CARTESIAN_POINT('Origin',(9.31,-4.8,78.));
#35983=CARTESIAN_POINT('',(11.3900156701126,-4.8,82.6284406437547));
#35984=CARTESIAN_POINT('Ctrl Pts',(12.1362287541399,-4.8,83.2926771136423));
#35985=CARTESIAN_POINT('Ctrl Pts',(12.0902994133922,-4.8,83.2665423174371));
#35986=CARTESIAN_POINT('Ctrl Pts',(12.0458661453988,-4.8,83.2398309878294));
#35987=CARTESIAN_POINT('Ctrl Pts',(12.0029911488357,-4.8,83.2125309103598));
#35988=CARTESIAN_POINT('Ctrl Pts',(11.9687223008297,-4.8,83.1907106822467));
#35989=CARTESIAN_POINT('Ctrl Pts',(11.9354479809844,-4.8,83.1685121172559));
#35990=CARTESIAN_POINT('Ctrl Pts',(11.9031957584663,-4.8,83.1459540757644));
#35991=CARTESIAN_POINT('Ctrl Pts',(11.8773601205811,-4.8,83.1278839600987));
#35992=CARTESIAN_POINT('Ctrl Pts',(11.8521793324076,-4.8,83.1095827248216));
#35993=CARTESIAN_POINT('Ctrl Pts',(11.8276849351316,-4.8,83.0910938659688));
#35994=CARTESIAN_POINT('Ctrl Pts',(11.800941310303,-4.8,83.0709072453674));
#35995=CARTESIAN_POINT('Ctrl Pts',(11.775015190457,-4.8,83.0504963215801));
#35996=CARTESIAN_POINT('Ctrl Pts',(11.7499895614165,-4.8,83.0299811312968));
#35997=CARTESIAN_POINT('Ctrl Pts',(11.7282350396413,-4.8,83.0121474875143));
#35998=CARTESIAN_POINT('Ctrl Pts',(11.707164280057,-4.8,82.9942403666271));
#35999=CARTESIAN_POINT('Ctrl Pts',(11.6868320620375,-4.8,82.9763327115825));
#36000=CARTESIAN_POINT('Ctrl Pts',(11.6702553987293,-4.8,82.9617327713285));
#36001=CARTESIAN_POINT('Ctrl Pts',(11.6541703214774,-4.8,82.9471334104638));
#36002=CARTESIAN_POINT('Ctrl Pts',(11.6385867178304,-4.8,82.9325391459589));
#36003=CARTESIAN_POINT('Ctrl Pts',(11.6215451465656,-4.8,82.9165794742263));
#36004=CARTESIAN_POINT('Ctrl Pts',(11.6051011529476,-4.8,82.9006223787257));
#36005=CARTESIAN_POINT('Ctrl Pts',(11.5892419666579,-4.8,82.8846299955104));
#36006=CARTESIAN_POINT('Ctrl Pts',(11.5774726734063,-4.8,82.8727618552153));
#36007=CARTESIAN_POINT('Ctrl Pts',(11.5660243534712,-4.8,82.8608724245862));
#36008=CARTESIAN_POINT('Ctrl Pts',(11.554903043514,-4.8,82.848964479454));
#36009=CARTESIAN_POINT('Ctrl Pts',(11.5447392590945,-4.8,82.8380817877867));
#36010=CARTESIAN_POINT('Ctrl Pts',(11.5348480518501,-4.8,82.8271827037259));
#36011=CARTESIAN_POINT('Ctrl Pts',(11.5252541209383,-4.8,82.816302611073));
#36012=CARTESIAN_POINT('Ctrl Pts',(11.5155287973603,-4.8,82.8052735112617));
#36013=CARTESIAN_POINT('Ctrl Pts',(11.5061087537551,-4.8,82.7942635682762));
#36014=CARTESIAN_POINT('Ctrl Pts',(11.4970484276151,-4.8,82.7833576097878));
#36015=CARTESIAN_POINT('Ctrl Pts',(11.4844330673021,-4.8,82.7681724394347));
#36016=CARTESIAN_POINT('Ctrl Pts',(11.472517281958,-4.8,82.7531921407433));
#36017=CARTESIAN_POINT('Ctrl Pts',(11.4614962405913,-4.8,82.7387292743878));
#36018=CARTESIAN_POINT('Ctrl Pts',(11.4532304595662,-4.8,82.7278821246212));
#36019=CARTESIAN_POINT('Ctrl Pts',(11.4454699177556,-4.8,82.7173292925021));
#36020=CARTESIAN_POINT('Ctrl Pts',(11.4382863643943,-4.8,82.7071881298805));
#36021=CARTESIAN_POINT('Ctrl Pts',(11.4313475404717,-4.8,82.6973924565885));
#36022=CARTESIAN_POINT('Ctrl Pts',(11.4249475978921,-4.8,82.6879817926255));
#36023=CARTESIAN_POINT('Ctrl Pts',(11.4191216148336,-4.8,82.6790163086589));
#36024=CARTESIAN_POINT('Ctrl Pts',(11.412438568019,-4.8,82.6687319071316));
#36025=CARTESIAN_POINT('Ctrl Pts',(11.4065100354132,-4.8,82.6590323622077));
#36026=CARTESIAN_POINT('Ctrl Pts',(11.4013494875778,-4.8,82.6499454002511));
#36027=CARTESIAN_POINT('Ctrl Pts',(11.3970365574561,-4.8,82.6423509678021));
#36028=CARTESIAN_POINT('Ctrl Pts',(11.3932587932986,-4.8,82.6351824796365));
#36029=CARTESIAN_POINT('Ctrl Pts',(11.3900156701126,-4.8,82.6284406437547));
#36030=CARTESIAN_POINT('',(11.2668331993474,-4.8,82.2182109750381));
#36031=CARTESIAN_POINT('',(10.6665660466648,-4.8,80.2191652207459));
#36032=CARTESIAN_POINT('',(10.5223925513275,-4.8,82.4891652120952));
#36033=CARTESIAN_POINT('Origin',(9.31000000000013,-4.8,78.0000000000003));
#36034=CARTESIAN_POINT('',(10.691719852285,-4.8,82.8825995361566));
#36035=CARTESIAN_POINT('',(9.61259837549256,-4.8,80.3752458702023));
#36036=CARTESIAN_POINT('',(10.5470504386678,-4.8,83.8710907174214));
#36037=CARTESIAN_POINT('Ctrl Pts',(10.691719852285,-4.8,82.8825995361566));
#36038=CARTESIAN_POINT('Ctrl Pts',(10.7026651208567,-4.8,82.9255070744082));
#36039=CARTESIAN_POINT('Ctrl Pts',(10.7072343621118,-4.8,82.9854352727938));
#36040=CARTESIAN_POINT('Ctrl Pts',(10.7128911041171,-4.8,83.1768711873215));
#36041=CARTESIAN_POINT('Ctrl Pts',(10.6953226813375,-4.8,83.3241290352659));
#36042=CARTESIAN_POINT('Ctrl Pts',(10.6373649270984,-4.8,83.5980315310389));
#36043=CARTESIAN_POINT('Ctrl Pts',(10.6001114118967,-4.8,83.7281023352314));
#36044=CARTESIAN_POINT('Ctrl Pts',(10.5470504386678,-4.8,83.8710907174214));
#36045=CARTESIAN_POINT('',(10.1555841198781,-4.8,83.9401167914621));
#36046=CARTESIAN_POINT('Origin',(9.31,-4.8,78.));
#36047=CARTESIAN_POINT('',(9.68155544397255,-4.8,83.0607187762934));
#36048=CARTESIAN_POINT('Ctrl Pts',(10.1555841198781,-4.8,83.9401167914621));
#36049=CARTESIAN_POINT('Ctrl Pts',(10.1213632840485,-4.8,83.8998493566156));
#36050=CARTESIAN_POINT('Ctrl Pts',(10.0887454828079,-4.8,83.8595518445941));
#36051=CARTESIAN_POINT('Ctrl Pts',(10.0577933413463,-4.8,83.8192340507748));
#36052=CARTESIAN_POINT('Ctrl Pts',(10.0330541147877,-4.8,83.78700910644));
#36053=CARTESIAN_POINT('Ctrl Pts',(10.0093788378727,-4.8,83.7547687903993));
#36054=CARTESIAN_POINT('Ctrl Pts',(9.98678696651789,-4.8,83.7225402548213));
#36055=CARTESIAN_POINT('Ctrl Pts',(9.96868975187523,-4.8,83.6967235919687));
#36056=CARTESIAN_POINT('Ctrl Pts',(9.95128694223038,-4.8,83.6709137195168));
#36057=CARTESIAN_POINT('Ctrl Pts',(9.93459330008706,-4.8,83.6451622980894));
#36058=CARTESIAN_POINT('Ctrl Pts',(9.9163667435806,-4.8,83.6170462204991));
#36059=CARTESIAN_POINT('Ctrl Pts',(9.89898510673091,-4.8,83.588998970037));
#36060=CARTESIAN_POINT('Ctrl Pts',(9.88248531574176,-4.8,83.5611617271314));
#36061=CARTESIAN_POINT('Ctrl Pts',(9.86814221774207,-4.8,83.5369630992034));
#36062=CARTESIAN_POINT('Ctrl Pts',(9.85446677667117,-4.8,83.5129292858282));
#36063=CARTESIAN_POINT('Ctrl Pts',(9.84148552034242,-4.8,83.4891475666002));
#36064=CARTESIAN_POINT('Ctrl Pts',(9.83090202589081,-4.8,83.4697585577767));
#36065=CARTESIAN_POINT('Ctrl Pts',(9.8207802730647,-4.8,83.4505382257358));
#36066=CARTESIAN_POINT('Ctrl Pts',(9.81112800822446,-4.8,83.431494196779));
#36067=CARTESIAN_POINT('Ctrl Pts',(9.8005726990786,-4.8,83.4106684510759));
#36068=CARTESIAN_POINT('Ctrl Pts',(9.79057804807715,-4.8,83.3900495098162));
#36069=CARTESIAN_POINT('Ctrl Pts',(9.78114500527958,-4.8,83.3695974248259));
#36070=CARTESIAN_POINT('Ctrl Pts',(9.77414463034711,-4.8,83.3544196856643));
#36071=CARTESIAN_POINT('Ctrl Pts',(9.76745315339273,-4.8,83.3393317194716));
#36072=CARTESIAN_POINT('Ctrl Pts',(9.7610752976329,-4.8,83.3243381993367));
#36073=CARTESIAN_POINT('Ctrl Pts',(9.75524656418418,-4.8,83.3106355952616));
#36074=CARTESIAN_POINT('Ctrl Pts',(9.74967957602566,-4.8,83.2970108142608));
#36075=CARTESIAN_POINT('Ctrl Pts',(9.74438544080102,-4.8,83.2835055538423));
#36076=CARTESIAN_POINT('Ctrl Pts',(9.73901880027901,-4.8,83.2698153334857));
#36077=CARTESIAN_POINT('Ctrl Pts',(9.73393247707929,-4.8,83.2562475265611));
#36078=CARTESIAN_POINT('Ctrl Pts',(9.72914861293952,-4.8,83.2429004637275));
#36079=CARTESIAN_POINT('Ctrl Pts',(9.7224876861611,-4.8,83.224316364003));
#36080=CARTESIAN_POINT('Ctrl Pts',(9.71641407457747,-4.8,83.2061640494016));
#36081=CARTESIAN_POINT('Ctrl Pts',(9.71100427501583,-4.8,83.1888039826073));
#36082=CARTESIAN_POINT('Ctrl Pts',(9.7069469253446,-4.8,83.1757839325116));
#36083=CARTESIAN_POINT('Ctrl Pts',(9.70326368266569,-4.8,83.1632132525234));
#36084=CARTESIAN_POINT('Ctrl Pts',(9.69998183250857,-4.8,83.1512267569901));
#36085=CARTESIAN_POINT('Ctrl Pts',(9.69681178844634,-4.8,83.1396486174734));
#36086=CARTESIAN_POINT('Ctrl Pts',(9.69401644626419,-4.8,83.1286165766646));
#36087=CARTESIAN_POINT('Ctrl Pts',(9.69160818908845,-4.8,83.1181991739405));
#36088=CARTESIAN_POINT('Ctrl Pts',(9.68884565180793,-4.8,83.1062492610819));
#36089=CARTESIAN_POINT('Ctrl Pts',(9.68659209322686,-4.8,83.0951069927227));
#36090=CARTESIAN_POINT('Ctrl Pts',(9.68485068856013,-4.8,83.0848030303271));
#36091=CARTESIAN_POINT('Ctrl Pts',(9.68339530889577,-4.8,83.0761914895294));
#36092=CARTESIAN_POINT('Ctrl Pts',(9.68229713919365,-4.8,83.0681632429366));
#36093=CARTESIAN_POINT('Ctrl Pts',(9.68155544397255,-4.8,83.0607187762934));
#36094=CARTESIAN_POINT('',(9.70610859527519,-4.8,82.6330980974667));
#36095=CARTESIAN_POINT('',(9.82575589679681,-4.8,80.5493060959508));
#36096=CARTESIAN_POINT('',(8.91389140472481,-4.8,82.6330980974667));
#36097=CARTESIAN_POINT('Origin',(9.31,-4.8,78.0000000000002));
#36098=CARTESIAN_POINT('',(8.93844455602746,-4.8,83.0607187762934));
#36099=CARTESIAN_POINT('',(8.78196752755185,-4.8,80.3354957565374));
#36100=CARTESIAN_POINT('',(8.46441588009367,-4.8,83.9401167914581));
#36101=CARTESIAN_POINT('Ctrl Pts',(8.93844455602746,-4.8,83.0607187762934));
#36102=CARTESIAN_POINT('Ctrl Pts',(8.93405450203344,-4.8,83.1047821724661));
#36103=CARTESIAN_POINT('Ctrl Pts',(8.91785153528776,-4.8,83.1626590275444));
#36104=CARTESIAN_POINT('Ctrl Pts',(8.85769219190737,-4.8,83.3444846720947));
#36105=CARTESIAN_POINT('Ctrl Pts',(8.79081812423295,-4.8,83.476853030494));
#36106=CARTESIAN_POINT('Ctrl Pts',(8.64267547983925,-4.8,83.7144144641847));
#36107=CARTESIAN_POINT('Ctrl Pts',(8.56318179159508,-4.8,83.823899586071));
#36108=CARTESIAN_POINT('Ctrl Pts',(8.46441588009366,-4.8,83.9401167914581));
#36109=CARTESIAN_POINT('',(8.07294956130202,-4.8,83.871090717415));
#36110=CARTESIAN_POINT('Origin',(9.31,-4.8,78.));
#36111=CARTESIAN_POINT('',(7.92828014771505,-4.8,82.8825995361566));
#36112=CARTESIAN_POINT('Ctrl Pts',(8.07294956130203,-4.8,83.871090717415));
#36113=CARTESIAN_POINT('Ctrl Pts',(8.05456476823445,-4.8,83.8215474908588));
#36114=CARTESIAN_POINT('Ctrl Pts',(8.03769662195923,-4.8,83.772524271155));
#36115=CARTESIAN_POINT('Ctrl Pts',(8.02240062066062,-4.8,83.7240516819751));
#36116=CARTESIAN_POINT('Ctrl Pts',(8.01017493288046,-4.8,83.6853088282291));
#36117=CARTESIAN_POINT('Ctrl Pts',(7.99895428802889,-4.8,83.6469154219601));
#36118=CARTESIAN_POINT('Ctrl Pts',(7.9887476820989,-4.8,83.6089036321699));
#36119=CARTESIAN_POINT('Ctrl Pts',(7.98057168151374,-4.8,83.5784542920367));
#36120=CARTESIAN_POINT('Ctrl Pts',(7.97304588574899,-4.8,83.548248833292));
#36121=CARTESIAN_POINT('Ctrl Pts',(7.96616649805019,-4.8,83.5183408501214));
#36122=CARTESIAN_POINT('Ctrl Pts',(7.95865540215379,-4.8,83.4856865297811));
#36123=CARTESIAN_POINT('Ctrl Pts',(7.95191473077081,-4.8,83.4533858653268));
#36124=CARTESIAN_POINT('Ctrl Pts',(7.94593089663239,-4.8,83.4215841524714));
#36125=CARTESIAN_POINT('Ctrl Pts',(7.94072921137237,-4.8,83.3939392516977));
#36126=CARTESIAN_POINT('Ctrl Pts',(7.93609854851438,-4.8,83.366677578063));
#36127=CARTESIAN_POINT('Ctrl Pts',(7.93203398466726,-4.8,83.3398902206079));
#36128=CARTESIAN_POINT('Ctrl Pts',(7.92872018455444,-4.8,83.3180507437302));
#36129=CARTESIAN_POINT('Ctrl Pts',(7.92578258878329,-4.8,83.2965276961172));
#36130=CARTESIAN_POINT('Ctrl Pts',(7.92322586820198,-4.8,83.2753308935615));
#36131=CARTESIAN_POINT('Ctrl Pts',(7.92042994648818,-4.8,83.2521509649602));
#36132=CARTESIAN_POINT('Ctrl Pts',(7.91809013983445,-4.8,83.2293571253706));
#36133=CARTESIAN_POINT('Ctrl Pts',(7.91622100408708,-4.8,83.2069121607238));
#36134=CARTESIAN_POINT('Ctrl Pts',(7.91483389591844,-4.8,83.1902554819084));
#36135=CARTESIAN_POINT('Ctrl Pts',(7.91370635273902,-4.8,83.1737888114215));
#36136=CARTESIAN_POINT('Ctrl Pts',(7.91284121463069,-4.8,83.1575181559638));
#36137=CARTESIAN_POINT('Ctrl Pts',(7.91205056341829,-4.8,83.1426483758209));
#36138=CARTESIAN_POINT('Ctrl Pts',(7.91147925526362,-4.8,83.1279412476054));
#36139=CARTESIAN_POINT('Ctrl Pts',(7.91112346655007,-4.8,83.1134397531939));
#36140=CARTESIAN_POINT('Ctrl Pts',(7.91076280516985,-4.8,83.0987396551006));
#36141=CARTESIAN_POINT('Ctrl Pts',(7.91062368804623,-4.8,83.0842504621696));
#36142=CARTESIAN_POINT('Ctrl Pts',(7.91069329054054,-4.8,83.0700721479122));
#36143=CARTESIAN_POINT('Ctrl Pts',(7.91079020322715,-4.8,83.0503306351971));
#36144=CARTESIAN_POINT('Ctrl Pts',(7.91129133246646,-4.8,83.0311957414029));
#36145=CARTESIAN_POINT('Ctrl Pts',(7.91214527626044,-4.8,83.0130323541204));
#36146=CARTESIAN_POINT('Ctrl Pts',(7.91278573410593,-4.8,82.9994098136585));
#36147=CARTESIAN_POINT('Ctrl Pts',(7.91362404390535,-4.8,82.9863374951043));
#36148=CARTESIAN_POINT('Ctrl Pts',(7.91463973644661,-4.8,82.9739514147098));
#36149=CARTESIAN_POINT('Ctrl Pts',(7.91562082635049,-4.8,82.9619873035935));
#36150=CARTESIAN_POINT('Ctrl Pts',(7.91676724408405,-4.8,82.9506645129822));
#36151=CARTESIAN_POINT('Ctrl Pts',(7.91806718413429,-4.8,82.9400516840982));
#36152=CARTESIAN_POINT('Ctrl Pts',(7.91955835913016,-4.8,82.9278775957128));
#36153=CARTESIAN_POINT('Ctrl Pts',(7.9212515869683,-4.8,82.9166365258692));
#36154=CARTESIAN_POINT('Ctrl Pts',(7.92313936453975,-4.8,82.9063583729027));
#36155=CARTESIAN_POINT('Ctrl Pts',(7.92471707547372,-4.8,82.8977684020495));
#36156=CARTESIAN_POINT('Ctrl Pts',(7.92643095561883,-4.8,82.8898487215006));
#36157=CARTESIAN_POINT('Ctrl Pts',(7.92828014771505,-4.8,82.8825995361566));
#36158=CARTESIAN_POINT('',(8.09760744867255,-4.8,82.4891652120952));
#36159=CARTESIAN_POINT('',(8.92273797402872,-4.8,80.571963032233));
#36160=CARTESIAN_POINT('',(7.3531668006526,-4.8,82.2182109750381));
#36161=CARTESIAN_POINT('Origin',(9.31000000000056,-4.8,77.9999999999986));
#36162=CARTESIAN_POINT('',(7.22998432988738,-4.8,82.6284406437547));
#36163=CARTESIAN_POINT('',(8.01502518871776,-4.8,80.0140503863876));
#36164=CARTESIAN_POINT('',(6.48377124583839,-4.8,83.2926771136307));
#36165=CARTESIAN_POINT('Ctrl Pts',(7.22998432988738,-4.8,82.6284406437547));
#36166=CARTESIAN_POINT('Ctrl Pts',(7.21078845977609,-4.8,82.6683452043475));
#36167=CARTESIAN_POINT('Ctrl Pts',(7.17576760202974,-4.8,82.7171899164891));
#36168=CARTESIAN_POINT('Ctrl Pts',(7.0570482750219,-4.8,82.867474428743));
#36169=CARTESIAN_POINT('Ctrl Pts',(6.94893456238546,-4.8,82.9689877197435));
#36170=CARTESIAN_POINT('Ctrl Pts',(6.72847521688295,-4.8,83.1415546773667));
#36171=CARTESIAN_POINT('Ctrl Pts',(6.61632946835478,-4.8,83.21724859508));
#36172=CARTESIAN_POINT('Ctrl Pts',(6.48377124583839,-4.8,83.2926771136307));
#36173=CARTESIAN_POINT('',(6.13952154251532,-4.8,83.0939244547427));
#36174=CARTESIAN_POINT('Origin',(9.31,-4.8,78.));
#36175=CARTESIAN_POINT('',(6.34166065765632,-4.8,82.1155667324646));
#36176=CARTESIAN_POINT('Ctrl Pts',(6.13952154251532,-4.8,83.0939244547427));
#36177=CARTESIAN_POINT('Ctrl Pts',(6.13919026958859,-4.8,83.0410810807779));
#36178=CARTESIAN_POINT('Ctrl Pts',(6.14010632566913,-4.8,82.9892450771334));
#36179=CARTESIAN_POINT('Ctrl Pts',(6.14231138803794,-4.8,82.9384642021974));
#36180=CARTESIAN_POINT('Ctrl Pts',(6.144073836074,-4.8,82.8978763918177));
#36181=CARTESIAN_POINT('Ctrl Pts',(6.14666119765675,-4.8,82.8579606997597));
#36182=CARTESIAN_POINT('Ctrl Pts',(6.15007092380639,-4.8,82.8187504318208));
#36183=CARTESIAN_POINT('Ctrl Pts',(6.15280228412168,-4.8,82.7873410560821));
#36184=CARTESIAN_POINT('Ctrl Pts',(6.15606122471426,-4.8,82.7563832370041));
#36185=CARTESIAN_POINT('Ctrl Pts',(6.15982584751516,-4.8,82.7259260380751));
#36186=CARTESIAN_POINT('Ctrl Pts',(6.16393616160808,-4.8,82.6926720679937));
#36187=CARTESIAN_POINT('Ctrl Pts',(6.16864948050054,-4.8,82.6600139264594));
#36188=CARTESIAN_POINT('Ctrl Pts',(6.17390334227212,-4.8,82.62808349967));
#36189=CARTESIAN_POINT('Ctrl Pts',(6.17847046997489,-4.8,82.6003267098853));
#36190=CARTESIAN_POINT('Ctrl Pts',(6.18344311179598,-4.8,82.5731253369718));
#36191=CARTESIAN_POINT('Ctrl Pts',(6.18878548697729,-4.8,82.5465632927227));
#36192=CARTESIAN_POINT('Ctrl Pts',(6.19314107449476,-4.8,82.5249075114561));
#36193=CARTESIAN_POINT('Ctrl Pts',(6.19774195326573,-4.8,82.5036777458914));
#36194=CARTESIAN_POINT('Ctrl Pts',(6.20258915525585,-4.8,82.4828848173746));
#36195=CARTESIAN_POINT('Ctrl Pts',(6.20788985046534,-4.8,82.4601465496472));
#36196=CARTESIAN_POINT('Ctrl Pts',(6.21348710337351,-4.8,82.4379270873797));
#36197=CARTESIAN_POINT('Ctrl Pts',(6.21940731995865,-4.8,82.4161964391848));
#36198=CARTESIAN_POINT('Ctrl Pts',(6.22380078431013,-4.8,82.4000698622588));
#36199=CARTESIAN_POINT('Ctrl Pts',(6.22837317328842,-4.8,82.3842106112069));
#36200=CARTESIAN_POINT('Ctrl Pts',(6.23312510128403,-4.8,82.3686253018486));
#36201=CARTESIAN_POINT('Ctrl Pts',(6.23746789652353,-4.8,82.3543818605864));
#36202=CARTESIAN_POINT('Ctrl Pts',(6.24196117657975,-4.8,82.3403662818851));
#36203=CARTESIAN_POINT('Ctrl Pts',(6.24658664775933,-4.8,82.3266176477455));
#36204=CARTESIAN_POINT('Ctrl Pts',(6.25127546664344,-4.8,82.312680720483));
#36205=CARTESIAN_POINT('Ctrl Pts',(6.25610033521784,-4.8,82.2990177518533));
#36206=CARTESIAN_POINT('Ctrl Pts',(6.2610150093059,-4.8,82.2857182999482));
#36207=CARTESIAN_POINT('Ctrl Pts',(6.26785807237896,-4.8,82.2672004925425));
#36208=CARTESIAN_POINT('Ctrl Pts',(6.27487349885991,-4.8,82.2493909706609));
#36209=CARTESIAN_POINT('Ctrl Pts',(6.28188818776893,-4.8,82.232615035949));
#36210=CARTESIAN_POINT('Ctrl Pts',(6.28714920445069,-4.8,82.220033084915));
#36211=CARTESIAN_POINT('Ctrl Pts',(6.29240795417291,-4.8,82.2080358426923));
#36212=CARTESIAN_POINT('Ctrl Pts',(6.29759868187373,-4.8,82.19674412186));
#36213=CARTESIAN_POINT('Ctrl Pts',(6.30261257180666,-4.8,82.185837087496));
#36214=CARTESIAN_POINT('Ctrl Pts',(6.30756247454736,-4.8,82.1755892427291));
#36215=CARTESIAN_POINT('Ctrl Pts',(6.3124138198641,-4.8,82.1660610514844));
#36216=CARTESIAN_POINT('Ctrl Pts',(6.31797884951121,-4.8,82.1551311622892));
#36217=CARTESIAN_POINT('Ctrl Pts',(6.32341463558439,-4.8,82.1451471298991));
#36218=CARTESIAN_POINT('Ctrl Pts',(6.32870390163747,-4.8,82.1361344833445));
#36219=CARTESIAN_POINT('Ctrl Pts',(6.33312440775988,-4.8,82.128602160547));
#36220=CARTESIAN_POINT('Ctrl Pts',(6.33744361831287,-4.8,82.1217462771392));
#36221=CARTESIAN_POINT('Ctrl Pts',(6.34166065765632,-4.8,82.1155667324646));
#36222=CARTESIAN_POINT('',(6.63533873676839,-4.8,81.8037727491227));
#36223=CARTESIAN_POINT('',(8.06642956697154,-4.8,80.2844032686962));
#36224=CARTESIAN_POINT('',(6.02846516020393,-4.8,81.2945453548562));
#36225=CARTESIAN_POINT('Origin',(9.3100000000004,-4.8,77.9999999999995));
#36226=CARTESIAN_POINT('',(5.77240469132478,-4.8,81.6379042610703));
#36227=CARTESIAN_POINT('',(7.40427592391703,-4.8,79.4496808154216));
#36228=CARTESIAN_POINT('',(4.8440115100785,-4.8,82.006862464309));
#36229=CARTESIAN_POINT('Ctrl Pts',(5.77240469132478,-4.8,81.6379042610703));
#36230=CARTESIAN_POINT('Ctrl Pts',(5.74071830812517,-4.8,81.6688369101196));
#36231=CARTESIAN_POINT('Ctrl Pts',(5.69110358768174,-4.8,81.7027580880799));
#36232=CARTESIAN_POINT('Ctrl Pts',(5.52814358921249,-4.8,81.8033749296924));
#36233=CARTESIAN_POINT('Ctrl Pts',(5.39183034107398,-4.8,81.8617891528896));
#36234=CARTESIAN_POINT('Ctrl Pts',(5.12564494391121,-4.8,81.9485475132162));
#36235=CARTESIAN_POINT('Ctrl Pts',(4.99437356661556,-4.8,81.9813204242451));
#36236=CARTESIAN_POINT('Ctrl Pts',(4.8440115100785,-4.8,82.006862464309));
#36237=CARTESIAN_POINT('',(4.58850001701745,-4.8,81.7023557244943));
#36238=CARTESIAN_POINT('Origin',(9.31,-4.8,78.));
#36239=CARTESIAN_POINT('',(5.11306670030725,-4.8,80.8521358415414));
#36240=CARTESIAN_POINT('Ctrl Pts',(4.58850001701745,-4.8,81.7023557244943));
#36241=CARTESIAN_POINT('Ctrl Pts',(4.60626222063291,-4.8,81.6525858939099));
#36242=CARTESIAN_POINT('Ctrl Pts',(4.62485198918894,-4.8,81.6041892934237));
#36243=CARTESIAN_POINT('Ctrl Pts',(4.6442921521603,-4.8,81.5572250557159));
#36244=CARTESIAN_POINT('Ctrl Pts',(4.65983016136228,-4.8,81.5196877799871));
#36245=CARTESIAN_POINT('Ctrl Pts',(4.67591345780073,-4.8,81.4830642260602));
#36246=CARTESIAN_POINT('Ctrl Pts',(4.69252825496127,-4.8,81.4473848193518));
#36247=CARTESIAN_POINT('Ctrl Pts',(4.70583753319529,-4.8,81.4188038414128));
#36248=CARTESIAN_POINT('Ctrl Pts',(4.71948813323713,-4.8,81.3908276310071));
#36249=CARTESIAN_POINT('Ctrl Pts',(4.73344269693336,-4.8,81.3634948031522));
#36250=CARTESIAN_POINT('Ctrl Pts',(4.74867865634235,-4.8,81.3336521033162));
#36251=CARTESIAN_POINT('Ctrl Pts',(4.76427746953913,-4.8,81.3045755389547));
#36252=CARTESIAN_POINT('Ctrl Pts',(4.78013533378095,-4.8,81.2763676793213));
#36253=CARTESIAN_POINT('Ctrl Pts',(4.79392041110474,-4.8,81.2518468787736));
#36254=CARTESIAN_POINT('Ctrl Pts',(4.8078965832873,-4.8,81.2279866933517));
#36255=CARTESIAN_POINT('Ctrl Pts',(4.82200152789346,-4.8,81.2048537366049));
#36256=CARTESIAN_POINT('Ctrl Pts',(4.8335011546974,-4.8,81.1859936576122));
#36257=CARTESIAN_POINT('Ctrl Pts',(4.84508557392789,-4.8,81.1676177969763));
#36258=CARTESIAN_POINT('Ctrl Pts',(4.85675205419961,-4.8,81.1497366763869));
#36259=CARTESIAN_POINT('Ctrl Pts',(4.86951002346223,-4.8,81.1301826393895));
#36260=CARTESIAN_POINT('Ctrl Pts',(4.88236922388144,-4.8,81.1112175487126));
#36261=CARTESIAN_POINT('Ctrl Pts',(4.89536472661568,-4.8,81.0928222530497));
#36262=CARTESIAN_POINT('Ctrl Pts',(4.90500884676139,-4.8,81.0791708811008));
#36263=CARTESIAN_POINT('Ctrl Pts',(4.91472967022465,-4.8,81.0658319091268));
#36264=CARTESIAN_POINT('Ctrl Pts',(4.92452551159968,-4.8,81.0528117640994));
#36265=CARTESIAN_POINT('Ctrl Pts',(4.93347794805258,-4.8,81.0409126309364));
#36266=CARTESIAN_POINT('Ctrl Pts',(4.94249386039137,-4.8,81.0292790873789));
#36267=CARTESIAN_POINT('Ctrl Pts',(4.95154269133482,-4.8,81.0179416016839));
#36268=CARTESIAN_POINT('Ctrl Pts',(4.96071544974391,-4.8,81.0064488444541));
#36269=CARTESIAN_POINT('Ctrl Pts',(4.96992235367127,-4.8,80.9952600558691));
#36270=CARTESIAN_POINT('Ctrl Pts',(4.97908931713115,-4.8,80.9844435765684));
#36271=CARTESIAN_POINT('Ctrl Pts',(4.99185315606398,-4.8,80.9693829951428));
#36272=CARTESIAN_POINT('Ctrl Pts',(5.00453671569697,-4.8,80.9550469361515));
#36273=CARTESIAN_POINT('Ctrl Pts',(5.01686607460425,-4.8,80.9416818791236));
#36274=CARTESIAN_POINT('Ctrl Pts',(5.02611309378471,-4.8,80.9316580863527));
#36275=CARTESIAN_POINT('Ctrl Pts',(5.03515800052709,-4.8,80.9221829647861));
#36276=CARTESIAN_POINT('Ctrl Pts',(5.04389768495218,-4.8,80.913347551555));
#36277=CARTESIAN_POINT('Ctrl Pts',(5.05233962579543,-4.8,80.9048131431948));
#36278=CARTESIAN_POINT('Ctrl Pts',(5.06049598222156,-4.8,80.8968762855306));
#36279=CARTESIAN_POINT('Ctrl Pts',(5.06831358896028,-4.8,80.8895819723517));
#36280=CARTESIAN_POINT('Ctrl Pts',(5.07728124855712,-4.8,80.8812145883469));
#36281=CARTESIAN_POINT('Ctrl Pts',(5.08580395683557,-4.8,80.8736918151081));
#36282=CARTESIAN_POINT('Ctrl Pts',(5.09385674780709,-4.8,80.8670317331858));
#36283=CARTESIAN_POINT('Ctrl Pts',(5.10058687068216,-4.8,80.8614655673864));
#36284=CARTESIAN_POINT('Ctrl Pts',(5.10699045098391,-4.8,80.8565004015291));
#36285=CARTESIAN_POINT('Ctrl Pts',(5.11306670030725,-4.8,80.8521358415414));
#36286=CARTESIAN_POINT('',(5.49567364700612,-4.8,80.659589154899));
#36287=CARTESIAN_POINT('',(7.36011410728251,-4.8,79.721310756753));
#36288=CARTESIAN_POINT('',(5.09956505173093,-4.8,79.9735089425676));
#36289=CARTESIAN_POINT('Origin',(9.30999999999911,-4.8,78.0000000000005));
#36290=CARTESIAN_POINT('',(4.7415112563347,-4.8,80.2085829347521));
#36291=CARTESIAN_POINT('',(7.02338510818378,-4.8,78.7104583431054));
#36292=CARTESIAN_POINT('',(3.74291589718234,-4.8,80.2377610668154));
#36293=CARTESIAN_POINT('Ctrl Pts',(4.7415112563347,-4.8,80.2085829347521));
#36294=CARTESIAN_POINT('Ctrl Pts',(4.7011562116549,-4.8,80.2268127331602));
#36295=CARTESIAN_POINT('Ctrl Pts',(4.6429319051249,-4.8,80.2417189802796));
#36296=CARTESIAN_POINT('Ctrl Pts',(4.45538659248291,-4.8,80.2805322845508));
#36297=CARTESIAN_POINT('Ctrl Pts',(4.30731519855239,-4.8,80.2888018217475));
#36298=CARTESIAN_POINT('Ctrl Pts',(4.02750964186796,-4.8,80.2792872446601));
#36299=CARTESIAN_POINT('Ctrl Pts',(3.89294590272478,-4.8,80.2651862520695));
#36300=CARTESIAN_POINT('Ctrl Pts',(3.74291589718234,-4.8,80.2377610668154));
#36301=CARTESIAN_POINT('',(3.60696107140887,-4.8,79.8642282529171));
#36302=CARTESIAN_POINT('Origin',(9.31,-4.8,78.));
#36303=CARTESIAN_POINT('',(4.39068483903982,-4.8,79.2446952750862));
#36304=CARTESIAN_POINT('Ctrl Pts',(3.60696107140887,-4.8,79.8642282529171));
#36305=CARTESIAN_POINT('Ctrl Pts',(3.64067436766681,-4.8,79.8235349418069));
#36306=CARTESIAN_POINT('Ctrl Pts',(3.67469564825235,-4.8,79.7844150887646));
#36307=CARTESIAN_POINT('Ctrl Pts',(3.70902614126382,-4.8,79.7469320684765));
#36308=CARTESIAN_POINT('Ctrl Pts',(3.73646559938461,-4.8,79.7169728784033));
#36309=CARTESIAN_POINT('Ctrl Pts',(3.76410494864752,-4.8,79.6880588052678));
#36310=CARTESIAN_POINT('Ctrl Pts',(3.79192082785855,-4.8,79.6602137243463));
#36311=CARTESIAN_POINT('Ctrl Pts',(3.81420272833821,-4.8,79.6379084318465));
#36312=CARTESIAN_POINT('Ctrl Pts',(3.83659852371768,-4.8,79.6162881738544));
#36313=CARTESIAN_POINT('Ctrl Pts',(3.85905990170427,-4.8,79.5953764593762));
#36314=CARTESIAN_POINT('Ctrl Pts',(3.88358382496445,-4.8,79.5725444994933));
#36315=CARTESIAN_POINT('Ctrl Pts',(3.90818668548508,-4.8,79.5505565747794));
#36316=CARTESIAN_POINT('Ctrl Pts',(3.93273585983976,-4.8,79.5294735661781));
#36317=CARTESIAN_POINT('Ctrl Pts',(3.95407620286161,-4.8,79.5111463251481));
#36318=CARTESIAN_POINT('Ctrl Pts',(3.97537017262871,-4.8,79.4935052175616));
#36319=CARTESIAN_POINT('Ctrl Pts',(3.99653642203519,-4.8,79.47659152415));
#36320=CARTESIAN_POINT('Ctrl Pts',(4.01379306328134,-4.8,79.4628019512433));
#36321=CARTESIAN_POINT('Ctrl Pts',(4.03096377091259,-4.8,79.4494963954657));
#36322=CARTESIAN_POINT('Ctrl Pts',(4.04804237963872,-4.8,79.4366838097816));
#36323=CARTESIAN_POINT('Ctrl Pts',(4.0667188232732,-4.8,79.4226725083823));
#36324=CARTESIAN_POINT('Ctrl Pts',(4.08528896157969,-4.8,79.4092492585601));
#36325=CARTESIAN_POINT('Ctrl Pts',(4.10379230079774,-4.8,79.3964080590159));
#36326=CARTESIAN_POINT('Ctrl Pts',(4.11752385348229,-4.8,79.3868784489279));
#36327=CARTESIAN_POINT('Ctrl Pts',(4.13122063662477,-4.8,79.377668632869));
#36328=CARTESIAN_POINT('Ctrl Pts',(4.14487886830775,-4.8,79.3687840737741));
#36329=CARTESIAN_POINT('Ctrl Pts',(4.15736114997002,-4.8,79.3606644597829));
#36330=CARTESIAN_POINT('Ctrl Pts',(4.1698122424592,-4.8,79.3528161284141));
#36331=CARTESIAN_POINT('Ctrl Pts',(4.18219301056543,-4.8,79.3452572592584));
#36332=CARTESIAN_POINT('Ctrl Pts',(4.19474333843089,-4.8,79.3375948682515));
#36333=CARTESIAN_POINT('Ctrl Pts',(4.20722178918766,-4.8,79.3302297927924));
#36334=CARTESIAN_POINT('Ctrl Pts',(4.21953537090469,-4.8,79.3232009131774));
#36335=CARTESIAN_POINT('Ctrl Pts',(4.2366804783172,-4.8,79.3134140860169));
#36336=CARTESIAN_POINT('Ctrl Pts',(4.25350234659464,-4.8,79.3042806301018));
#36337=CARTESIAN_POINT('Ctrl Pts',(4.26965927283183,-4.8,79.2959384737804));
#36338=CARTESIAN_POINT('Ctrl Pts',(4.28177696750972,-4.8,79.2896818565394));
#36339=CARTESIAN_POINT('Ctrl Pts',(4.29351708201629,-4.8,79.2838716950536));
#36340=CARTESIAN_POINT('Ctrl Pts',(4.30475158822826,-4.8,79.2785582705871));
#36341=CARTESIAN_POINT('Ctrl Pts',(4.31560335725497,-4.8,79.2734258638783));
#36342=CARTESIAN_POINT('Ctrl Pts',(4.32598239033975,-4.8,79.2687572955227));
#36343=CARTESIAN_POINT('Ctrl Pts',(4.33582333969107,-4.8,79.2645766622574));
#36344=CARTESIAN_POINT('Ctrl Pts',(4.34711199719151,-4.8,79.2597810134453));
#36345=CARTESIAN_POINT('Ctrl Pts',(4.35769366331604,-4.8,79.2556268568332));
#36346=CARTESIAN_POINT('Ctrl Pts',(4.36753869379978,-4.8,79.2521226437087));
#36347=CARTESIAN_POINT('Ctrl Pts',(4.3757666812864,-4.8,79.2491939964296));
#36348=CARTESIAN_POINT('Ctrl Pts',(4.38348226505871,-4.8,79.246718420208));
#36349=CARTESIAN_POINT('Ctrl Pts',(4.39068483903982,-4.8,79.2446952750862));
#36350=CARTESIAN_POINT('',(4.81607260887647,-4.8,79.194619857239));
#36351=CARTESIAN_POINT('',(6.88898366350615,-4.8,78.9506027637043));
#36352=CARTESIAN_POINT('',(4.67850553742098,-4.8,78.4144382259154));
#36353=CARTESIAN_POINT('Origin',(9.31000000000016,-4.8,78.));
#36354=CARTESIAN_POINT('',(6.91829379524532,-4.8,77.8855441093625));
#36355=CARTESIAN_POINT('Origin',(9.31,-9.325,78.));
#36356=CARTESIAN_POINT('',(3.06,-13.85,78.));
#36357=CARTESIAN_POINT('Origin',(9.31,-13.85,78.));
#36358=CARTESIAN_POINT('',(3.06,-9.325,78.));
#36359=CARTESIAN_POINT('Origin',(9.31,4.875,78.));
#36360=CARTESIAN_POINT('',(15.41,4.8,78.));
#36361=CARTESIAN_POINT('Origin',(9.31,4.8,78.));
#36362=CARTESIAN_POINT('',(15.56,4.95,78.));
#36363=CARTESIAN_POINT('',(15.485,4.875,78.));
#36364=CARTESIAN_POINT('',(3.06,4.95,78.));
#36365=CARTESIAN_POINT('Origin',(9.31,4.95,78.));
#36366=CARTESIAN_POINT('Origin',(9.31,4.95,78.));
#36367=CARTESIAN_POINT('Origin',(9.31,4.8,78.));
#36368=CARTESIAN_POINT('',(3.31329278848646,4.8,78.1987526588035));
#36369=CARTESIAN_POINT('',(4.2616449875437,4.8,78.5128739112901));
#36370=CARTESIAN_POINT('Ctrl Pts',(3.31329278848646,4.8,78.1987526588035));
#36371=CARTESIAN_POINT('Ctrl Pts',(3.35889085630227,4.8,78.2254612365697));
#36372=CARTESIAN_POINT('Ctrl Pts',(3.40424018037907,4.8,78.2505859106759));
#36373=CARTESIAN_POINT('Ctrl Pts',(3.44932023930959,4.8,78.2740667081797));
#36374=CARTESIAN_POINT('Ctrl Pts',(3.48535154078234,4.8,78.2928342899832));
#36375=CARTESIAN_POINT('Ctrl Pts',(3.52121322744871,4.8,78.3105514163533));
#36376=CARTESIAN_POINT('Ctrl Pts',(3.55687518114691,4.8,78.3272036418769));
#36377=CARTESIAN_POINT('Ctrl Pts',(3.58544217793619,4.8,78.3405429018931));
#36378=CARTESIAN_POINT('Ctrl Pts',(3.61388190532127,4.8,78.3531994856718));
#36379=CARTESIAN_POINT('Ctrl Pts',(3.64214092404874,4.8,78.3651678257731));
#36380=CARTESIAN_POINT('Ctrl Pts',(3.67299486093853,4.8,78.3782351730056));
#36381=CARTESIAN_POINT('Ctrl Pts',(3.70363429760745,4.8,78.3904823886558));
#36382=CARTESIAN_POINT('Ctrl Pts',(3.73391378633966,4.8,78.4018976232415));
#36383=CARTESIAN_POINT('Ctrl Pts',(3.7602354354294,4.8,78.4118207696229));
#36384=CARTESIAN_POINT('Ctrl Pts',(3.7862788364629,4.8,78.4211150220416));
#36385=CARTESIAN_POINT('Ctrl Pts',(3.81195342930972,4.8,78.4297694116381));
#36386=CARTESIAN_POINT('Ctrl Pts',(3.83288567961382,4.8,78.4368252528094));
#36387=CARTESIAN_POINT('Ctrl Pts',(3.85357163513014,4.8,78.4434556576798));
#36388=CARTESIAN_POINT('Ctrl Pts',(3.87400244027753,4.8,78.449654321866));
#36389=CARTESIAN_POINT('Ctrl Pts',(3.89634470605425,4.8,78.4564329192688));
#36390=CARTESIAN_POINT('Ctrl Pts',(3.91838595195131,4.8,78.4626952874073));
#36391=CARTESIAN_POINT('Ctrl Pts',(3.94016535426666,4.8,78.468433553731));
#36392=CARTESIAN_POINT('Ctrl Pts',(3.95632811179584,4.8,78.4726919904816));
#36393=CARTESIAN_POINT('Ctrl Pts',(3.97234882063946,4.8,78.4766618110219));
#36394=CARTESIAN_POINT('Ctrl Pts',(3.98822205852683,4.8,78.4803391753661));
#36395=CARTESIAN_POINT('Ctrl Pts',(4.00272863804244,4.8,78.4836999249904));
#36396=CARTESIAN_POINT('Ctrl Pts',(4.01711312520302,4.8,78.4868164196652));
#36397=CARTESIAN_POINT('Ctrl Pts',(4.03133252715836,4.8,78.4896849611932));
#36398=CARTESIAN_POINT('Ctrl Pts',(4.04574666952095,4.8,78.4925927885468));
#36399=CARTESIAN_POINT('Ctrl Pts',(4.05999158159986,4.8,78.4952458141038));
#36400=CARTESIAN_POINT('Ctrl Pts',(4.073966581728,4.8,78.4976393074474));
#36401=CARTESIAN_POINT('Ctrl Pts',(4.09342500507885,4.8,78.5009719447526));
#36402=CARTESIAN_POINT('Ctrl Pts',(4.11235621687838,4.8,78.5038011681971));
#36403=CARTESIAN_POINT('Ctrl Pts',(4.13039194713631,4.8,78.5061142367954));
#36404=CARTESIAN_POINT('Ctrl Pts',(4.14391874482975,4.8,78.5078490382441));
#36405=CARTESIAN_POINT('Ctrl Pts',(4.15693803635337,4.8,78.5092934485219));
#36406=CARTESIAN_POINT('Ctrl Pts',(4.16931231741,4.8,78.510444006894));
#36407=CARTESIAN_POINT('Ctrl Pts',(4.1812650311382,4.8,78.5115553680136));
#36408=CARTESIAN_POINT('Ctrl Pts',(4.19261487634346,4.8,78.512392548869));
#36409=CARTESIAN_POINT('Ctrl Pts',(4.20329220461838,4.8,78.5129552562033));
#36410=CARTESIAN_POINT('Ctrl Pts',(4.21554028124679,4.8,78.513600743761));
#36411=CARTESIAN_POINT('Ctrl Pts',(4.22690460006138,4.8,78.513885231135));
#36412=CARTESIAN_POINT('Ctrl Pts',(4.23735441405482,4.8,78.5138109156641));
#36413=CARTESIAN_POINT('Ctrl Pts',(4.24608785027474,4.8,78.5137488064796));
#36414=CARTESIAN_POINT('Ctrl Pts',(4.25418482498679,4.8,78.5134362021356));
#36415=CARTESIAN_POINT('Ctrl Pts',(4.2616449875437,4.8,78.5128739112901));
#36416=CARTESIAN_POINT('',(4.67850553742098,4.8,78.4144382259154));
#36417=CARTESIAN_POINT('',(6.91829379524532,4.8,77.8855441093625));
#36418=CARTESIAN_POINT('',(4.81607260887647,4.8,79.194619857239));
#36419=CARTESIAN_POINT('Origin',(9.31000000000016,4.8,78.));
#36420=CARTESIAN_POINT('',(4.39068483903982,4.8,79.2446952750862));
#36421=CARTESIAN_POINT('',(6.88898366350615,4.8,78.9506027637043));
#36422=CARTESIAN_POINT('',(3.60696107140888,4.8,79.8642282529171));
#36423=CARTESIAN_POINT('Ctrl Pts',(4.39068483903982,4.8,79.2446952750862));
#36424=CARTESIAN_POINT('Ctrl Pts',(4.34805318204033,4.8,79.256670164774));
#36425=CARTESIAN_POINT('Ctrl Pts',(4.29386921508062,4.8,79.2826771886758));
#36426=CARTESIAN_POINT('Ctrl Pts',(4.12525249151527,4.8,79.3734962560852));
#36427=CARTESIAN_POINT('Ctrl Pts',(4.00650766503333,4.8,79.4623398804252));
#36428=CARTESIAN_POINT('Ctrl Pts',(3.79828002278047,4.8,79.6494840153308));
#36429=CARTESIAN_POINT('Ctrl Pts',(3.70426215728068,4.8,79.7467819098348));
#36430=CARTESIAN_POINT('Ctrl Pts',(3.60696107140887,4.8,79.8642282529171));
#36431=CARTESIAN_POINT('',(3.74291589718233,4.8,80.2377610668154));
#36432=CARTESIAN_POINT('Origin',(9.31,4.8,78.));
#36433=CARTESIAN_POINT('',(4.7415112563347,4.8,80.2085829347521));
#36434=CARTESIAN_POINT('Ctrl Pts',(3.74291589718233,4.8,80.2377610668154));
#36435=CARTESIAN_POINT('Ctrl Pts',(3.79489893662468,4.8,80.2472634625638));
#36436=CARTESIAN_POINT('Ctrl Pts',(3.8461065064291,4.8,80.2553625510896));
#36437=CARTESIAN_POINT('Ctrl Pts',(3.89649881086473,4.8,80.2620089950116));
#36438=CARTESIAN_POINT('Ctrl Pts',(3.93677604781892,4.8,80.2673213219581));
#36439=CARTESIAN_POINT('Ctrl Pts',(3.97653462213701,4.8,80.271704555469));
#36440=CARTESIAN_POINT('Ctrl Pts',(4.01574129138727,4.8,80.275155422314));
#36441=CARTESIAN_POINT('Ctrl Pts',(4.04714778360346,4.8,80.2779197383036));
#36442=CARTESIAN_POINT('Ctrl Pts',(4.07820119267025,4.8,80.280086077154));
#36443=CARTESIAN_POINT('Ctrl Pts',(4.10884939793472,4.8,80.281667484482));
#36444=CARTESIAN_POINT('Ctrl Pts',(4.14231191142195,4.8,80.2833941064353));
#36445=CARTESIAN_POINT('Ctrl Pts',(4.17529235909806,4.8,80.2844234201605));
#36446=CARTESIAN_POINT('Ctrl Pts',(4.20765001204969,4.8,80.2847940368353));
#36447=CARTESIAN_POINT('Ctrl Pts',(4.23577818756272,4.8,80.2851162101058));
#36448=CARTESIAN_POINT('Ctrl Pts',(4.26342980102536,4.8,80.2849425827943));
#36449=CARTESIAN_POINT('Ctrl Pts',(4.29051600217998,4.8,80.2842938209344));
#36450=CARTESIAN_POINT('Ctrl Pts',(4.3125991233526,4.8,80.2837648915846));
#36451=CARTESIAN_POINT('Ctrl Pts',(4.33430529534107,4.8,80.2829204206548));
#36452=CARTESIAN_POINT('Ctrl Pts',(4.3556240403936,4.8,80.2817575127505));
#36453=CARTESIAN_POINT('Ctrl Pts',(4.3789373199094,4.8,80.2804858057641));
#36454=CARTESIAN_POINT('Ctrl Pts',(4.40179117244473,4.8,80.2788319567986));
#36455=CARTESIAN_POINT('Ctrl Pts',(4.42421971910711,4.8,80.2767751689934));
#36456=CARTESIAN_POINT('Ctrl Pts',(4.44086421427025,4.8,80.2752488019402));
#36457=CARTESIAN_POINT('Ctrl Pts',(4.457276514773,4.8,80.2734998078755));
#36458=CARTESIAN_POINT('Ctrl Pts',(4.47345021199511,4.8,80.271526432919));
#36459=CARTESIAN_POINT('Ctrl Pts',(4.48823138184513,4.8,80.2697229621349));
#36460=CARTESIAN_POINT('Ctrl Pts',(4.50281428229542,4.8,80.267731724821));
#36461=CARTESIAN_POINT('Ctrl Pts',(4.51715724842402,4.8,80.2655639502292));
#36462=CARTESIAN_POINT('Ctrl Pts',(4.53169664720218,4.8,80.2633664870985));
#36463=CARTESIAN_POINT('Ctrl Pts',(4.54598987418342,4.8,80.2609874687648));
#36464=CARTESIAN_POINT('Ctrl Pts',(4.5599407016508,4.8,80.2584568852483));
#36465=CARTESIAN_POINT('Ctrl Pts',(4.57936546759993,4.8,80.254933367189));
#36466=CARTESIAN_POINT('Ctrl Pts',(4.59812263906443,4.8,80.2511171118083));
#36467=CARTESIAN_POINT('Ctrl Pts',(4.61586179777949,4.8,80.2471221022498));
#36468=CARTESIAN_POINT('Ctrl Pts',(4.62916616681578,4.8,80.2441258450809));
#36469=CARTESIAN_POINT('Ctrl Pts',(4.64189431642035,4.8,80.2410302868029));
#36470=CARTESIAN_POINT('Ctrl Pts',(4.65391585117796,4.8,80.2378792046286));
#36471=CARTESIAN_POINT('Ctrl Pts',(4.66552783602353,4.8,80.2348354735915));
#36472=CARTESIAN_POINT('Ctrl Pts',(4.67647953458823,4.8,80.2317402905604));
#36473=CARTESIAN_POINT('Ctrl Pts',(4.68670539847485,4.8,80.228617201124));
#36474=CARTESIAN_POINT('Ctrl Pts',(4.69843559535106,4.8,80.2250346721214));
#36475=CARTESIAN_POINT('Ctrl Pts',(4.70921186221142,4.8,80.2214151768855));
#36476=CARTESIAN_POINT('Ctrl Pts',(4.71900605785115,4.8,80.2177712963384));
#36477=CARTESIAN_POINT('Ctrl Pts',(4.72719156090807,4.8,80.2147259216641));
#36478=CARTESIAN_POINT('Ctrl Pts',(4.73469331137732,4.8,80.2116628411954));
#36479=CARTESIAN_POINT('Ctrl Pts',(4.7415112563347,4.8,80.2085829347521));
#36480=CARTESIAN_POINT('',(5.09956505173093,4.8,79.9735089425676));
#36481=CARTESIAN_POINT('',(7.02338510818378,4.8,78.7104583431054));
#36482=CARTESIAN_POINT('',(5.49567364700612,4.8,80.659589154899));
#36483=CARTESIAN_POINT('Origin',(9.30999999999911,4.8,78.0000000000005));
#36484=CARTESIAN_POINT('',(5.11306670030725,4.8,80.8521358415414));
#36485=CARTESIAN_POINT('',(7.36011410728251,4.8,79.721310756753));
#36486=CARTESIAN_POINT('',(4.58850001701745,4.8,81.7023557244943));
#36487=CARTESIAN_POINT('Ctrl Pts',(5.11306670030725,4.8,80.8521358415414));
#36488=CARTESIAN_POINT('Ctrl Pts',(5.07710170065269,4.8,80.8779694421884));
#36489=CARTESIAN_POINT('Ctrl Pts',(5.03508035307228,4.8,80.9209400583674));
#36490=CARTESIAN_POINT('Ctrl Pts',(4.90769441223799,4.8,81.0639523820827));
#36491=CARTESIAN_POINT('Ctrl Pts',(4.82649708410344,4.8,81.1880512030074));
#36492=CARTESIAN_POINT('Ctrl Pts',(4.69483416885232,4.8,81.4351272139253));
#36493=CARTESIAN_POINT('Ctrl Pts',(4.63976411435854,4.8,81.5587133310751));
#36494=CARTESIAN_POINT('Ctrl Pts',(4.58850001701746,4.8,81.7023557244943));
#36495=CARTESIAN_POINT('',(4.8440115100785,4.8,82.006862464309));
#36496=CARTESIAN_POINT('Origin',(9.31,4.8,78.));
#36497=CARTESIAN_POINT('',(5.77240469132478,4.8,81.6379042610703));
#36498=CARTESIAN_POINT('Ctrl Pts',(4.84401151007851,4.8,82.0068624643091));
#36499=CARTESIAN_POINT('Ctrl Pts',(4.89610959940387,4.8,81.9980125488754));
#36500=CARTESIAN_POINT('Ctrl Pts',(4.94699902627575,4.8,81.988109182246));
#36501=CARTESIAN_POINT('Ctrl Pts',(4.99662552059134,4.8,81.9771196133745));
#36502=CARTESIAN_POINT('Ctrl Pts',(5.03629066414916,4.8,81.9683359418108));
#36503=CARTESIAN_POINT('Ctrl Pts',(5.07515065565679,4.8,81.9588566011248));
#36504=CARTESIAN_POINT('Ctrl Pts',(5.11317313793904,4.8,81.9486898850655));
#36505=CARTESIAN_POINT('Ctrl Pts',(5.14363103907588,4.8,81.9405458393843));
#36506=CARTESIAN_POINT('Ctrl Pts',(5.17355263034768,4.8,81.931960640535));
#36507=CARTESIAN_POINT('Ctrl Pts',(5.20289339622169,4.8,81.9229643737014));
#36508=CARTESIAN_POINT('Ctrl Pts',(5.23492841319329,4.8,81.9131420138512));
#36509=CARTESIAN_POINT('Ctrl Pts',(5.26627194300247,4.8,81.9028292748064));
#36510=CARTESIAN_POINT('Ctrl Pts',(5.29680494952465,4.8,81.8921105713328));
#36511=CARTESIAN_POINT('Ctrl Pts',(5.32334697835746,4.8,81.8827929125414));
#36512=CARTESIAN_POINT('Ctrl Pts',(5.34927161155919,4.8,81.8731723474198));
#36513=CARTESIAN_POINT('Ctrl Pts',(5.37450242539821,4.8,81.863298684267));
#36514=CARTESIAN_POINT('Ctrl Pts',(5.39507286694955,4.8,81.8552487809988));
#36515=CARTESIAN_POINT('Ctrl Pts',(5.41518117055855,4.8,81.847031289851));
#36516=CARTESIAN_POINT('Ctrl Pts',(5.4348165000751,4.8,81.838647073645));
#36517=CARTESIAN_POINT('Ctrl Pts',(5.45628886765119,4.8,81.8294784486897));
#36518=CARTESIAN_POINT('Ctrl Pts',(5.47719881481788,4.8,81.8201078610154));
#36519=CARTESIAN_POINT('Ctrl Pts',(5.49757129198245,4.8,81.810504097856));
#36520=CARTESIAN_POINT('Ctrl Pts',(5.5126899530357,4.8,81.803377029367));
#36521=CARTESIAN_POINT('Ctrl Pts',(5.52751427955579,4.8,81.7961201751675));
#36522=CARTESIAN_POINT('Ctrl Pts',(5.54203764954719,4.8,81.7887340790253));
#36523=CARTESIAN_POINT('Ctrl Pts',(5.55531058243868,4.8,81.7819839130181));
#36524=CARTESIAN_POINT('Ctrl Pts',(5.56833298310324,4.8,81.7751251163156));
#36525=CARTESIAN_POINT('Ctrl Pts',(5.58106953995245,4.8,81.7681824912052));
#36526=CARTESIAN_POINT('Ctrl Pts',(5.59398052898341,4.8,81.761144784099));
#36527=CARTESIAN_POINT('Ctrl Pts',(5.60659809666052,4.8,81.7540206666206));
#36528=CARTESIAN_POINT('Ctrl Pts',(5.6188420757021,4.8,81.7468712319881));
#36529=CARTESIAN_POINT('Ctrl Pts',(5.63589027087475,4.8,81.7369165467854));
#36530=CARTESIAN_POINT('Ctrl Pts',(5.65221101037482,4.8,81.7269151092405));
#36531=CARTESIAN_POINT('Ctrl Pts',(5.6675139932742,4.8,81.7170938785846));
#36532=CARTESIAN_POINT('Ctrl Pts',(5.67899123044873,4.8,81.7097279555928));
#36533=CARTESIAN_POINT('Ctrl Pts',(5.68989303549415,4.8,81.7024657987365));
#36534=CARTESIAN_POINT('Ctrl Pts',(5.70011184948736,4.8,81.6953931429993));
#36535=CARTESIAN_POINT('Ctrl Pts',(5.70998252861731,4.8,81.6885614387111));
#36536=CARTESIAN_POINT('Ctrl Pts',(5.71921514399013,4.8,81.6819072165723));
#36537=CARTESIAN_POINT('Ctrl Pts',(5.72775615332453,4.8,81.6754750210674));
#36538=CARTESIAN_POINT('Ctrl Pts',(5.7375536356891,4.8,81.6680965814056));
#36539=CARTESIAN_POINT('Ctrl Pts',(5.74644207386582,4.8,81.6610096681232));
#36540=CARTESIAN_POINT('Ctrl Pts',(5.75439932669715,4.8,81.6542357282713));
#36541=CARTESIAN_POINT('Ctrl Pts',(5.76104960421005,4.8,81.6485744050953));
#36542=CARTESIAN_POINT('Ctrl Pts',(5.7670513086917,4.8,81.6431303010753));
#36543=CARTESIAN_POINT('Ctrl Pts',(5.77240469132478,4.8,81.6379042610703));
#36544=CARTESIAN_POINT('',(6.02846516020393,4.8,81.2945453548562));
#36545=CARTESIAN_POINT('',(7.40427592391703,4.8,79.4496808154216));
#36546=CARTESIAN_POINT('',(6.63533873676839,4.8,81.8037727491227));
#36547=CARTESIAN_POINT('Origin',(9.3100000000004,4.8,77.9999999999995));
#36548=CARTESIAN_POINT('',(6.34166065765632,4.8,82.1155667324646));
#36549=CARTESIAN_POINT('',(8.06642956697154,4.8,80.2844032686962));
#36550=CARTESIAN_POINT('',(6.13952154251532,4.8,83.0939244547427));
#36551=CARTESIAN_POINT('Ctrl Pts',(6.34166065765632,4.8,82.1155667324646));
#36552=CARTESIAN_POINT('Ctrl Pts',(6.31670022593569,4.8,82.1521431289251));
#36553=CARTESIAN_POINT('Ctrl Pts',(6.29190989233962,4.8,82.2068944446312));
#36554=CARTESIAN_POINT('Ctrl Pts',(6.22111935694833,4.8,82.3848506343714));
#36555=CARTESIAN_POINT('Ctrl Pts',(6.18726312363742,4.8,82.5292365021937));
#36556=CARTESIAN_POINT('Ctrl Pts',(6.14804542664426,4.8,82.8064433752316));
#36557=CARTESIAN_POINT('Ctrl Pts',(6.13856544450829,4.8,82.9414114044585));
#36558=CARTESIAN_POINT('Ctrl Pts',(6.13952154251532,4.8,83.0939244547427));
#36559=CARTESIAN_POINT('',(6.48377124583838,4.8,83.2926771136307));
#36560=CARTESIAN_POINT('Origin',(9.31,4.8,78.));
#36561=CARTESIAN_POINT('',(7.22998432988738,4.8,82.6284406437547));
#36562=CARTESIAN_POINT('Ctrl Pts',(6.48377124583838,4.8,83.2926771136307));
#36563=CARTESIAN_POINT('Ctrl Pts',(6.52970058658809,4.8,83.2665423174258));
#36564=CARTESIAN_POINT('Ctrl Pts',(6.57413385459844,4.8,83.2398309878224));
#36565=CARTESIAN_POINT('Ctrl Pts',(6.61700885117049,4.8,83.2125309103563));
#36566=CARTESIAN_POINT('Ctrl Pts',(6.65127769902839,4.8,83.1907106823448));
#36567=CARTESIAN_POINT('Ctrl Pts',(6.68455201872959,4.8,83.1685121174579));
#36568=CARTESIAN_POINT('Ctrl Pts',(6.71680424110902,4.8,83.1459540760717));
#36569=CARTESIAN_POINT('Ctrl Pts',(6.74263987891727,4.8,83.1278839604665));
#36570=CARTESIAN_POINT('Ctrl Pts',(6.767820667016,4.8,83.1095827252503));
#36571=CARTESIAN_POINT('Ctrl Pts',(6.79231506422289,4.8,83.0910938664587));
#36572=CARTESIAN_POINT('Ctrl Pts',(6.81905868866002,4.8,83.0709072461628));
#36573=CARTESIAN_POINT('Ctrl Pts',(6.84498480814072,4.8,83.0504963226871));
#36574=CARTESIAN_POINT('Ctrl Pts',(6.87001043684679,4.8,83.0299811327162));
#36575=CARTESIAN_POINT('Ctrl Pts',(6.89176495873056,4.8,83.0121474888779));
#36576=CARTESIAN_POINT('Ctrl Pts',(6.91283571842148,4.8,82.9942403679326));
#36577=CARTESIAN_POINT('Ctrl Pts',(6.9331679365434,4.8,82.9763327128294));
#36578=CARTESIAN_POINT('Ctrl Pts',(6.94974459985959,4.8,82.9617327725942));
#36579=CARTESIAN_POINT('Ctrl Pts',(6.96582967712102,4.8,82.9471334117481));
#36580=CARTESIAN_POINT('Ctrl Pts',(6.98141328077829,4.8,82.9325391472623));
#36581=CARTESIAN_POINT('Ctrl Pts',(6.9984548522823,4.8,82.9165794753371));
#36582=CARTESIAN_POINT('Ctrl Pts',(7.01489884612417,4.8,82.9006223796449));
#36583=CARTESIAN_POINT('Ctrl Pts',(7.03075803262354,4.8,82.8846299962369));
#36584=CARTESIAN_POINT('Ctrl Pts',(7.04252732591772,4.8,82.8727618559127));
#36585=CARTESIAN_POINT('Ctrl Pts',(7.05397564589378,4.8,82.8608724252541));
#36586=CARTESIAN_POINT('Ctrl Pts',(7.06509695589111,4.8,82.8489644800917));
#36587=CARTESIAN_POINT('Ctrl Pts',(7.07526074030863,4.8,82.838081788438));
#36588=CARTESIAN_POINT('Ctrl Pts',(7.08515194755247,4.8,82.8271827043902));
#36589=CARTESIAN_POINT('Ctrl Pts',(7.09474587846554,4.8,82.816302611749));
#36590=CARTESIAN_POINT('Ctrl Pts',(7.10447120202654,4.8,82.8052735119704));
#36591=CARTESIAN_POINT('Ctrl Pts',(7.11389124561773,4.8,82.7942635690162));
#36592=CARTESIAN_POINT('Ctrl Pts',(7.12295157174751,4.8,82.7833576105563));
#36593=CARTESIAN_POINT('Ctrl Pts',(7.13556693213933,4.8,82.7681724401309));
#36594=CARTESIAN_POINT('Ctrl Pts',(7.14748271755908,4.8,82.7531921413648));
#36595=CARTESIAN_POINT('Ctrl Pts',(7.15850375899473,4.8,82.7387292749356));
#36596=CARTESIAN_POINT('Ctrl Pts',(7.16676954007146,4.8,82.7278821251137));
#36597=CARTESIAN_POINT('Ctrl Pts',(7.17453008192975,4.8,82.71732929294));
#36598=CARTESIAN_POINT('Ctrl Pts',(7.18171363533377,4.8,82.707188130266));
#36599=CARTESIAN_POINT('Ctrl Pts',(7.18865245925014,4.8,82.6973924569906));
#36600=CARTESIAN_POINT('Ctrl Pts',(7.19505240182619,4.8,82.6879817930411));
#36601=CARTESIAN_POINT('Ctrl Pts',(7.20087838488489,4.8,82.6790163090847));
#36602=CARTESIAN_POINT('Ctrl Pts',(7.20756143170267,4.8,82.6687319075646));
#36603=CARTESIAN_POINT('Ctrl Pts',(7.21348996431612,4.8,82.6590323626442));
#36604=CARTESIAN_POINT('Ctrl Pts',(7.21865051216571,4.8,82.6499454006877));
#36605=CARTESIAN_POINT('Ctrl Pts',(7.2229634423908,4.8,82.6423509680773));
#36606=CARTESIAN_POINT('Ctrl Pts',(7.22674120663366,4.8,82.6351824797662));
#36607=CARTESIAN_POINT('Ctrl Pts',(7.22998432988738,4.8,82.6284406437547));
#36608=CARTESIAN_POINT('',(7.3531668006526,4.8,82.2182109750381));
#36609=CARTESIAN_POINT('',(8.01502518871776,4.8,80.0140503863876));
#36610=CARTESIAN_POINT('',(8.09760744867255,4.8,82.4891652120952));
#36611=CARTESIAN_POINT('Origin',(9.31000000000056,4.8,77.9999999999986));
#36612=CARTESIAN_POINT('',(7.92828014771505,4.8,82.8825995361566));
#36613=CARTESIAN_POINT('',(8.92273797402872,4.8,80.571963032233));
#36614=CARTESIAN_POINT('',(8.07294956130202,4.8,83.871090717415));
#36615=CARTESIAN_POINT('Ctrl Pts',(7.92828014771505,4.8,82.8825995361566));
#36616=CARTESIAN_POINT('Ctrl Pts',(7.9173348789892,4.8,82.9255070749658));
#36617=CARTESIAN_POINT('Ctrl Pts',(7.91276563787875,4.8,82.9854352740174));
#36618=CARTESIAN_POINT('Ctrl Pts',(7.90710889583203,4.8,83.1768711867349));
#36619=CARTESIAN_POINT('Ctrl Pts',(7.92467731857551,4.8,83.324129034775));
#36620=CARTESIAN_POINT('Ctrl Pts',(7.9826350727204,4.8,83.5980315302565));
#36621=CARTESIAN_POINT('Ctrl Pts',(8.01988858795822,4.8,83.7281023348967));
#36622=CARTESIAN_POINT('Ctrl Pts',(8.07294956130202,4.8,83.8710907174151));
#36623=CARTESIAN_POINT('',(8.46441588009367,4.8,83.9401167914581));
#36624=CARTESIAN_POINT('Origin',(9.31,4.8,78.));
#36625=CARTESIAN_POINT('',(8.93844455602746,4.8,83.0607187762934));
#36626=CARTESIAN_POINT('Ctrl Pts',(8.46441588009367,4.8,83.9401167914581));
#36627=CARTESIAN_POINT('Ctrl Pts',(8.58010145233928,4.8,83.8039903313703));
#36628=CARTESIAN_POINT('Ctrl Pts',(8.68428079930222,4.8,83.6590948598213));
#36629=CARTESIAN_POINT('Ctrl Pts',(8.82124532673101,4.8,83.4122455604697));
#36630=CARTESIAN_POINT('Ctrl Pts',(8.85851086683854,4.8,83.3308593655485));
#36631=CARTESIAN_POINT('Ctrl Pts',(8.91127075343445,4.8,83.1876271019925));
#36632=CARTESIAN_POINT('Ctrl Pts',(8.93326894789525,4.8,83.1126668552635));
#36633=CARTESIAN_POINT('Ctrl Pts',(8.93844455602746,4.8,83.0607187762934));
#36634=CARTESIAN_POINT('',(8.91389140472481,4.8,82.6330980974667));
#36635=CARTESIAN_POINT('',(8.78196752755185,4.8,80.3354957565374));
#36636=CARTESIAN_POINT('',(9.70610859527519,4.8,82.6330980974667));
#36637=CARTESIAN_POINT('Origin',(9.31,4.8,78.0000000000002));
#36638=CARTESIAN_POINT('',(9.68155544397255,4.8,83.0607187762934));
#36639=CARTESIAN_POINT('',(9.82575589679681,4.8,80.5493060959508));
#36640=CARTESIAN_POINT('',(10.1555841198781,4.8,83.9401167914621));
#36641=CARTESIAN_POINT('Ctrl Pts',(9.68155544397255,4.8,83.0607187762934));
#36642=CARTESIAN_POINT('Ctrl Pts',(9.68594549803534,4.8,83.1047821733634));
#36643=CARTESIAN_POINT('Ctrl Pts',(9.70214846535674,4.8,83.1626590293364));
#36644=CARTESIAN_POINT('Ctrl Pts',(9.76230780763636,4.8,83.344484671119));
#36645=CARTESIAN_POINT('Ctrl Pts',(9.82918187530145,4.8,83.4768530296735));
#36646=CARTESIAN_POINT('Ctrl Pts',(9.9773245196029,4.8,83.7144144633533));
#36647=CARTESIAN_POINT('Ctrl Pts',(10.0568182080785,4.8,83.8238995857148));
#36648=CARTESIAN_POINT('Ctrl Pts',(10.1555841198781,4.8,83.9401167914621));
#36649=CARTESIAN_POINT('',(10.5470504386678,4.8,83.8710907174214));
#36650=CARTESIAN_POINT('Origin',(9.31,4.8,78.));
#36651=CARTESIAN_POINT('',(10.691719852285,4.8,82.8825995361566));
#36652=CARTESIAN_POINT('Ctrl Pts',(10.5470504386678,4.8,83.8710907174214));
#36653=CARTESIAN_POINT('Ctrl Pts',(10.565435231738,4.8,83.8215474908647));
#36654=CARTESIAN_POINT('Ctrl Pts',(10.5823033780305,4.8,83.7725242711596));
#36655=CARTESIAN_POINT('Ctrl Pts',(10.5975993793386,4.8,83.7240516819789));
#36656=CARTESIAN_POINT('Ctrl Pts',(10.6098250669771,4.8,83.6853088287051));
#36657=CARTESIAN_POINT('Ctrl Pts',(10.6210457117067,4.8,83.6469154229001));
#36658=CARTESIAN_POINT('Ctrl Pts',(10.6312523175355,4.8,83.6089036335644));
#36659=CARTESIAN_POINT('Ctrl Pts',(10.6394283181237,4.8,83.5784542934822));
#36660=CARTESIAN_POINT('Ctrl Pts',(10.6469541138919,4.8,83.5482488347871));
#36661=CARTESIAN_POINT('Ctrl Pts',(10.6538335015972,4.8,83.5183408516636));
#36662=CARTESIAN_POINT('Ctrl Pts',(10.6613445974944,4.8,83.4856865314016));
#36663=CARTESIAN_POINT('Ctrl Pts',(10.6680852688832,4.8,83.4533858670217));
#36664=CARTESIAN_POINT('Ctrl Pts',(10.674069103033,4.8,83.421584154235));
#36665=CARTESIAN_POINT('Ctrl Pts',(10.6792707883309,4.8,83.3939392533715));
#36666=CARTESIAN_POINT('Ctrl Pts',(10.6839014512246,4.8,83.3666775796467));
#36667=CARTESIAN_POINT('Ctrl Pts',(10.6879660151044,4.8,83.339890222103));
#36668=CARTESIAN_POINT('Ctrl Pts',(10.6912798152377,4.8,83.3180507451939));
#36669=CARTESIAN_POINT('Ctrl Pts',(10.6942174110287,4.8,83.2965276975492));
#36670=CARTESIAN_POINT('Ctrl Pts',(10.6967741316292,4.8,83.2753308949627));
#36671=CARTESIAN_POINT('Ctrl Pts',(10.6995700533865,4.8,83.2521509661404));
#36672=CARTESIAN_POINT('Ctrl Pts',(10.7019098600755,4.8,83.2293571263374));
#36673=CARTESIAN_POINT('Ctrl Pts',(10.7037789958498,4.8,83.2069121614836));
#36674=CARTESIAN_POINT('Ctrl Pts',(10.7051661040288,4.8,83.1902554826306));
#36675=CARTESIAN_POINT('Ctrl Pts',(10.7062936472176,4.8,83.1737888121069));
#36676=CARTESIAN_POINT('Ctrl Pts',(10.7071587853345,4.8,83.1575181566129));
#36677=CARTESIAN_POINT('Ctrl Pts',(10.7079494365539,4.8,83.1426483764518));
#36678=CARTESIAN_POINT('Ctrl Pts',(10.7085207447153,4.8,83.1279412482181));
#36679=CARTESIAN_POINT('Ctrl Pts',(10.7088765334352,4.8,83.113439753788));
#36680=CARTESIAN_POINT('Ctrl Pts',(10.7092371948217,4.8,83.098739655688));
#36681=CARTESIAN_POINT('Ctrl Pts',(10.7093763119515,4.8,83.0842504627495));
#36682=CARTESIAN_POINT('Ctrl Pts',(10.7093067094632,4.8,83.070072148483));
#36683=CARTESIAN_POINT('Ctrl Pts',(10.7092097967847,4.8,83.0503306357088));
#36684=CARTESIAN_POINT('Ctrl Pts',(10.7087086675511,4.8,83.031195741855));
#36685=CARTESIAN_POINT('Ctrl Pts',(10.70785472376,4.8,83.0130323545146));
#36686=CARTESIAN_POINT('Ctrl Pts',(10.7072142659167,4.8,82.9994098140094));
#36687=CARTESIAN_POINT('Ctrl Pts',(10.7063759561179,4.8,82.9863374954128));
#36688=CARTESIAN_POINT('Ctrl Pts',(10.705360263576,4.8,82.9739514149783));
#36689=CARTESIAN_POINT('Ctrl Pts',(10.7043791736755,4.8,82.9619873038731));
#36690=CARTESIAN_POINT('Ctrl Pts',(10.7032327559455,4.8,82.9506645132699));
#36691=CARTESIAN_POINT('Ctrl Pts',(10.7019328158995,4.8,82.9400516843912));
#36692=CARTESIAN_POINT('Ctrl Pts',(10.7004416409093,4.8,82.9278775960186));
#36693=CARTESIAN_POINT('Ctrl Pts',(10.6987484130779,4.8,82.916636526183));
#36694=CARTESIAN_POINT('Ctrl Pts',(10.6968606355152,4.8,82.9063583732204));
#36695=CARTESIAN_POINT('Ctrl Pts',(10.6952829245654,4.8,82.8977684022446));
#36696=CARTESIAN_POINT('Ctrl Pts',(10.6935690444019,4.8,82.8898487215898));
#36697=CARTESIAN_POINT('Ctrl Pts',(10.691719852285,4.8,82.8825995361566));
#36698=CARTESIAN_POINT('',(10.5223925513275,4.8,82.4891652120952));
#36699=CARTESIAN_POINT('',(9.61259837549256,4.8,80.3752458702023));
#36700=CARTESIAN_POINT('',(11.2668331993474,4.8,82.2182109750381));
#36701=CARTESIAN_POINT('Origin',(9.31000000000013,4.8,78.0000000000003));
#36702=CARTESIAN_POINT('',(11.3900156701126,4.8,82.6284406437547));
#36703=CARTESIAN_POINT('',(10.6665660466648,4.8,80.2191652207459));
#36704=CARTESIAN_POINT('',(12.1362287541399,4.8,83.2926771136423));
#36705=CARTESIAN_POINT('Ctrl Pts',(11.3900156701126,4.8,82.6284406437547));
#36706=CARTESIAN_POINT('Ctrl Pts',(11.4092115405355,4.8,82.6683452050612));
#36707=CARTESIAN_POINT('Ctrl Pts',(11.4442323990395,4.8,82.7171899177271));
#36708=CARTESIAN_POINT('Ctrl Pts',(11.5629517238869,4.8,82.8674744276728));
#36709=CARTESIAN_POINT('Ctrl Pts',(11.6710654366442,4.8,82.9689877189041));
#36710=CARTESIAN_POINT('Ctrl Pts',(11.8915247821159,4.8,83.1415546766503));
#36711=CARTESIAN_POINT('Ctrl Pts',(12.0036705310799,4.8,83.2172485947785));
#36712=CARTESIAN_POINT('Ctrl Pts',(12.1362287541399,4.8,83.2926771136423));
#36713=CARTESIAN_POINT('',(12.4804784574569,4.8,83.09392445476));
#36714=CARTESIAN_POINT('Origin',(9.31,4.8,78.));
#36715=CARTESIAN_POINT('',(12.2783393423437,4.8,82.1155667324646));
#36716=CARTESIAN_POINT('Ctrl Pts',(12.4804784574569,4.8,83.09392445476));
#36717=CARTESIAN_POINT('Ctrl Pts',(12.4808097303862,4.8,83.0410810807943));
#36718=CARTESIAN_POINT('Ctrl Pts',(12.4798936743225,4.8,82.9892450771466));
#36719=CARTESIAN_POINT('Ctrl Pts',(12.4776886119629,4.8,82.9384642022077));
#36720=CARTESIAN_POINT('Ctrl Pts',(12.4759261639599,4.8,82.8978763924165));
#36721=CARTESIAN_POINT('Ctrl Pts',(12.4733388024296,4.8,82.857960700928));
#36722=CARTESIAN_POINT('Ctrl Pts',(12.4699290763522,4.8,82.8187504335389));
#36723=CARTESIAN_POINT('Ctrl Pts',(12.4671977160268,4.8,82.7873410574586));
#36724=CARTESIAN_POINT('Ctrl Pts',(12.4639387754109,4.8,82.7563832380486));
#36725=CARTESIAN_POINT('Ctrl Pts',(12.4601741525764,4.8,82.7259260387977));
#36726=CARTESIAN_POINT('Ctrl Pts',(12.4560638384958,4.8,82.6926720687609));
#36727=CARTESIAN_POINT('Ctrl Pts',(12.451350519618,4.8,82.6600139272687));
#36728=CARTESIAN_POINT('Ctrl Pts',(12.4460966578638,4.8,82.6280835005169));
#36729=CARTESIAN_POINT('Ctrl Pts',(12.4415295301632,4.8,82.6003267106864));
#36730=CARTESIAN_POINT('Ctrl Pts',(12.4365568883439,4.8,82.5731253377266));
#36731=CARTESIAN_POINT('Ctrl Pts',(12.4312145131633,4.8,82.5465632934318));
#36732=CARTESIAN_POINT('Ctrl Pts',(12.4268589256494,4.8,82.524907512143));
#36733=CARTESIAN_POINT('Ctrl Pts',(12.4222580468816,4.8,82.5036777465558));
#36734=CARTESIAN_POINT('Ctrl Pts',(12.4174108448943,4.8,82.4828848180173));
#36735=CARTESIAN_POINT('Ctrl Pts',(12.4121101496759,4.8,82.4601465502152));
#36736=CARTESIAN_POINT('Ctrl Pts',(12.4065128967569,4.8,82.4379270878765));
#36737=CARTESIAN_POINT('Ctrl Pts',(12.4005926801591,4.8,82.4161964396135));
#36738=CARTESIAN_POINT('Ctrl Pts',(12.3961992158058,4.8,82.4000698626646));
#36739=CARTESIAN_POINT('Ctrl Pts',(12.3916268268252,4.8,82.3842106115907));
#36740=CARTESIAN_POINT('Ctrl Pts',(12.386874898827,4.8,82.368625302211));
#36741=CARTESIAN_POINT('Ctrl Pts',(12.3825321035846,4.8,82.3543818609281));
#36742=CARTESIAN_POINT('Ctrl Pts',(12.3780388235253,4.8,82.3403662822065));
#36743=CARTESIAN_POINT('Ctrl Pts',(12.3734133523422,4.8,82.326617648047));
#36744=CARTESIAN_POINT('Ctrl Pts',(12.3687245334624,4.8,82.3126807207881));
#36745=CARTESIAN_POINT('Ctrl Pts',(12.3638996648925,4.8,82.2990177521613));
#36746=CARTESIAN_POINT('Ctrl Pts',(12.3589849908085,4.8,82.2857183002578));
#36747=CARTESIAN_POINT('Ctrl Pts',(12.3521419277283,4.8,82.2672004928195));
#36748=CARTESIAN_POINT('Ctrl Pts',(12.3451265012387,4.8,82.2493909709054));
#36749=CARTESIAN_POINT('Ctrl Pts',(12.3381118123199,4.8,82.2326150361613));
#36750=CARTESIAN_POINT('Ctrl Pts',(12.3328507956308,4.8,82.2200330851033));
#36751=CARTESIAN_POINT('Ctrl Pts',(12.3275920459005,4.8,82.2080358428568));
#36752=CARTESIAN_POINT('Ctrl Pts',(12.3224013181914,4.8,82.1967441220017));
#36753=CARTESIAN_POINT('Ctrl Pts',(12.3173874282394,4.8,82.1858370875918));
#36754=CARTESIAN_POINT('Ctrl Pts',(12.3124375254797,4.8,82.1755892427828));
#36755=CARTESIAN_POINT('Ctrl Pts',(12.3075861801448,4.8,82.1660610515014));
#36756=CARTESIAN_POINT('Ctrl Pts',(12.3020211505258,4.8,82.15513116236));
#36757=CARTESIAN_POINT('Ctrl Pts',(12.2965853644795,4.8,82.1451471300143));
#36758=CARTESIAN_POINT('Ctrl Pts',(12.2912960984526,4.8,82.136134483496));
#36759=CARTESIAN_POINT('Ctrl Pts',(12.2868755922982,4.8,82.1286021606371));
#36760=CARTESIAN_POINT('Ctrl Pts',(12.2825563817151,4.8,82.1217462771787));
#36761=CARTESIAN_POINT('Ctrl Pts',(12.2783393423437,4.8,82.1155667324646));
#36762=CARTESIAN_POINT('',(11.9846612632316,4.8,81.8037727491227));
#36763=CARTESIAN_POINT('',(10.4067313934724,4.8,80.1285062770252));
#36764=CARTESIAN_POINT('',(12.5915348397961,4.8,81.2945453548562));
#36765=CARTESIAN_POINT('Origin',(9.31000000000031,4.8,78.0000000000004));
#36766=CARTESIAN_POINT('',(12.8475953086752,4.8,81.6379042610703));
#36767=CARTESIAN_POINT('',(11.3437543105226,4.8,79.6213602685287));
#36768=CARTESIAN_POINT('',(13.7759884899248,4.8,82.0068624643054));
#36769=CARTESIAN_POINT('Ctrl Pts',(12.8475953086752,4.8,81.6379042610703));
#36770=CARTESIAN_POINT('Ctrl Pts',(12.8792816901564,4.8,81.668836908395));
#36771=CARTESIAN_POINT('Ctrl Pts',(12.9288964078831,4.8,81.7027580854298));
#36772=CARTESIAN_POINT('Ctrl Pts',(13.0918564124497,4.8,81.8033749305029));
#36773=CARTESIAN_POINT('Ctrl Pts',(13.2281696606021,4.8,81.8617891535078));
#36774=CARTESIAN_POINT('Ctrl Pts',(13.4943550569333,4.8,81.9485475134328));
#36775=CARTESIAN_POINT('Ctrl Pts',(13.6256264337655,4.8,81.9813204243067));
#36776=CARTESIAN_POINT('Ctrl Pts',(13.7759884899248,4.8,82.0068624643054));
#36777=CARTESIAN_POINT('',(14.0314999829639,4.8,81.7023557245181));
#36778=CARTESIAN_POINT('Origin',(9.31,4.8,78.));
#36779=CARTESIAN_POINT('',(13.5069332996928,4.8,80.8521358415414));
#36780=CARTESIAN_POINT('Ctrl Pts',(14.0314999829639,4.8,81.7023557245181));
#36781=CARTESIAN_POINT('Ctrl Pts',(14.0137377793507,4.8,81.6525858939324));
#36782=CARTESIAN_POINT('Ctrl Pts',(13.9951480108104,4.8,81.6041892934436));
#36783=CARTESIAN_POINT('Ctrl Pts',(13.9757078478474,4.8,81.5572250557336));
#36784=CARTESIAN_POINT('Ctrl Pts',(13.9601698393049,4.8,81.5196877815801));
#36785=CARTESIAN_POINT('Ctrl Pts',(13.9440865435676,4.8,81.483064229152));
#36786=CARTESIAN_POINT('Ctrl Pts',(13.9274717471481,4.8,81.4473848238621));
#36787=CARTESIAN_POINT('Ctrl Pts',(13.9141624688315,4.8,81.4188038456076));
#36788=CARTESIAN_POINT('Ctrl Pts',(13.9005118686982,4.8,81.3908276348962));
#36789=CARTESIAN_POINT('Ctrl Pts',(13.8865573049032,4.8,81.3634948067451));
#36790=CARTESIAN_POINT('Ctrl Pts',(13.8713213455486,4.8,81.3336521069032));
#36791=CARTESIAN_POINT('Ctrl Pts',(13.8557225324051,4.8,81.3045755425303));
#36792=CARTESIAN_POINT('Ctrl Pts',(13.8398646682139,4.8,81.2763676828765));
#36793=CARTESIAN_POINT('Ctrl Pts',(13.8260795908255,4.8,81.2518468821179));
#36794=CARTESIAN_POINT('Ctrl Pts',(13.812103418573,4.8,81.2279866964885));
#36795=CARTESIAN_POINT('Ctrl Pts',(13.7979984738936,4.8,81.2048537395401));
#36796=CARTESIAN_POINT('Ctrl Pts',(13.786498847035,4.8,81.1859936603912));
#36797=CARTESIAN_POINT('Ctrl Pts',(13.7749144277477,4.8,81.1676177996027));
#36798=CARTESIAN_POINT('Ctrl Pts',(13.7632479474187,4.8,81.1497366788665));
#36799=CARTESIAN_POINT('Ctrl Pts',(13.750489977824,4.8,81.1301826412959));
#36800=CARTESIAN_POINT('Ctrl Pts',(13.7376307770682,4.8,81.1112175500781));
#36801=CARTESIAN_POINT('Ctrl Pts',(13.7246352739907,4.8,81.0928222539058));
#36802=CARTESIAN_POINT('Ctrl Pts',(13.7149911538226,4.8,81.0791708819076));
#36803=CARTESIAN_POINT('Ctrl Pts',(13.7052703303368,4.8,81.0658319098867));
#36804=CARTESIAN_POINT('Ctrl Pts',(13.6954744889387,4.8,81.0528117648138));
#36805=CARTESIAN_POINT('Ctrl Pts',(13.6865220524789,4.8,81.040912631628));
#36806=CARTESIAN_POINT('Ctrl Pts',(13.6775061401329,4.8,81.0292790880483));
#36807=CARTESIAN_POINT('Ctrl Pts',(13.6684573091815,4.8,81.0179416023308));
#36808=CARTESIAN_POINT('Ctrl Pts',(13.6592845507989,4.8,81.0064488451214));
#36809=CARTESIAN_POINT('Ctrl Pts',(13.6500776468974,4.8,80.9952600565541));
#36810=CARTESIAN_POINT('Ctrl Pts',(13.6409106834611,4.8,80.9844435772673));
#36811=CARTESIAN_POINT('Ctrl Pts',(13.6281468444773,4.8,80.9693829957619));
#36812=CARTESIAN_POINT('Ctrl Pts',(13.6154632847898,4.8,80.9550469366923));
#36813=CARTESIAN_POINT('Ctrl Pts',(13.6031339258266,4.8,80.9416818795899));
#36814=CARTESIAN_POINT('Ctrl Pts',(13.5938869066041,4.8,80.9316580867631));
#36815=CARTESIAN_POINT('Ctrl Pts',(13.584841999819,4.8,80.9221829651429));
#36816=CARTESIAN_POINT('Ctrl Pts',(13.5761023153521,4.8,80.9133475518622));
#36817=CARTESIAN_POINT('Ctrl Pts',(13.5676603744987,4.8,80.9048131434847));
#36818=CARTESIAN_POINT('Ctrl Pts',(13.5595040180612,4.8,80.8968762858028));
#36819=CARTESIAN_POINT('Ctrl Pts',(13.5516864113113,4.8,80.8895819726066));
#36820=CARTESIAN_POINT('Ctrl Pts',(13.5427187517547,4.8,80.8812145886315));
#36821=CARTESIAN_POINT('Ctrl Pts',(13.5341960435113,4.8,80.8736918154127));
#36822=CARTESIAN_POINT('Ctrl Pts',(13.5261432525711,4.8,80.8670317335012));
#36823=CARTESIAN_POINT('Ctrl Pts',(13.5194131295563,4.8,80.8614655675736));
#36824=CARTESIAN_POINT('Ctrl Pts',(13.5130095491284,4.8,80.8565004016111));
#36825=CARTESIAN_POINT('Ctrl Pts',(13.5069332996928,4.8,80.8521358415414));
#36826=CARTESIAN_POINT('',(13.1243263529939,4.8,80.659589154899));
#36827=CARTESIAN_POINT('',(11.0685824193681,4.8,79.6250374134319));
#36828=CARTESIAN_POINT('',(13.5204349482691,4.8,79.9735089425676));
#36829=CARTESIAN_POINT('Origin',(9.31000000000061,4.8,78.0000000000004));
#36830=CARTESIAN_POINT('',(13.8784887436653,4.8,80.2085829347521));
#36831=CARTESIAN_POINT('',(11.7756417895143,4.8,78.8279953391977));
#36832=CARTESIAN_POINT('',(14.877084102819,4.8,80.237761066812));
#36833=CARTESIAN_POINT('Ctrl Pts',(13.8784887436653,4.8,80.2085829347521));
#36834=CARTESIAN_POINT('Ctrl Pts',(13.9188437915828,4.8,80.226812734718));
#36835=CARTESIAN_POINT('Ctrl Pts',(13.9770681023252,4.8,80.241718981607));
#36836=CARTESIAN_POINT('Ctrl Pts',(14.1646134025171,4.8,80.2805322840692));
#36837=CARTESIAN_POINT('Ctrl Pts',(14.3126847969111,4.8,80.2888018216863));
#36838=CARTESIAN_POINT('Ctrl Pts',(14.5924903558759,4.8,80.2792872449101));
#36839=CARTESIAN_POINT('Ctrl Pts',(14.7270540960429,4.8,80.2651862522944));
#36840=CARTESIAN_POINT('Ctrl Pts',(14.877084102819,4.8,80.237761066812));
#36841=CARTESIAN_POINT('',(15.0130389285914,4.8,79.8642282529162));
#36842=CARTESIAN_POINT('Origin',(9.31,4.8,78.));
#36843=CARTESIAN_POINT('',(14.2293151609602,4.8,79.2446952750862));
#36844=CARTESIAN_POINT('Ctrl Pts',(15.0130389285914,4.8,79.8642282529162));
#36845=CARTESIAN_POINT('Ctrl Pts',(14.9793256323352,4.8,79.8235349418062));
#36846=CARTESIAN_POINT('Ctrl Pts',(14.9453043517715,4.8,79.7844150887897));
#36847=CARTESIAN_POINT('Ctrl Pts',(14.9109738587714,4.8,79.7469320685151));
#36848=CARTESIAN_POINT('Ctrl Pts',(14.8835344026255,4.8,79.7169728805989));
#36849=CARTESIAN_POINT('Ctrl Pts',(14.8558950553602,4.8,79.6880588094625));
#36850=CARTESIAN_POINT('Ctrl Pts',(14.8280791781634,4.8,79.6602137303782));
#36851=CARTESIAN_POINT('Ctrl Pts',(14.8057972773248,4.8,79.6379084373754));
#36852=CARTESIAN_POINT('Ctrl Pts',(14.7834014815771,4.8,79.6162881788984));
#36853=CARTESIAN_POINT('Ctrl Pts',(14.7609401032154,4.8,79.5953764639576));
#36854=CARTESIAN_POINT('Ctrl Pts',(14.7364161795572,4.8,79.5725445035804));
#36855=CARTESIAN_POINT('Ctrl Pts',(14.7118133186302,4.8,79.5505565783982));
#36856=CARTESIAN_POINT('Ctrl Pts',(14.6872641438652,4.8,79.5294735693576));
#36857=CARTESIAN_POINT('Ctrl Pts',(14.6659238006834,4.8,79.5111463281149));
#36858=CARTESIAN_POINT('Ctrl Pts',(14.6446298307527,4.8,79.4935052203248));
#36859=CARTESIAN_POINT('Ctrl Pts',(14.6234635811816,4.8,79.4765915267188));
#36860=CARTESIAN_POINT('Ctrl Pts',(14.6062069397889,4.8,79.4628019536438));
#36861=CARTESIAN_POINT('Ctrl Pts',(14.5890362320106,4.8,79.4494963977045));
#36862=CARTESIAN_POINT('Ctrl Pts',(14.5719576231394,4.8,79.4366838118659));
#36863=CARTESIAN_POINT('Ctrl Pts',(14.553281178991,4.8,79.4226725100313));
#36864=CARTESIAN_POINT('Ctrl Pts',(14.5347110401775,4.8,79.4092492598048));
#36865=CARTESIAN_POINT('Ctrl Pts',(14.5162077004567,4.8,79.3964080598874));
#36866=CARTESIAN_POINT('Ctrl Pts',(14.5024761477173,4.8,79.3868784497433));
#36867=CARTESIAN_POINT('Ctrl Pts',(14.4887793645206,4.8,79.3776686336305));
#36868=CARTESIAN_POINT('Ctrl Pts',(14.4751211327833,4.8,79.3687840744841));
#36869=CARTESIAN_POINT('Ctrl Pts',(14.462638851088,4.8,79.3606644604567));
#36870=CARTESIAN_POINT('Ctrl Pts',(14.4501877585656,4.8,79.3528161290529));
#36871=CARTESIAN_POINT('Ctrl Pts',(14.4378069904251,4.8,79.3452572598632));
#36872=CARTESIAN_POINT('Ctrl Pts',(14.4252566625921,4.8,79.3375948688627));
#36873=CARTESIAN_POINT('Ctrl Pts',(14.4127782118658,4.8,79.330229793408));
#36874=CARTESIAN_POINT('Ctrl Pts',(14.4004646301748,4.8,79.3232009137939));
#36875=CARTESIAN_POINT('Ctrl Pts',(14.3833195226597,4.8,79.3134140865556));
#36876=CARTESIAN_POINT('Ctrl Pts',(14.3664976542761,4.8,79.3042806305664));
#36877=CARTESIAN_POINT('Ctrl Pts',(14.3503407279331,4.8,79.2959384741763));
#36878=CARTESIAN_POINT('Ctrl Pts',(14.3382230331759,4.8,79.2896818568836));
#36879=CARTESIAN_POINT('Ctrl Pts',(14.3264829185903,4.8,79.2838716953493));
#36880=CARTESIAN_POINT('Ctrl Pts',(14.3152484123024,4.8,79.2785582708383));
#36881=CARTESIAN_POINT('Ctrl Pts',(14.3043966432488,4.8,79.2734258641086));
#36882=CARTESIAN_POINT('Ctrl Pts',(14.2940176101361,4.8,79.2687572957321));
#36883=CARTESIAN_POINT('Ctrl Pts',(14.2841766607576,4.8,79.2645766624468));
#36884=CARTESIAN_POINT('Ctrl Pts',(14.2728880033202,4.8,79.2597810136519));
#36885=CARTESIAN_POINT('Ctrl Pts',(14.2623063372479,4.8,79.2556268570475));
#36886=CARTESIAN_POINT('Ctrl Pts',(14.2524613068071,4.8,79.2521226439224));
#36887=CARTESIAN_POINT('Ctrl Pts',(14.2442333190914,4.8,79.2491939965485));
#36888=CARTESIAN_POINT('Ctrl Pts',(14.2365177351167,4.8,79.2467184202557));
#36889=CARTESIAN_POINT('Ctrl Pts',(14.2293151609602,4.8,79.2446952750862));
#36890=CARTESIAN_POINT('',(13.8039273911235,4.8,79.194619857239));
#36891=CARTESIAN_POINT('',(11.5183224515755,4.8,78.9255650547807));
#36892=CARTESIAN_POINT('',(13.941494462579,4.8,78.4144382259154));
#36893=CARTESIAN_POINT('Origin',(9.30999999999925,4.8,77.9999999999999));
#36894=CARTESIAN_POINT('',(14.3583550124563,4.8,78.5128739112901));
#36895=CARTESIAN_POINT('',(11.9101364796933,4.8,77.9347619520498));
#36896=CARTESIAN_POINT('',(15.306707211514,4.8,78.1987526587886));
#36897=CARTESIAN_POINT('Ctrl Pts',(14.3583550124563,4.8,78.5128739112901));
#36898=CARTESIAN_POINT('Ctrl Pts',(14.4025113095208,4.8,78.5162020802714));
#36899=CARTESIAN_POINT('Ctrl Pts',(14.4623224986856,4.8,78.5102954845377));
#36900=CARTESIAN_POINT('Ctrl Pts',(14.655508486079,4.8,78.4820870105105));
#36901=CARTESIAN_POINT('Ctrl Pts',(14.7941933914243,4.8,78.4380535020656));
#36902=CARTESIAN_POINT('Ctrl Pts',(15.0510922588474,4.8,78.3375379190762));
#36903=CARTESIAN_POINT('Ctrl Pts',(15.1814858801512,4.8,78.2720997067482));
#36904=CARTESIAN_POINT('Ctrl Pts',(15.306707211514,4.8,78.1987526587886));
#36905=CARTESIAN_POINT('',(15.3067072115039,4.8,77.8012473409061));
#36906=CARTESIAN_POINT('Origin',(9.31,4.8,78.));
#36907=CARTESIAN_POINT('',(14.3583550124563,4.8,77.4871260887099));
#36908=CARTESIAN_POINT('Ctrl Pts',(15.3067072115039,4.8,77.8012473409061));
#36909=CARTESIAN_POINT('Ctrl Pts',(15.2611091436898,4.8,77.7745387631645));
#36910=CARTESIAN_POINT('Ctrl Pts',(15.2157598196307,4.8,77.7494140892397));
#36911=CARTESIAN_POINT('Ctrl Pts',(15.1706797607092,4.8,77.7259332918341));
#36912=CARTESIAN_POINT('Ctrl Pts',(15.1346484571073,4.8,77.7071657089965));
#36913=CARTESIAN_POINT('Ctrl Pts',(15.0987867683259,4.8,77.6894485816647));
#36914=CARTESIAN_POINT('Ctrl Pts',(15.063124812535,4.8,77.6727963552642));
#36915=CARTESIAN_POINT('Ctrl Pts',(15.0345578158729,4.8,77.6594570953877));
#36916=CARTESIAN_POINT('Ctrl Pts',(15.006118088614,4.8,77.6468005117217));
#36917=CARTESIAN_POINT('Ctrl Pts',(14.9778590700176,4.8,77.6348321717349));
#36918=CARTESIAN_POINT('Ctrl Pts',(14.9470051291957,4.8,77.6217648229016));
#36919=CARTESIAN_POINT('Ctrl Pts',(14.9163656886571,4.8,77.6095176058724));
#36920=CARTESIAN_POINT('Ctrl Pts',(14.8860861961812,4.8,77.5981023701413));
#36921=CARTESIAN_POINT('Ctrl Pts',(14.8597645479413,4.8,77.5881792243115));
#36922=CARTESIAN_POINT('Ctrl Pts',(14.833721147768,4.8,77.5788849724225));
#36923=CARTESIAN_POINT('Ctrl Pts',(14.8080465557734,4.8,77.5702305833215));
#36924=CARTESIAN_POINT('Ctrl Pts',(14.7871143057029,4.8,77.5631747423989));
#36925=CARTESIAN_POINT('Ctrl Pts',(14.7664283504253,4.8,77.5565443377725));
#36926=CARTESIAN_POINT('Ctrl Pts',(14.7459975455092,4.8,77.5503456738222));
#36927=CARTESIAN_POINT('Ctrl Pts',(14.723655282707,4.8,77.5435670775032));
#36928=CARTESIAN_POINT('Ctrl Pts',(14.7016140396996,4.8,77.537304710313));
#36929=CARTESIAN_POINT('Ctrl Pts',(14.6798346402041,4.8,77.5315664448051));
#36930=CARTESIAN_POINT('Ctrl Pts',(14.6636718829377,4.8,77.5273080081778));
#36931=CARTESIAN_POINT('Ctrl Pts',(14.6476511743518,4.8,77.5233381877535));
#36932=CARTESIAN_POINT('Ctrl Pts',(14.6317779367209,4.8,77.5196608235206));
#36933=CARTESIAN_POINT('Ctrl Pts',(14.6172713572202,4.8,77.5163000739471));
#36934=CARTESIAN_POINT('Ctrl Pts',(14.6028868700773,4.8,77.5131835793267));
#36935=CARTESIAN_POINT('Ctrl Pts',(14.5886674681478,4.8,77.5103150378569));
#36936=CARTESIAN_POINT('Ctrl Pts',(14.5742533255308,4.8,77.5074072105056));
#36937=CARTESIAN_POINT('Ctrl Pts',(14.5600084132126,4.8,77.5047541849647));
#36938=CARTESIAN_POINT('Ctrl Pts',(14.5460334128722,4.8,77.5023606916477));
#36939=CARTESIAN_POINT('Ctrl Pts',(14.5265749900718,4.8,77.4990280545245));
#36940=CARTESIAN_POINT('Ctrl Pts',(14.5076437788303,4.8,77.4961988312379));
#36941=CARTESIAN_POINT('Ctrl Pts',(14.4896080491137,4.8,77.4938857627618));
#36942=CARTESIAN_POINT('Ctrl Pts',(14.4760812518262,4.8,77.4921509614047));
#36943=CARTESIAN_POINT('Ctrl Pts',(14.4630619606985,4.8,77.4907065511982));
#36944=CARTESIAN_POINT('Ctrl Pts',(14.4506876800147,4.8,77.4895559928777));
#36945=CARTESIAN_POINT('Ctrl Pts',(14.4387349662656,4.8,77.4884446317726));
#36946=CARTESIAN_POINT('Ctrl Pts',(14.4273851210563,4.8,77.487607450931));
#36947=CARTESIAN_POINT('Ctrl Pts',(14.4167077927931,4.8,77.4870447436184));
#36948=CARTESIAN_POINT('Ctrl Pts',(14.4044597161182,4.8,77.4863992560827));
#36949=CARTESIAN_POINT('Ctrl Pts',(14.3930953972864,4.8,77.4861147687456));
#36950=CARTESIAN_POINT('Ctrl Pts',(14.3826455833045,4.8,77.486189084285));
#36951=CARTESIAN_POINT('Ctrl Pts',(14.3739121480898,4.8,77.4862511935197));
#36952=CARTESIAN_POINT('Ctrl Pts',(14.3658151742579,4.8,77.4865637978793));
#36953=CARTESIAN_POINT('Ctrl Pts',(14.3583550124563,4.8,77.4871260887099));
#36954=CARTESIAN_POINT('',(13.941494462579,4.8,77.5855617740846));
#36955=CARTESIAN_POINT('',(11.7017062047547,4.8,78.1144558906375));
#36956=CARTESIAN_POINT('',(13.8039273911235,4.8,76.805380142761));
#36957=CARTESIAN_POINT('Origin',(9.30999999999972,4.8,78.0000000000001));
#36958=CARTESIAN_POINT('',(14.2293151609602,4.8,76.7553047249138));
#36959=CARTESIAN_POINT('',(11.7310163364939,4.8,77.0493972362957));
#36960=CARTESIAN_POINT('',(15.0130389285309,4.8,76.1357717468986));
#36961=CARTESIAN_POINT('Ctrl Pts',(14.2293151609602,4.8,76.7553047249138));
#36962=CARTESIAN_POINT('Ctrl Pts',(14.2719468108673,4.8,76.7433298370116));
#36963=CARTESIAN_POINT('Ctrl Pts',(14.3261307716226,4.8,76.7173228190353));
#36964=CARTESIAN_POINT('Ctrl Pts',(14.4947475177318,4.8,76.62650373751));
#36965=CARTESIAN_POINT('Ctrl Pts',(14.6134923426114,4.8,76.5376601132773));
#36966=CARTESIAN_POINT('Ctrl Pts',(14.8217199834009,4.8,76.3505159786347));
#36967=CARTESIAN_POINT('Ctrl Pts',(14.9157378453733,4.8,76.2532180867664));
#36968=CARTESIAN_POINT('Ctrl Pts',(15.0130389285309,4.8,76.1357717468986));
#36969=CARTESIAN_POINT('',(14.8770841027247,4.8,75.7622389329533));
#36970=CARTESIAN_POINT('Origin',(9.31,4.8,78.));
#36971=CARTESIAN_POINT('',(13.8784887436653,4.8,75.7914170652479));
#36972=CARTESIAN_POINT('Ctrl Pts',(14.8770841027247,4.8,75.7622389329533));
#36973=CARTESIAN_POINT('Ctrl Pts',(14.7013523460961,4.8,75.7301155190193));
#36974=CARTESIAN_POINT('Ctrl Pts',(14.5237795099726,4.8,75.7123412935216));
#36975=CARTESIAN_POINT('Ctrl Pts',(14.241519484279,4.8,75.7171511830311));
#36976=CARTESIAN_POINT('Ctrl Pts',(14.1524042015108,4.8,75.7255713759847));
#36977=CARTESIAN_POINT('Ctrl Pts',(14.0019814863757,4.8,75.751496104531));
#36978=CARTESIAN_POINT('Ctrl Pts',(13.9260649067567,4.8,75.7699252323531));
#36979=CARTESIAN_POINT('Ctrl Pts',(13.8784887436653,4.8,75.7914170652479));
#36980=CARTESIAN_POINT('',(13.5204349482691,4.8,76.0264910574324));
#36981=CARTESIAN_POINT('',(11.5966148918162,4.8,77.2895416568946));
#36982=CARTESIAN_POINT('',(13.1243263529939,4.8,75.340410845101));
#36983=CARTESIAN_POINT('Origin',(9.31000000000134,4.8,77.9999999999992));
#36984=CARTESIAN_POINT('',(13.5069332996928,4.8,75.1478641584586));
#36985=CARTESIAN_POINT('',(11.2598858927175,4.8,76.278689243247));
#36986=CARTESIAN_POINT('',(14.0314999829165,4.8,74.2976442754215));
#36987=CARTESIAN_POINT('Ctrl Pts',(13.5069332996928,4.8,75.1478641584586));
#36988=CARTESIAN_POINT('Ctrl Pts',(13.5428982946376,4.8,75.1220305609756));
#36989=CARTESIAN_POINT('Ctrl Pts',(13.5849196393322,4.8,75.079059950823));
#36990=CARTESIAN_POINT('Ctrl Pts',(13.7123055934936,4.8,74.9360476097479));
#36991=CARTESIAN_POINT('Ctrl Pts',(13.7935029203389,4.8,74.8119487895258));
#36992=CARTESIAN_POINT('Ctrl Pts',(13.9251658340055,4.8,74.5648727799932));
#36993=CARTESIAN_POINT('Ctrl Pts',(13.980235886818,4.8,74.4412866654118));
#36994=CARTESIAN_POINT('Ctrl Pts',(14.0314999829165,4.8,74.2976442754215));
#36995=CARTESIAN_POINT('',(13.7759884897161,4.8,73.993137535462));
#36996=CARTESIAN_POINT('Origin',(9.31,4.8,78.));
#36997=CARTESIAN_POINT('',(12.8475953086752,4.8,74.3620957389297));
#36998=CARTESIAN_POINT('Ctrl Pts',(13.7759884897161,4.8,73.993137535462));
#36999=CARTESIAN_POINT('Ctrl Pts',(13.7238904004033,4.8,74.0019874509187));
#37000=CARTESIAN_POINT('Ctrl Pts',(13.6730009735598,4.8,74.0118908177042));
#37001=CARTESIAN_POINT('Ctrl Pts',(13.6233744792638,4.8,74.0228803866613));
#37002=CARTESIAN_POINT('Ctrl Pts',(13.5837093243563,4.8,74.0316640608102));
#37003=CARTESIAN_POINT('Ctrl Pts',(13.5448493219531,4.8,74.0411434044381));
#37004=CARTESIAN_POINT('Ctrl Pts',(13.5068268292634,4.8,74.0513101237898));
#37005=CARTESIAN_POINT('Ctrl Pts',(13.4763689303774,4.8,74.0594541692774));
#37006=CARTESIAN_POINT('Ctrl Pts',(13.4464473412981,4.8,74.068039367854));
#37007=CARTESIAN_POINT('Ctrl Pts',(13.4171065775658,4.8,74.0770356343559));
#37008=CARTESIAN_POINT('Ctrl Pts',(13.3850715584932,4.8,74.0868579952051));
#37009=CARTESIAN_POINT('Ctrl Pts',(13.3537280267159,4.8,74.0971707353158));
#37010=CARTESIAN_POINT('Ctrl Pts',(13.3231950184018,4.8,74.1078894398987));
#37011=CARTESIAN_POINT('Ctrl Pts',(13.2966529914007,4.8,74.1172070984644));
#37012=CARTESIAN_POINT('Ctrl Pts',(13.2707283600065,4.8,74.1268276633136));
#37013=CARTESIAN_POINT('Ctrl Pts',(13.2454975479251,4.8,74.1367013261576));
#37014=CARTESIAN_POINT('Ctrl Pts',(13.2249271074216,4.8,74.1447512293248));
#37015=CARTESIAN_POINT('Ctrl Pts',(13.2048188048439,4.8,74.1529687203539));
#37016=CARTESIAN_POINT('Ctrl Pts',(13.1851834763243,4.8,74.1613529364339));
#37017=CARTESIAN_POINT('Ctrl Pts',(13.1637111136978,4.8,74.1705215596035));
#37018=CARTESIAN_POINT('Ctrl Pts',(13.1428011712343,4.8,74.1798921454136));
#37019=CARTESIAN_POINT('Ctrl Pts',(13.122428698542,4.8,74.1894959066136));
#37020=CARTESIAN_POINT('Ctrl Pts',(13.1073100380069,4.8,74.1966229749688));
#37021=CARTESIAN_POINT('Ctrl Pts',(13.0924857119884,4.8,74.2038798290292));
#37022=CARTESIAN_POINT('Ctrl Pts',(13.0779623424873,4.8,74.211265925024));
#37023=CARTESIAN_POINT('Ctrl Pts',(13.0646894097681,4.8,74.2180160910367));
#37024=CARTESIAN_POINT('Ctrl Pts',(13.0516670092769,4.8,74.2248748877425));
#37025=CARTESIAN_POINT('Ctrl Pts',(13.0389304526091,4.8,74.2318175128486));
#37026=CARTESIAN_POINT('Ctrl Pts',(13.0260194633204,4.8,74.2388552201912));
#37027=CARTESIAN_POINT('Ctrl Pts',(13.0134018954141,4.8,74.245979337904));
#37028=CARTESIAN_POINT('Ctrl Pts',(13.0011579161868,4.8,74.2531287727555));
#37029=CARTESIAN_POINT('Ctrl Pts',(12.9841097219238,4.8,74.263083457581));
#37030=CARTESIAN_POINT('Ctrl Pts',(12.9677889833194,4.8,74.273084894711));
#37031=CARTESIAN_POINT('Ctrl Pts',(12.9524860012689,4.8,74.2829061249336));
#37032=CARTESIAN_POINT('Ctrl Pts',(12.941008764731,4.8,74.2902720476006));
#37033=CARTESIAN_POINT('Ctrl Pts',(12.930106960295,4.8,74.2975342041223));
#37034=CARTESIAN_POINT('Ctrl Pts',(12.9198881468665,4.8,74.3046068595292));
#37035=CARTESIAN_POINT('Ctrl Pts',(12.9100174678259,4.8,74.3114385638141));
#37036=CARTESIAN_POINT('Ctrl Pts',(12.9007848525593,4.8,74.3180927859375));
#37037=CARTESIAN_POINT('Ctrl Pts',(12.8922438433448,4.8,74.3245249814216));
#37038=CARTESIAN_POINT('Ctrl Pts',(12.8824463607762,4.8,74.3319034213167));
#37039=CARTESIAN_POINT('Ctrl Pts',(12.8735579224768,4.8,74.3389903348055));
#37040=CARTESIAN_POINT('Ctrl Pts',(12.8656006696037,4.8,74.3457642748448));
#37041=CARTESIAN_POINT('Ctrl Pts',(12.858950393561,4.8,74.3514255968961));
#37042=CARTESIAN_POINT('Ctrl Pts',(12.8529486903123,4.8,74.3568696998768));
#37043=CARTESIAN_POINT('Ctrl Pts',(12.8475953086752,4.8,74.3620957389297));
#37044=CARTESIAN_POINT('',(12.5915348397961,4.8,74.7054546451438));
#37045=CARTESIAN_POINT('',(11.215724076083,4.8,76.5503191845784));
#37046=CARTESIAN_POINT('',(11.9846612632316,4.8,74.1962272508773));
#37047=CARTESIAN_POINT('Origin',(9.3099999999996,4.8,78.0000000000005));
#37048=CARTESIAN_POINT('',(12.2783393423437,4.8,73.8844332675354));
#37049=CARTESIAN_POINT('',(10.5535704330285,4.8,75.7155967313038));
#37050=CARTESIAN_POINT('',(12.4804784574649,4.8,72.906075545245));
#37051=CARTESIAN_POINT('Ctrl Pts',(12.2783393423437,4.8,73.8844332675354));
#37052=CARTESIAN_POINT('Ctrl Pts',(12.3032997730562,4.8,73.847856872409));
#37053=CARTESIAN_POINT('Ctrl Pts',(12.3280901065664,4.8,73.7931055586751));
#37054=CARTESIAN_POINT('Ctrl Pts',(12.3988806442072,4.8,73.6151493612448));
#37055=CARTESIAN_POINT('Ctrl Pts',(12.4327368770971,4.8,73.4707634939834));
#37056=CARTESIAN_POINT('Ctrl Pts',(12.4719545735749,4.8,73.1935566220854));
#37057=CARTESIAN_POINT('Ctrl Pts',(12.4814345554534,4.8,73.0585885935031));
#37058=CARTESIAN_POINT('Ctrl Pts',(12.4804784574649,4.8,72.906075545245));
#37059=CARTESIAN_POINT('',(12.1362287539072,4.8,72.7073228862334));
#37060=CARTESIAN_POINT('Origin',(9.31,4.8,78.));
#37061=CARTESIAN_POINT('',(11.3900156701126,4.8,73.3715593562453));
#37062=CARTESIAN_POINT('Ctrl Pts',(12.1362287539072,4.8,72.7073228862334));
#37063=CARTESIAN_POINT('Ctrl Pts',(12.0902994131742,4.8,72.7334576824571));
#37064=CARTESIAN_POINT('Ctrl Pts',(12.0458661451943,4.8,72.7601690122162));
#37065=CARTESIAN_POINT('Ctrl Pts',(12.0029911486446,4.8,72.7874690897655));
#37066=CARTESIAN_POINT('Ctrl Pts',(11.9687222872374,4.8,72.8092893264821));
#37067=CARTESIAN_POINT('Ctrl Pts',(11.935447954768,4.8,72.8314879003312));
#37068=CARTESIAN_POINT('Ctrl Pts',(11.9031957204388,4.8,72.8540459509127));
#37069=CARTESIAN_POINT('Ctrl Pts',(11.8773600856403,4.8,72.8721160650835));
#37070=CARTESIAN_POINT('Ctrl Pts',(11.8521793004395,4.8,72.8904172987917));
#37071=CARTESIAN_POINT('Ctrl Pts',(11.8276849060244,4.8,72.90890615602));
#37072=CARTESIAN_POINT('Ctrl Pts',(11.8009412807114,4.8,72.9290927775709));
#37073=CARTESIAN_POINT('Ctrl Pts',(11.7750151604701,4.8,72.949503702302));
#37074=CARTESIAN_POINT('Ctrl Pts',(11.7499895311469,4.8,72.9700188934941));
#37075=CARTESIAN_POINT('Ctrl Pts',(11.7282350112657,4.8,72.9878525363126));
#37076=CARTESIAN_POINT('Ctrl Pts',(11.707164253526,4.8,73.0057596561935));
#37077=CARTESIAN_POINT('Ctrl Pts',(11.6868320372831,4.8,73.0236673102102));
#37078=CARTESIAN_POINT('Ctrl Pts',(11.6702553752548,4.8,73.0382672497746));
#37079=CARTESIAN_POINT('Ctrl Pts',(11.654170299247,4.8,73.0528666099356));
#37080=CARTESIAN_POINT('Ctrl Pts',(11.6385866967945,4.8,73.067460873742));
#37081=CARTESIAN_POINT('Ctrl Pts',(11.6215451301536,4.8,73.0834205416036));
#37082=CARTESIAN_POINT('Ctrl Pts',(11.6051011408651,4.8,73.0993776332441));
#37083=CARTESIAN_POINT('Ctrl Pts',(11.5892419586191,4.8,73.1153700125893));
#37084=CARTESIAN_POINT('Ctrl Pts',(11.5774726658493,4.8,73.1272381525525));
#37085=CARTESIAN_POINT('Ctrl Pts',(11.5660243463772,4.8,73.1391275828518));
#37086=CARTESIAN_POINT('Ctrl Pts',(11.5549030368674,4.8,73.1510355276518));
#37087=CARTESIAN_POINT('Ctrl Pts',(11.5447392527121,4.8,73.1619182191707));
#37088=CARTESIAN_POINT('Ctrl Pts',(11.5348480457267,4.8,73.1728173030816));
#37089=CARTESIAN_POINT('Ctrl Pts',(11.5252541150731,4.8,73.1836973955759));
#37090=CARTESIAN_POINT('Ctrl Pts',(11.5155287913938,4.8,73.1947264956381));
#37091=CARTESIAN_POINT('Ctrl Pts',(11.5061087477094,4.8,73.2057364388639));
#37092=CARTESIAN_POINT('Ctrl Pts',(11.4970484215219,4.8,73.2166423975633));
#37093=CARTESIAN_POINT('Ctrl Pts',(11.484433061942,4.8,73.2318275672483));
#37094=CARTESIAN_POINT('Ctrl Pts',(11.472517277305,4.8,73.2468078652383));
#37095=CARTESIAN_POINT('Ctrl Pts',(11.461496236598,4.8,73.2612707308838));
#37096=CARTESIAN_POINT('Ctrl Pts',(11.4532304560678,4.8,73.272117880118));
#37097=CARTESIAN_POINT('Ctrl Pts',(11.4454699147249,4.8,73.2826707117006));
#37098=CARTESIAN_POINT('Ctrl Pts',(11.4382863617921,4.8,73.2928118738022));
#37099=CARTESIAN_POINT('Ctrl Pts',(11.4313475380429,4.8,73.3026075469311));
#37100=CARTESIAN_POINT('Ctrl Pts',(11.4249475956373,4.8,73.3120182107202));
#37101=CARTESIAN_POINT('Ctrl Pts',(11.4191216127486,4.8,73.3209836945166));
#37102=CARTESIAN_POINT('Ctrl Pts',(11.4124385657172,4.8,73.3312680964817));
#37103=CARTESIAN_POINT('Ctrl Pts',(11.4065100329821,4.8,73.3409676417767));
#37104=CARTESIAN_POINT('Ctrl Pts',(11.4013494851028,4.8,73.350054604053));
#37105=CARTESIAN_POINT('Ctrl Pts',(11.3970365560116,4.8,73.3576490348903));
#37106=CARTESIAN_POINT('Ctrl Pts',(11.3932587926791,4.8,73.3648175216196));
#37107=CARTESIAN_POINT('Ctrl Pts',(11.3900156701126,4.8,73.3715593562453));
#37108=CARTESIAN_POINT('',(11.2668331993474,4.8,73.7817890249619));
#37109=CARTESIAN_POINT('',(10.6049748112822,4.8,75.9859496136124));
#37110=CARTESIAN_POINT('',(10.5223925513275,4.8,73.5108347879048));
#37111=CARTESIAN_POINT('Origin',(9.31000000000015,4.8,77.9999999999997));
#37112=CARTESIAN_POINT('',(10.691719852285,4.8,73.1174004638434));
#37113=CARTESIAN_POINT('',(9.6972620259713,4.8,75.428036967767));
#37114=CARTESIAN_POINT('',(10.5470504387829,4.8,72.1289092826028));
#37115=CARTESIAN_POINT('Ctrl Pts',(10.691719852285,4.8,73.1174004638434));
#37116=CARTESIAN_POINT('Ctrl Pts',(10.7026651211628,4.8,73.0744929241743));
#37117=CARTESIAN_POINT('Ctrl Pts',(10.7072343623596,4.8,73.0145647240501));
#37118=CARTESIAN_POINT('Ctrl Pts',(10.7128911037806,4.8,72.8231288094491));
#37119=CARTESIAN_POINT('Ctrl Pts',(10.6953226809553,4.8,72.6758709620368));
#37120=CARTESIAN_POINT('Ctrl Pts',(10.6373649269874,4.8,72.4019684691396));
#37121=CARTESIAN_POINT('Ctrl Pts',(10.6001114115581,4.8,72.2718976636863));
#37122=CARTESIAN_POINT('Ctrl Pts',(10.5470504387829,4.8,72.1289092826028));
#37123=CARTESIAN_POINT('',(10.1555841196958,4.8,72.059883208512));
#37124=CARTESIAN_POINT('Origin',(9.31,4.8,78.));
#37125=CARTESIAN_POINT('',(9.68155544397255,4.8,72.9392812237066));
#37126=CARTESIAN_POINT('Ctrl Pts',(10.1555841196958,4.8,72.059883208512));
#37127=CARTESIAN_POINT('Ctrl Pts',(10.1213632838796,4.8,72.1001506433707));
#37128=CARTESIAN_POINT('Ctrl Pts',(10.0887454826508,4.8,72.1404481555294));
#37129=CARTESIAN_POINT('Ctrl Pts',(10.0577933412008,4.8,72.1807659494182));
#37130=CARTESIAN_POINT('Ctrl Pts',(10.0330541051411,4.8,72.2129909061963));
#37131=CARTESIAN_POINT('Ctrl Pts',(10.009378819543,4.8,72.2452312346535));
#37132=CARTESIAN_POINT('Ctrl Pts',(9.98678694034531,4.8,72.2774597825885));
#37133=CARTESIAN_POINT('Ctrl Pts',(9.96868972816606,4.8,72.303276442863));
#37134=CARTESIAN_POINT('Ctrl Pts',(9.95128692085213,4.8,72.3290863127067));
#37135=CARTESIAN_POINT('Ctrl Pts',(9.93459328090694,4.8,72.3548377315138));
#37136=CARTESIAN_POINT('Ctrl Pts',(9.91636672526524,4.8,72.3829538086114));
#37137=CARTESIAN_POINT('Ctrl Pts',(9.89898508926508,4.8,72.411001058554));
#37138=CARTESIAN_POINT('Ctrl Pts',(9.88248529911423,4.8,72.4388383009022));
#37139=CARTESIAN_POINT('Ctrl Pts',(9.86814220232304,4.8,72.4630369275363));
#37140=CARTESIAN_POINT('Ctrl Pts',(9.85446676240731,4.8,72.4870707395995));
#37141=CARTESIAN_POINT('Ctrl Pts',(9.84148550717457,4.8,72.5108524575166));
#37142=CARTESIAN_POINT('Ctrl Pts',(9.83090201362154,4.8,72.5302414652623));
#37143=CARTESIAN_POINT('Ctrl Pts',(9.82078026165405,4.8,72.5494617962272));
#37144=CARTESIAN_POINT('Ctrl Pts',(9.81112799762775,4.8,72.5685058241284));
#37145=CARTESIAN_POINT('Ctrl Pts',(9.80057269094209,4.8,72.5893315655792));
#37146=CARTESIAN_POINT('Ctrl Pts',(9.79057804217991,4.8,72.6099505026764));
#37147=CARTESIAN_POINT('Ctrl Pts',(9.78114500139984,4.8,72.6304025835768));
#37148=CARTESIAN_POINT('Ctrl Pts',(9.7741446267435,4.8,72.6455803223508));
#37149=CARTESIAN_POINT('Ctrl Pts',(9.76745315005117,4.8,72.660668288163));
#37150=CARTESIAN_POINT('Ctrl Pts',(9.7610752945402,4.8,72.6756618079211));
#37151=CARTESIAN_POINT('Ctrl Pts',(9.75524656128037,4.8,72.6893644117423));
#37152=CARTESIAN_POINT('Ctrl Pts',(9.7496795733032,4.8,72.7029891924912));
#37153=CARTESIAN_POINT('Ctrl Pts',(9.7443854382534,4.8,72.7164944526537));
#37154=CARTESIAN_POINT('Ctrl Pts',(9.73901879774745,4.8,72.7301846731619));
#37155=CARTESIAN_POINT('Ctrl Pts',(9.73393247457399,4.8,72.7437524802262));
#37156=CARTESIAN_POINT('Ctrl Pts',(9.72914861047331,4.8,72.7570995431718));
#37157=CARTESIAN_POINT('Ctrl Pts',(9.72248768404499,4.8,72.7756836422271));
#37158=CARTESIAN_POINT('Ctrl Pts',(9.71641407278451,4.8,72.7938359561415));
#37159=CARTESIAN_POINT('Ctrl Pts',(9.71100427351269,4.8,72.8111960222505));
#37160=CARTESIAN_POINT('Ctrl Pts',(9.70694692405882,4.8,72.8242160718323));
#37161=CARTESIAN_POINT('Ctrl Pts',(9.70326368157836,4.8,72.8367867513079));
#37162=CARTESIAN_POINT('Ctrl Pts',(9.69998183159711,4.8,72.8487732463486));
#37163=CARTESIAN_POINT('Ctrl Pts',(9.69681178764907,4.8,72.8603513855929));
#37164=CARTESIAN_POINT('Ctrl Pts',(9.69401644557314,4.8,72.8713834261291));
#37165=CARTESIAN_POINT('Ctrl Pts',(9.6916081884937,4.8,72.8818008285971));
#37166=CARTESIAN_POINT('Ctrl Pts',(9.68884565114532,4.8,72.8937507419333));
#37167=CARTESIAN_POINT('Ctrl Pts',(9.68659209254914,4.8,72.9048930106879));
#37168=CARTESIAN_POINT('Ctrl Pts',(9.68485068791891,4.8,72.9151969734135));
#37169=CARTESIAN_POINT('Ctrl Pts',(9.68339530857426,4.8,72.9238085127757));
#37170=CARTESIAN_POINT('Ctrl Pts',(9.68229713908583,4.8,72.9318367581203));
#37171=CARTESIAN_POINT('Ctrl Pts',(9.68155544397255,4.8,72.9392812237066));
#37172=CARTESIAN_POINT('',(9.70610859527519,4.8,73.3669019025333));
#37173=CARTESIAN_POINT('',(9.83803247244813,4.8,75.6645042434626));
#37174=CARTESIAN_POINT('',(8.91389140472481,4.8,73.3669019025333));
#37175=CARTESIAN_POINT('Origin',(9.31,4.8,77.9999999999998));
#37176=CARTESIAN_POINT('',(8.93844455602745,4.8,72.9392812237066));
#37177=CARTESIAN_POINT('',(8.79424410320319,4.8,75.4506939040492));
#37178=CARTESIAN_POINT('',(8.46441588028028,4.8,72.0598832085154));
#37179=CARTESIAN_POINT('Ctrl Pts',(8.93844455602745,4.8,72.9392812237066));
#37180=CARTESIAN_POINT('Ctrl Pts',(8.93405450155534,4.8,72.8952178225727));
#37181=CARTESIAN_POINT('Ctrl Pts',(8.91785153193323,4.8,72.8373409623484));
#37182=CARTESIAN_POINT('Ctrl Pts',(8.85769219205878,4.8,72.6555153283963));
#37183=CARTESIAN_POINT('Ctrl Pts',(8.79081812458728,4.8,72.5231469699846));
#37184=CARTESIAN_POINT('Ctrl Pts',(8.64267548147068,4.8,72.2855855384878));
#37185=CARTESIAN_POINT('Ctrl Pts',(8.56318179199311,4.8,72.1761004142322));
#37186=CARTESIAN_POINT('Ctrl Pts',(8.46441588028027,4.8,72.0598832085154));
#37187=CARTESIAN_POINT('',(8.07294956118024,4.8,72.1289092826106));
#37188=CARTESIAN_POINT('Origin',(9.31,4.8,78.));
#37189=CARTESIAN_POINT('',(7.92828014771504,4.8,73.1174004638434));
#37190=CARTESIAN_POINT('Ctrl Pts',(8.07294956118024,4.8,72.1289092826106));
#37191=CARTESIAN_POINT('Ctrl Pts',(8.01079867475487,4.8,72.2963931067747));
#37192=CARTESIAN_POINT('Ctrl Pts',(7.96245928031717,4.8,72.4681817504002));
#37193=CARTESIAN_POINT('Ctrl Pts',(7.91818215761049,4.8,72.7469888411323));
#37194=CARTESIAN_POINT('Ctrl Pts',(7.91099972253224,4.8,72.8362124135078));
#37195=CARTESIAN_POINT('Ctrl Pts',(7.9104099657788,4.8,72.9888516549209));
#37196=CARTESIAN_POINT('Ctrl Pts',(7.91537633853598,4.8,73.0668150730702));
#37197=CARTESIAN_POINT('Ctrl Pts',(7.92828014771504,4.8,73.1174004638434));
#37198=CARTESIAN_POINT('',(8.09760744867254,4.8,73.5108347879048));
#37199=CARTESIAN_POINT('',(9.00740162450745,4.8,75.6247541297977));
#37200=CARTESIAN_POINT('',(7.3531668006526,4.8,73.7817890249619));
#37201=CARTESIAN_POINT('Origin',(9.30999999999986,4.8,77.9999999999997));
#37202=CARTESIAN_POINT('',(7.22998432988738,4.8,73.3715593562453));
#37203=CARTESIAN_POINT('',(7.95343395333514,4.8,75.7808347792541));
#37204=CARTESIAN_POINT('',(6.48377124607659,4.8,72.7073228862421));
#37205=CARTESIAN_POINT('Ctrl Pts',(7.22998432988738,4.8,73.3715593562453));
#37206=CARTESIAN_POINT('Ctrl Pts',(7.21078845692561,4.8,73.3316547895226));
#37207=CARTESIAN_POINT('Ctrl Pts',(7.17576759298895,4.8,73.2828100723767));
#37208=CARTESIAN_POINT('Ctrl Pts',(7.05704827823986,4.8,73.1325255745702));
#37209=CARTESIAN_POINT('Ctrl Pts',(6.94893456556166,4.8,73.0310122828858));
#37210=CARTESIAN_POINT('Ctrl Pts',(6.72847522208608,4.8,72.858445326573));
#37211=CARTESIAN_POINT('Ctrl Pts',(6.61632947039997,4.8,72.7827514058996));
#37212=CARTESIAN_POINT('Ctrl Pts',(6.48377124607659,4.8,72.7073228862421));
#37213=CARTESIAN_POINT('',(6.13952154251132,4.8,72.9060755452598));
#37214=CARTESIAN_POINT('Origin',(9.31,4.8,78.));
#37215=CARTESIAN_POINT('',(6.34166065765632,4.8,73.8844332675354));
#37216=CARTESIAN_POINT('Ctrl Pts',(6.13952154251132,4.8,72.9060755452598));
#37217=CARTESIAN_POINT('Ctrl Pts',(6.13919026958786,4.8,72.9589189192305));
#37218=CARTESIAN_POINT('Ctrl Pts',(6.14010632567283,4.8,73.0107549229785));
#37219=CARTESIAN_POINT('Ctrl Pts',(6.14231138804498,4.8,73.0615357979665));
#37220=CARTESIAN_POINT('Ctrl Pts',(6.14407383648731,4.8,73.1021236176823));
#37221=CARTESIAN_POINT('Ctrl Pts',(6.14666119885485,4.8,73.1420393187381));
#37222=CARTESIAN_POINT('Ctrl Pts',(6.15007092616186,4.8,73.1812495953145));
#37223=CARTESIAN_POINT('Ctrl Pts',(6.15280228663195,4.8,73.2126589690911));
#37224=CARTESIAN_POINT('Ctrl Pts',(6.15606122731895,4.8,73.2436167862334));
#37225=CARTESIAN_POINT('Ctrl Pts',(6.15982585015175,4.8,73.2740739832677));
#37226=CARTESIAN_POINT('Ctrl Pts',(6.16393616428756,4.8,73.3073279513457));
#37227=CARTESIAN_POINT('Ctrl Pts',(6.16864948314967,4.8,73.3399860909232));
#37228=CARTESIAN_POINT('Ctrl Pts',(6.17390334482274,4.8,73.3719165158161));
#37229=CARTESIAN_POINT('Ctrl Pts',(6.17847047257082,4.8,73.3996733047479));
#37230=CARTESIAN_POINT('Ctrl Pts',(6.18344311440971,4.8,73.4268746768222));
#37231=CARTESIAN_POINT('Ctrl Pts',(6.18878548958805,4.8,73.4534367202513));
#37232=CARTESIAN_POINT('Ctrl Pts',(6.1931410770833,4.8,73.4750925007508));
#37233=CARTESIAN_POINT('Ctrl Pts',(6.19774195581625,4.8,73.4963222655652));
#37234=CARTESIAN_POINT('Ctrl Pts',(6.20258915775713,4.8,73.5171151933554));
#37235=CARTESIAN_POINT('Ctrl Pts',(6.20788985257399,4.8,73.5398534588348));
#37236=CARTESIAN_POINT('Ctrl Pts',(6.21348710503892,4.8,73.5620729189504));
#37237=CARTESIAN_POINT('Ctrl Pts',(6.21940732112328,4.8,73.5838035650851));
#37238=CARTESIAN_POINT('Ctrl Pts',(6.22380078545766,4.8,73.5999301417836));
#37239=CARTESIAN_POINT('Ctrl Pts',(6.22837317441562,4.8,73.6157893926149));
#37240=CARTESIAN_POINT('Ctrl Pts',(6.23312510238621,4.8,73.6313747017585));
#37241=CARTESIAN_POINT('Ctrl Pts',(6.23746789761259,4.8,73.6456181428564));
#37242=CARTESIAN_POINT('Ctrl Pts',(6.2419611776524,4.8,73.6596337213974));
#37243=CARTESIAN_POINT('Ctrl Pts',(6.2465866488109,4.8,73.6733823553783));
#37244=CARTESIAN_POINT('Ctrl Pts',(6.25127546773714,4.8,73.6873192826687));
#37245=CARTESIAN_POINT('Ctrl Pts',(6.25610033635251,4.8,73.7009822513204));
#37246=CARTESIAN_POINT('Ctrl Pts',(6.26101501047773,4.8,73.7142817032348));
#37247=CARTESIAN_POINT('Ctrl Pts',(6.26785807347238,4.8,73.7327995103013));
#37248=CARTESIAN_POINT('Ctrl Pts',(6.27487349986076,4.8,73.7506090318451));
#37249=CARTESIAN_POINT('Ctrl Pts',(6.28188818866958,4.8,73.7673849662274));
#37250=CARTESIAN_POINT('Ctrl Pts',(6.28714920527619,4.8,73.7799669170141));
#37251=CARTESIAN_POINT('Ctrl Pts',(6.29240795491918,4.8,73.7919641589943));
#37252=CARTESIAN_POINT('Ctrl Pts',(6.29759868254043,4.8,73.8032558795968));
#37253=CARTESIAN_POINT('Ctrl Pts',(6.3026125724438,4.8,73.8141629138417));
#37254=CARTESIAN_POINT('Ctrl Pts',(6.3075624751535,4.8,73.824410758489));
#37255=CARTESIAN_POINT('Ctrl Pts',(6.31241382043933,4.8,73.8339389496217));
#37256=CARTESIAN_POINT('Ctrl Pts',(6.31797885022995,4.8,73.84486883904));
#37257=CARTESIAN_POINT('Ctrl Pts',(6.32341463643833,4.8,73.8548528716026));
#37258=CARTESIAN_POINT('Ctrl Pts',(6.32870390261798,4.8,73.8638655182879));
#37259=CARTESIAN_POINT('Ctrl Pts',(6.33312440839882,4.8,73.8713978404324));
#37260=CARTESIAN_POINT('Ctrl Pts',(6.33744361862487,4.8,73.8782537232953));
#37261=CARTESIAN_POINT('Ctrl Pts',(6.34166065765632,4.8,73.8844332675354));
#37262=CARTESIAN_POINT('',(6.63533873676838,4.8,74.1962272508773));
#37263=CARTESIAN_POINT('',(8.21326860652757,4.8,75.8714937229748));
#37264=CARTESIAN_POINT('',(6.02846516020394,4.8,74.7054546451438));
#37265=CARTESIAN_POINT('Origin',(9.30999999999964,4.8,77.9999999999996));
#37266=CARTESIAN_POINT('',(5.77240469132477,4.8,74.3620957389297));
#37267=CARTESIAN_POINT('',(7.27624568947745,4.8,76.3786397314713));
#37268=CARTESIAN_POINT('',(4.84401151027683,4.8,73.9931375354699));
#37269=CARTESIAN_POINT('Ctrl Pts',(5.77240469132477,4.8,74.3620957389297));
#37270=CARTESIAN_POINT('Ctrl Pts',(5.74071830526386,4.8,74.3311630869991));
#37271=CARTESIAN_POINT('Ctrl Pts',(5.69110358025555,4.8,74.2972419075011));
#37272=CARTESIAN_POINT('Ctrl Pts',(5.52814359189328,4.8,74.1966250715416));
#37273=CARTESIAN_POINT('Ctrl Pts',(5.39183034320095,4.8,74.1382108478629));
#37274=CARTESIAN_POINT('Ctrl Pts',(5.12564495012972,4.8,74.0514524887457));
#37275=CARTESIAN_POINT('Ctrl Pts',(4.99437356897251,4.8,74.0186795759735));
#37276=CARTESIAN_POINT('Ctrl Pts',(4.84401151027683,4.8,73.9931375354699));
#37277=CARTESIAN_POINT('',(4.58850001706627,4.8,74.2976442754434));
#37278=CARTESIAN_POINT('Origin',(9.31,4.8,78.));
#37279=CARTESIAN_POINT('',(5.11306670030725,4.8,75.1478641584586));
#37280=CARTESIAN_POINT('Ctrl Pts',(4.58850001706627,4.8,74.2976442754434));
#37281=CARTESIAN_POINT('Ctrl Pts',(4.60626222068121,4.8,74.3474141060367));
#37282=CARTESIAN_POINT('Ctrl Pts',(4.6248519892365,4.8,74.3958107066347));
#37283=CARTESIAN_POINT('Ctrl Pts',(4.64429215220695,4.8,74.4427749443995));
#37284=CARTESIAN_POINT('Ctrl Pts',(4.65983016360494,4.8,74.4803122254808));
#37285=CARTESIAN_POINT('Ctrl Pts',(4.67591346239461,4.8,74.5169357844687));
#37286=CARTESIAN_POINT('Ctrl Pts',(4.69252826205227,4.8,74.5526151959383));
#37287=CARTESIAN_POINT('Ctrl Pts',(4.70583753983714,4.8,74.5811961724311));
#37288=CARTESIAN_POINT('Ctrl Pts',(4.71948813939692,4.8,74.6091723814237));
#37289=CARTESIAN_POINT('Ctrl Pts',(4.73344270257734,4.8,74.6365052079171));
#37290=CARTESIAN_POINT('Ctrl Pts',(4.74867866115537,4.8,74.6663479057422));
#37291=CARTESIAN_POINT('Ctrl Pts',(4.76427747346707,4.8,74.6954244681821));
#37292=CARTESIAN_POINT('Ctrl Pts',(4.78013533678421,4.8,74.7236323260018));
#37293=CARTESIAN_POINT('Ctrl Pts',(4.79392041401104,4.8,74.7481531262302));
#37294=CARTESIAN_POINT('Ctrl Pts',(4.80789658608741,4.8,74.7720133113463));
#37295=CARTESIAN_POINT('Ctrl Pts',(4.8220015305823,4.8,74.7951462677966));
#37296=CARTESIAN_POINT('Ctrl Pts',(4.83350115716757,4.8,74.8140063463377));
#37297=CARTESIAN_POINT('Ctrl Pts',(4.84508557617433,4.8,74.8323822065386));
#37298=CARTESIAN_POINT('Ctrl Pts',(4.85675205622014,4.8,74.8502633267103));
#37299=CARTESIAN_POINT('Ctrl Pts',(4.86951002512632,4.8,74.8698173630831));
#37300=CARTESIAN_POINT('Ctrl Pts',(4.88236922518497,4.8,74.8887824531661));
#37301=CARTESIAN_POINT('Ctrl Pts',(4.8953647275517,4.8,74.9071777482689));
#37302=CARTESIAN_POINT('Ctrl Pts',(4.90500884766322,4.8,74.9208291201398));
#37303=CARTESIAN_POINT('Ctrl Pts',(4.91472967109205,4.8,74.9341680920388));
#37304=CARTESIAN_POINT('Ctrl Pts',(4.92452551243159,4.8,74.9471882369959));
#37305=CARTESIAN_POINT('Ctrl Pts',(4.93347794881098,4.8,74.9590873700401));
#37306=CARTESIAN_POINT('Ctrl Pts',(4.94249386107474,4.8,74.970720913485));
#37307=CARTESIAN_POINT('Ctrl Pts',(4.95154269194146,4.8,74.9820583990737));
#37308=CARTESIAN_POINT('Ctrl Pts',(4.96071545031099,4.8,74.9935511562436));
#37309=CARTESIAN_POINT('Ctrl Pts',(4.96992235419727,4.8,75.0047399447727));
#37310=CARTESIAN_POINT('Ctrl Pts',(4.97908931761474,4.8,75.0155564240187));
#37311=CARTESIAN_POINT('Ctrl Pts',(4.99185315650524,4.8,75.030617005388));
#37312=CARTESIAN_POINT('Ctrl Pts',(5.00453671609312,4.8,75.0449530643228));
#37313=CARTESIAN_POINT('Ctrl Pts',(5.01686607495472,4.8,75.0583181212877));
#37314=CARTESIAN_POINT('Ctrl Pts',(5.02611309410092,4.8,75.0683419140114));
#37315=CARTESIAN_POINT('Ctrl Pts',(5.03515800080879,4.8,75.0778170355269));
#37316=CARTESIAN_POINT('Ctrl Pts',(5.0438976852005,4.8,75.0866524487053));
#37317=CARTESIAN_POINT('Ctrl Pts',(5.05233962593721,4.8,75.0951868569394));
#37318=CARTESIAN_POINT('Ctrl Pts',(5.06049598226297,4.8,75.1031237144866));
#37319=CARTESIAN_POINT('Ctrl Pts',(5.0683135889096,4.8,75.1104180275667));
#37320=CARTESIAN_POINT('Ctrl Pts',(5.07728124869061,4.8,75.1187854117285));
#37321=CARTESIAN_POINT('Ctrl Pts',(5.0858039571351,4.8,75.1263081850942));
#37322=CARTESIAN_POINT('Ctrl Pts',(5.09385674825335,4.8,75.1329682671262));
#37323=CARTESIAN_POINT('Ctrl Pts',(5.1005868709652,4.8,75.1385344327809));
#37324=CARTESIAN_POINT('Ctrl Pts',(5.10699045111816,4.8,75.1434995985332));
#37325=CARTESIAN_POINT('Ctrl Pts',(5.11306670030725,4.8,75.1478641584586));
#37326=CARTESIAN_POINT('',(5.49567364700612,4.8,75.340410845101));
#37327=CARTESIAN_POINT('',(7.55141758063195,4.8,76.3749625865681));
#37328=CARTESIAN_POINT('',(5.09956505173093,4.8,76.0264910574324));
#37329=CARTESIAN_POINT('Origin',(9.30999999999911,4.8,77.9999999999995));
#37330=CARTESIAN_POINT('',(4.7415112563347,4.8,75.7914170652479));
#37331=CARTESIAN_POINT('',(6.84435821048571,4.8,77.1720046608023));
#37332=CARTESIAN_POINT('',(3.74291589727828,4.8,75.7622389329459));
#37333=CARTESIAN_POINT('Ctrl Pts',(4.7415112563347,4.8,75.7914170652479));
#37334=CARTESIAN_POINT('Ctrl Pts',(4.70115619977021,4.8,75.7731872611718));
#37335=CARTESIAN_POINT('Ctrl Pts',(4.64293187777709,4.8,75.7582810147208));
#37336=CARTESIAN_POINT('Ctrl Pts',(4.45538660771444,4.8,75.7194677169205));
#37337=CARTESIAN_POINT('Ctrl Pts',(4.30731521231246,4.8,75.7111981783558));
#37338=CARTESIAN_POINT('Ctrl Pts',(4.02750965317559,4.8,75.7207127544803));
#37339=CARTESIAN_POINT('Ctrl Pts',(3.89294590785691,4.8,75.7348137468304));
#37340=CARTESIAN_POINT('Ctrl Pts',(3.74291589727828,4.8,75.7622389329459));
#37341=CARTESIAN_POINT('',(3.60696107145241,4.8,76.1357717469497));
#37342=CARTESIAN_POINT('Origin',(9.31,4.8,78.));
#37343=CARTESIAN_POINT('',(4.39068483903982,4.8,76.7553047249138));
#37344=CARTESIAN_POINT('Ctrl Pts',(3.60696107145242,4.8,76.1357717469498));
#37345=CARTESIAN_POINT('Ctrl Pts',(3.6406743677089,4.8,76.1764650580725));
#37346=CARTESIAN_POINT('Ctrl Pts',(3.67469564829431,4.8,76.215584911225));
#37347=CARTESIAN_POINT('Ctrl Pts',(3.70902614130493,4.8,76.253067931571));
#37348=CARTESIAN_POINT('Ctrl Pts',(3.7364656004989,4.8,76.2830271228629));
#37349=CARTESIAN_POINT('Ctrl Pts',(3.76410495085053,4.8,76.3119411971029));
#37350=CARTESIAN_POINT('Ctrl Pts',(3.79192083116205,4.8,76.3397862790184));
#37351=CARTESIAN_POINT('Ctrl Pts',(3.8142027312811,4.8,76.3620915710709));
#37352=CARTESIAN_POINT('Ctrl Pts',(3.83659852629453,4.8,76.3837118286243));
#37353=CARTESIAN_POINT('Ctrl Pts',(3.85905990391048,4.8,76.4046235426909));
#37354=CARTESIAN_POINT('Ctrl Pts',(3.88358382515552,4.8,76.4274555006248));
#37355=CARTESIAN_POINT('Ctrl Pts',(3.90818668364436,4.8,76.4494434235343));
#37356=CARTESIAN_POINT('Ctrl Pts',(3.93273585598364,4.8,76.4705264304943));
#37357=CARTESIAN_POINT('Ctrl Pts',(3.9540761991713,4.8,76.4888536717444));
#37358=CARTESIAN_POINT('Ctrl Pts',(3.97537016910973,4.8,76.5064947795499));
#37359=CARTESIAN_POINT('Ctrl Pts',(3.99653641868867,4.8,76.5234084731701));
#37360=CARTESIAN_POINT('Ctrl Pts',(4.01379305985171,4.8,76.537198046068));
#37361=CARTESIAN_POINT('Ctrl Pts',(4.0309637674028,4.8,76.5505036018421));
#37362=CARTESIAN_POINT('Ctrl Pts',(4.04804237604851,4.8,76.563316187525));
#37363=CARTESIAN_POINT('Ctrl Pts',(4.06671882044551,4.8,76.5773274895609));
#37364=CARTESIAN_POINT('Ctrl Pts',(4.08528895950369,4.8,76.5907507399687));
#37365=CARTESIAN_POINT('Ctrl Pts',(4.10379229946702,4.8,76.6035919400525));
#37366=CARTESIAN_POINT('Ctrl Pts',(4.11752385220946,4.8,76.6131215501973));
#37367=CARTESIAN_POINT('Ctrl Pts',(4.13122063540912,4.8,76.6223313663111));
#37368=CARTESIAN_POINT('Ctrl Pts',(4.14487886714958,4.8,76.6312159254611));
#37369=CARTESIAN_POINT('Ctrl Pts',(4.15736114877002,4.8,76.6393355394413));
#37370=CARTESIAN_POINT('Ctrl Pts',(4.16981224121807,4.8,76.6471838708035));
#37371=CARTESIAN_POINT('Ctrl Pts',(4.18219300928576,4.8,76.6547427399577));
#37372=CARTESIAN_POINT('Ctrl Pts',(4.19474333702386,4.8,76.6624051309092));
#37373=CARTESIAN_POINT('Ctrl Pts',(4.207221787657,4.8,76.6697702063222));
#37374=CARTESIAN_POINT('Ctrl Pts',(4.21953536925903,4.8,76.6767990859001));
#37375=CARTESIAN_POINT('Ctrl Pts',(4.23668047682952,4.8,76.6865859131902));
#37376=CARTESIAN_POINT('Ctrl Pts',(4.25350234527019,4.8,76.6957193692272));
#37377=CARTESIAN_POINT('Ctrl Pts',(4.2696592716686,4.8,76.7040615256509));
#37378=CARTESIAN_POINT('Ctrl Pts',(4.2817769664674,4.8,76.7103181429686));
#37379=CARTESIAN_POINT('Ctrl Pts',(4.29351708109353,4.8,76.7161283045197));
#37380=CARTESIAN_POINT('Ctrl Pts',(4.30475158741952,4.8,76.7214417290397));
#37381=CARTESIAN_POINT('Ctrl Pts',(4.31560335638421,4.8,76.7265741357187));
#37382=CARTESIAN_POINT('Ctrl Pts',(4.32598238941678,4.8,76.731242704048));
#37383=CARTESIAN_POINT('Ctrl Pts',(4.33582333872569,4.8,76.7354233372979));
#37384=CARTESIAN_POINT('Ctrl Pts',(4.34711199630289,4.8,76.7402189861455));
#37385=CARTESIAN_POINT('Ctrl Pts',(4.35769366250113,4.8,76.7443731427938));
#37386=CARTESIAN_POINT('Ctrl Pts',(4.36753869305379,4.8,76.7478773559685));
#37387=CARTESIAN_POINT('Ctrl Pts',(4.37576668082011,4.8,76.7508060033686));
#37388=CARTESIAN_POINT('Ctrl Pts',(4.38348226484115,4.8,76.7532815796966));
#37389=CARTESIAN_POINT('Ctrl Pts',(4.39068483903982,4.8,76.7553047249138));
#37390=CARTESIAN_POINT('',(4.81607260887647,4.8,76.805380142761));
#37391=CARTESIAN_POINT('',(7.10167754842447,4.8,77.0744349452193));
#37392=CARTESIAN_POINT('',(4.67850553742098,4.8,77.5855617740846));
#37393=CARTESIAN_POINT('Origin',(9.3100000000004,4.8,78.0000000000001));
#37394=CARTESIAN_POINT('',(4.2616449875437,4.8,77.4871260887099));
#37395=CARTESIAN_POINT('',(6.70986352030667,4.8,78.0652380479502));
#37396=CARTESIAN_POINT('',(3.31329278849671,4.8,77.8012473408872));
#37397=CARTESIAN_POINT('Ctrl Pts',(4.2616449875437,4.8,77.4871260887099));
#37398=CARTESIAN_POINT('Ctrl Pts',(4.21748867968916,4.8,77.4837979186763));
#37399=CARTESIAN_POINT('Ctrl Pts',(4.15767747875508,4.8,77.4897045193291));
#37400=CARTESIAN_POINT('Ctrl Pts',(3.9644915235101,4.8,77.5179129865806));
#37401=CARTESIAN_POINT('Ctrl Pts',(3.82580661557927,4.8,77.5619464956297));
#37402=CARTESIAN_POINT('Ctrl Pts',(3.56890774902052,4.8,77.6624620772996));
#37403=CARTESIAN_POINT('Ctrl Pts',(3.43851412071864,4.8,77.7279002925011));
#37404=CARTESIAN_POINT('Ctrl Pts',(3.31329278849671,4.8,77.8012473408872));
#37405=CARTESIAN_POINT('Origin',(9.31,4.8,78.));
#37406=CARTESIAN_POINT('Origin',(9.31,9.325,78.));
#37407=CARTESIAN_POINT('',(3.06,13.85,78.));
#37408=CARTESIAN_POINT('',(3.06,9.325,78.));
#37409=CARTESIAN_POINT('Origin',(9.31,13.85,78.));
#37410=CARTESIAN_POINT('Origin',(12.21,23.,78.));
#37411=CARTESIAN_POINT('',(6.41,23.,78.));
#37412=CARTESIAN_POINT('Origin',(9.31,23.,78.));
#37413=CARTESIAN_POINT('Origin',(9.31,22.95,78.));
#37414=CARTESIAN_POINT('',(6.31,22.9,78.));
#37415=CARTESIAN_POINT('Origin',(9.31,22.9,78.));
#37416=CARTESIAN_POINT('',(6.36,22.95,78.));
#37417=CARTESIAN_POINT('Origin',(9.31,18.45,78.));
#37418=CARTESIAN_POINT('',(6.31,14.,78.));
#37419=CARTESIAN_POINT('Origin',(9.31,14.,78.));
#37420=CARTESIAN_POINT('',(6.31,18.45,78.));
#37421=CARTESIAN_POINT('Origin',(15.41,14.,78.));
#37422=CARTESIAN_POINT('',(3.21,14.,78.));
#37423=CARTESIAN_POINT('Origin',(9.31,14.,78.));
#37424=CARTESIAN_POINT('Origin',(9.31,13.925,78.));
#37425=CARTESIAN_POINT('',(3.135,13.925,78.));
#37426=CARTESIAN_POINT('Origin',(9.31,-13.925,78.));
#37427=CARTESIAN_POINT('',(3.21,-14.,78.));
#37428=CARTESIAN_POINT('Origin',(9.31,-14.,78.));
#37429=CARTESIAN_POINT('',(3.135,-13.925,78.));
#37430=CARTESIAN_POINT('Origin',(12.31,-14.,78.));
#37431=CARTESIAN_POINT('',(6.31,-14.,78.));
#37432=CARTESIAN_POINT('Origin',(9.31,-14.,78.));
#37433=CARTESIAN_POINT('Origin',(9.31,-16.2,78.));
#37434=CARTESIAN_POINT('',(6.31,-18.4,78.));
#37435=CARTESIAN_POINT('Origin',(9.31,-18.4,78.));
#37436=CARTESIAN_POINT('',(6.31,-16.2,78.));
#37437=CARTESIAN_POINT('Origin',(9.31,-18.45,78.));
#37438=CARTESIAN_POINT('',(6.41,-18.5,78.));
#37439=CARTESIAN_POINT('Origin',(9.31,-18.5,78.));
#37440=CARTESIAN_POINT('',(6.36,-18.45,78.));
#37441=CARTESIAN_POINT('Origin',(9.31,-18.5,78.));
#37442=CARTESIAN_POINT('Ctrl Pts',(4.55037293434634,-5.,81.8152261002327));
#37443=CARTESIAN_POINT('Ctrl Pts',(4.55037293434634,5.,81.8152261002327));
#37444=CARTESIAN_POINT('Ctrl Pts',(4.55326576923268,-5.,81.8061728189788));
#37445=CARTESIAN_POINT('Ctrl Pts',(4.55326576923268,5.,81.8061728189788));
#37446=CARTESIAN_POINT('Ctrl Pts',(4.55909298521487,-5.,81.7881352345572));
#37447=CARTESIAN_POINT('Ctrl Pts',(4.55909298521487,5.,81.7881352345572));
#37448=CARTESIAN_POINT('Ctrl Pts',(4.56795844777182,-5.,81.7612857920655));
#37449=CARTESIAN_POINT('Ctrl Pts',(4.56795844777182,5.,81.7612857920655));
#37450=CARTESIAN_POINT('Ctrl Pts',(4.5800287934221,-5.,81.7259011540785));
#37451=CARTESIAN_POINT('Ctrl Pts',(4.5800287934221,5.,81.7259011540785));
#37452=CARTESIAN_POINT('Ctrl Pts',(4.59553572302973,-5.,81.6823663399517));
#37453=CARTESIAN_POINT('Ctrl Pts',(4.59553572302973,5.,81.6823663399517));
#37454=CARTESIAN_POINT('Ctrl Pts',(4.61146542604692,-5.,81.6395347836739));
#37455=CARTESIAN_POINT('Ctrl Pts',(4.61146542604692,5.,81.6395347836739));
#37456=CARTESIAN_POINT('Ctrl Pts',(4.62782195277065,-5.,81.5974152138272));
#37457=CARTESIAN_POINT('Ctrl Pts',(4.62782195277065,5.,81.5974152138272));
#37458=CARTESIAN_POINT('Ctrl Pts',(4.64460884258077,-5.,81.5560168849901));
#37459=CARTESIAN_POINT('Ctrl Pts',(4.64460884258077,5.,81.5560168849901));
#37460=CARTESIAN_POINT('Ctrl Pts',(4.66182827725197,-5.,81.51534844747));
#37461=CARTESIAN_POINT('Ctrl Pts',(4.66182827725197,5.,81.51534844747));
#37462=CARTESIAN_POINT('Ctrl Pts',(4.6794801351961,-5.,81.4754169688554));
#37463=CARTESIAN_POINT('Ctrl Pts',(4.6794801351961,5.,81.4754169688554));
#37464=CARTESIAN_POINT('Ctrl Pts',(4.69756020902606,-5.,81.4362308703527));
#37465=CARTESIAN_POINT('Ctrl Pts',(4.69756020902606,5.,81.4362308703527));
#37466=CARTESIAN_POINT('Ctrl Pts',(4.71605851282859,-5.,81.397802395678));
#37467=CARTESIAN_POINT('Ctrl Pts',(4.71605851282859,5.,81.397802395678));
#37468=CARTESIAN_POINT('Ctrl Pts',(4.73495715972825,-5.,81.3601503543456));
#37469=CARTESIAN_POINT('Ctrl Pts',(4.73495715972825,5.,81.3601503543456));
#37470=CARTESIAN_POINT('Ctrl Pts',(4.7542288770199,-5.,81.3233020975585));
#37471=CARTESIAN_POINT('Ctrl Pts',(4.7542288770199,5.,81.3233020975585));
#37472=CARTESIAN_POINT('Ctrl Pts',(4.77383361228162,-5.,81.2872970095592));
#37473=CARTESIAN_POINT('Ctrl Pts',(4.77383361228162,5.,81.2872970095592));
#37474=CARTESIAN_POINT('Ctrl Pts',(4.79372122786719,-5.,81.2521844855106));
#37475=CARTESIAN_POINT('Ctrl Pts',(4.79372122786719,5.,81.2521844855106));
#37476=CARTESIAN_POINT('Ctrl Pts',(4.81384166090125,-5.,81.2180152029093));
#37477=CARTESIAN_POINT('Ctrl Pts',(4.81384166090125,5.,81.2180152029093));
#37478=CARTESIAN_POINT('Ctrl Pts',(4.8341534505068,-5.,81.184833647465));
#37479=CARTESIAN_POINT('Ctrl Pts',(4.8341534505068,5.,81.184833647465));
#37480=CARTESIAN_POINT('Ctrl Pts',(4.85463221422933,-5.,81.152670529545));
#37481=CARTESIAN_POINT('Ctrl Pts',(4.85463221422933,5.,81.152670529545));
#37482=CARTESIAN_POINT('Ctrl Pts',(4.87528087827813,-5.,81.1215334547639));
#37483=CARTESIAN_POINT('Ctrl Pts',(4.87528087827813,5.,81.1215334547639));
#37484=CARTESIAN_POINT('Ctrl Pts',(4.89613444857731,-5.,81.091402307974));
#37485=CARTESIAN_POINT('Ctrl Pts',(4.89613444857731,5.,81.091402307974));
#37486=CARTESIAN_POINT('Ctrl Pts',(4.91722853182858,-5.,81.0622569233023));
#37487=CARTESIAN_POINT('Ctrl Pts',(4.91722853182858,5.,81.0622569233023));
#37488=CARTESIAN_POINT('Ctrl Pts',(4.93857071576868,-5.,81.0341019923514));
#37489=CARTESIAN_POINT('Ctrl Pts',(4.93857071576868,5.,81.0341019923514));
#37490=CARTESIAN_POINT('Ctrl Pts',(4.96011273429653,-5.,81.0069911329727));
#37491=CARTESIAN_POINT('Ctrl Pts',(4.96011273429653,5.,81.0069911329727));
#37492=CARTESIAN_POINT('Ctrl Pts',(4.98171699052596,-5.,80.981055696686));
#37493=CARTESIAN_POINT('Ctrl Pts',(4.98171699052596,5.,80.981055696686));
#37494=CARTESIAN_POINT('Ctrl Pts',(5.00313954967413,-5.,80.9565189839515));
#37495=CARTESIAN_POINT('Ctrl Pts',(5.00313954967413,5.,80.9565189839515));
#37496=CARTESIAN_POINT('Ctrl Pts',(5.02408529635557,-5.,80.9336473146961));
#37497=CARTESIAN_POINT('Ctrl Pts',(5.02408529635557,5.,80.9336473146961));
#37498=CARTESIAN_POINT('Ctrl Pts',(5.0442546199981,-5.,80.9127081471617));
#37499=CARTESIAN_POINT('Ctrl Pts',(5.0442546199981,5.,80.9127081471617));
#37500=CARTESIAN_POINT('Ctrl Pts',(5.06338898078167,-5.,80.8939293165779));
#37501=CARTESIAN_POINT('Ctrl Pts',(5.06338898078167,5.,80.8939293165779));
#37502=CARTESIAN_POINT('Ctrl Pts',(5.0813283019591,-5.,80.8774468502762));
#37503=CARTESIAN_POINT('Ctrl Pts',(5.0813283019591,5.,80.8774468502762));
#37504=CARTESIAN_POINT('Ctrl Pts',(5.09466658957796,-5.,80.8661420261577));
#37505=CARTESIAN_POINT('Ctrl Pts',(5.09466658957796,5.,80.8661420261577));
#37506=CARTESIAN_POINT('Ctrl Pts',(5.10409134141797,-5.,80.8587263580475));
#37507=CARTESIAN_POINT('Ctrl Pts',(5.10409134141797,5.,80.8587263580475));
#37508=CARTESIAN_POINT('Ctrl Pts',(5.11011771525274,-5.,80.8542540927006));
#37509=CARTESIAN_POINT('Ctrl Pts',(5.11011771525274,5.,80.8542540927006));
#37510=CARTESIAN_POINT('Ctrl Pts',(5.11306670030725,-5.,80.8521358415414));
#37511=CARTESIAN_POINT('Ctrl Pts',(5.11306670030725,5.,80.8521358415414));
#37512=CARTESIAN_POINT('',(5.11306670030725,0.,80.8521358415414));
#37513=CARTESIAN_POINT('Ctrl Pts',(4.58850001701745,4.8,81.7023557244943));
#37514=CARTESIAN_POINT('Ctrl Pts',(4.58850001701745,3.13333333333333,81.7023557244943));
#37515=CARTESIAN_POINT('Ctrl Pts',(4.58850001701745,1.46666666666667,81.7023557244943));
#37516=CARTESIAN_POINT('Ctrl Pts',(4.58850001701745,-1.73333333333333,81.7023557244943));
#37517=CARTESIAN_POINT('Ctrl Pts',(4.58850001701746,-3.26666666666667,81.7023557244943));
#37518=CARTESIAN_POINT('Ctrl Pts',(4.58850001701746,-4.8,81.7023557244943));
#37519=CARTESIAN_POINT('Origin',(9.30999999999911,0.,78.0000000000005));
#37520=CARTESIAN_POINT('',(5.09956505173093,0.,79.9735089425676));
#37521=CARTESIAN_POINT('',(5.49567364700612,0.,80.659589154899));
#37522=CARTESIAN_POINT('Origin',(5.11306670030725,0.,80.8521358415414));
#37523=CARTESIAN_POINT('Ctrl Pts',(4.7415112563347,-5.,80.2085829347521));
#37524=CARTESIAN_POINT('Ctrl Pts',(4.7415112563347,5.,80.2085829347521));
#37525=CARTESIAN_POINT('Ctrl Pts',(4.73820230448305,-5.,80.2100777051253));
#37526=CARTESIAN_POINT('Ctrl Pts',(4.73820230448305,5.,80.2100777051253));
#37527=CARTESIAN_POINT('Ctrl Pts',(4.73131602214839,-5.,80.2130605652534));
#37528=CARTESIAN_POINT('Ctrl Pts',(4.73131602214839,5.,80.2130605652534));
#37529=CARTESIAN_POINT('Ctrl Pts',(4.72018148924741,-5.,80.2175148056905));
#37530=CARTESIAN_POINT('Ctrl Pts',(4.72018148924741,5.,80.2175148056905));
#37531=CARTESIAN_POINT('Ctrl Pts',(4.70372208056832,-5.,80.2234136895571));
#37532=CARTESIAN_POINT('Ctrl Pts',(4.70372208056832,5.,80.2234136895571));
#37533=CARTESIAN_POINT('Ctrl Pts',(4.68047818546464,-5.,80.2307083643155));
#37534=CARTESIAN_POINT('Ctrl Pts',(4.68047818546464,5.,80.2307083643155));
#37535=CARTESIAN_POINT('Ctrl Pts',(4.65464806075414,-5.,80.2378897915926));
#37536=CARTESIAN_POINT('Ctrl Pts',(4.65464806075414,5.,80.2378897915926));
#37537=CARTESIAN_POINT('Ctrl Pts',(4.62642954792474,-5.,80.2448873545015));
#37538=CARTESIAN_POINT('Ctrl Pts',(4.62642954792474,5.,80.2448873545015));
#37539=CARTESIAN_POINT('Ctrl Pts',(4.59614922798182,-5.,80.2515910686015));
#37540=CARTESIAN_POINT('Ctrl Pts',(4.59614922798182,5.,80.2515910686015));
#37541=CARTESIAN_POINT('Ctrl Pts',(4.56418853184677,-5.,80.2578751926538));
#37542=CARTESIAN_POINT('Ctrl Pts',(4.56418853184677,5.,80.2578751926538));
#37543=CARTESIAN_POINT('Ctrl Pts',(4.53092565703995,-5.,80.263617309213));
#37544=CARTESIAN_POINT('Ctrl Pts',(4.53092565703995,5.,80.263617309213));
#37545=CARTESIAN_POINT('Ctrl Pts',(4.49667595482943,-5.,80.2687178148024));
#37546=CARTESIAN_POINT('Ctrl Pts',(4.49667595482943,5.,80.2687178148024));
#37547=CARTESIAN_POINT('Ctrl Pts',(4.46162197741276,-5.,80.2731232227872));
#37548=CARTESIAN_POINT('Ctrl Pts',(4.46162197741276,5.,80.2731232227872));
#37549=CARTESIAN_POINT('Ctrl Pts',(4.42583429226076,-5.,80.2768185424213));
#37550=CARTESIAN_POINT('Ctrl Pts',(4.42583429226076,5.,80.2768185424213));
#37551=CARTESIAN_POINT('Ctrl Pts',(4.38931316854944,-5.,80.2798126906734));
#37552=CARTESIAN_POINT('Ctrl Pts',(4.38931316854944,5.,80.2798126906734));
#37553=CARTESIAN_POINT('Ctrl Pts',(4.35202333876695,-5.,80.2821264209091));
#37554=CARTESIAN_POINT('Ctrl Pts',(4.35202333876695,5.,80.2821264209091));
#37555=CARTESIAN_POINT('Ctrl Pts',(4.31392987972062,-5.,80.28377999157));
#37556=CARTESIAN_POINT('Ctrl Pts',(4.31392987972062,5.,80.28377999157));
#37557=CARTESIAN_POINT('Ctrl Pts',(4.27503791496249,-5.,80.2847797396365));
#37558=CARTESIAN_POINT('Ctrl Pts',(4.27503791496249,5.,80.2847797396365));
#37559=CARTESIAN_POINT('Ctrl Pts',(4.23538623168037,-5.,80.2851199044714));
#37560=CARTESIAN_POINT('Ctrl Pts',(4.23538623168037,5.,80.2851199044714));
#37561=CARTESIAN_POINT('Ctrl Pts',(4.19503408606993,-5.,80.2847868227625));
#37562=CARTESIAN_POINT('Ctrl Pts',(4.19503408606993,5.,80.2847868227625));
#37563=CARTESIAN_POINT('Ctrl Pts',(4.15405039756986,-5.,80.2837624775403));
#37564=CARTESIAN_POINT('Ctrl Pts',(4.15405039756986,5.,80.2837624775403));
#37565=CARTESIAN_POINT('Ctrl Pts',(4.1125030124698,-5.,80.282028145913));
#37566=CARTESIAN_POINT('Ctrl Pts',(4.1125030124698,5.,80.282028145913));
#37567=CARTESIAN_POINT('Ctrl Pts',(4.07044606473299,-5.,80.2795688335823));
#37568=CARTESIAN_POINT('Ctrl Pts',(4.07044606473299,5.,80.2795688335823));
#37569=CARTESIAN_POINT('Ctrl Pts',(4.02791687754441,-5.,80.2763745972855));
#37570=CARTESIAN_POINT('Ctrl Pts',(4.02791687754441,5.,80.2763745972855));
#37571=CARTESIAN_POINT('Ctrl Pts',(3.98494068385443,-5.,80.2724393512809));
#37572=CARTESIAN_POINT('Ctrl Pts',(3.98494068385443,5.,80.2724393512809));
#37573=CARTESIAN_POINT('Ctrl Pts',(3.94153307998497,-5.,80.267760569364));
#37574=CARTESIAN_POINT('Ctrl Pts',(3.94153307998497,5.,80.267760569364));
#37575=CARTESIAN_POINT('Ctrl Pts',(3.89770346260675,-5.,80.2623388184301));
#37576=CARTESIAN_POINT('Ctrl Pts',(3.89770346260675,5.,80.2623388184301));
#37577=CARTESIAN_POINT('Ctrl Pts',(3.85345801322638,-5.,80.2561775269785));
#37578=CARTESIAN_POINT('Ctrl Pts',(3.85345801322638,5.,80.2561775269785));
#37579=CARTESIAN_POINT('Ctrl Pts',(3.80880313234891,-5.,80.249282909649));
#37580=CARTESIAN_POINT('Ctrl Pts',(3.80880313234891,5.,80.249282909649));
#37581=CARTESIAN_POINT('Ctrl Pts',(3.76374506499486,-5.,80.2416626589451));
#37582=CARTESIAN_POINT('Ctrl Pts',(3.76374506499486,5.,80.2416626589451));
#37583=CARTESIAN_POINT('Ctrl Pts',(3.71828934520081,-5.,80.2333246468413));
#37584=CARTESIAN_POINT('Ctrl Pts',(3.71828934520081,5.,80.2333246468413));
#37585=CARTESIAN_POINT('Ctrl Pts',(3.68161017699181,-5.,80.2260855538483));
#37586=CARTESIAN_POINT('Ctrl Pts',(3.68161017699181,5.,80.2260855538483));
#37587=CARTESIAN_POINT('Ctrl Pts',(3.65392514646726,-5.,80.220338548454));
#37588=CARTESIAN_POINT('Ctrl Pts',(3.65392514646726,5.,80.220338548454));
#37589=CARTESIAN_POINT('Ctrl Pts',(3.63539053217137,-5.,80.2163662733738));
#37590=CARTESIAN_POINT('Ctrl Pts',(3.63539053217137,5.,80.2163662733738));
#37591=CARTESIAN_POINT('Ctrl Pts',(3.62610374319018,-5.,80.2143449012797));
#37592=CARTESIAN_POINT('Ctrl Pts',(3.62610374319018,5.,80.2143449012797));
#37593=CARTESIAN_POINT('Ctrl Pts',(3.74291589718233,-4.8,80.2377610668154));
#37594=CARTESIAN_POINT('Ctrl Pts',(3.74291589718233,-3.13333333333333,80.2377610668154));
#37595=CARTESIAN_POINT('Ctrl Pts',(3.74291589718233,-1.46666666666667,80.2377610668154));
#37596=CARTESIAN_POINT('Ctrl Pts',(3.74291589718233,1.73333333333333,80.2377610668154));
#37597=CARTESIAN_POINT('Ctrl Pts',(3.74291589718234,3.26666666666667,80.2377610668154));
#37598=CARTESIAN_POINT('Ctrl Pts',(3.74291589718234,4.8,80.2377610668154));
#37599=CARTESIAN_POINT('',(4.7415112563347,0.,80.2085829347521));
#37600=CARTESIAN_POINT('Origin',(5.09956505173093,0.,79.9735089425676));
#37601=CARTESIAN_POINT('Ctrl Pts',(8.11629420041964,-5.,83.9820620578567));
#37602=CARTESIAN_POINT('Ctrl Pts',(8.11629420041964,5.,83.9820620578567));
#37603=CARTESIAN_POINT('Ctrl Pts',(8.11269090350116,-5.,83.9732673636178));
#37604=CARTESIAN_POINT('Ctrl Pts',(8.11269090350116,5.,83.9732673636178));
#37605=CARTESIAN_POINT('Ctrl Pts',(8.10556047416415,-5.,83.9557041100362));
#37606=CARTESIAN_POINT('Ctrl Pts',(8.10556047416415,5.,83.9557041100362));
#37607=CARTESIAN_POINT('Ctrl Pts',(8.09509332354789,-5.,83.9294376342902));
#37608=CARTESIAN_POINT('Ctrl Pts',(8.09509332354789,5.,83.9294376342902));
#37609=CARTESIAN_POINT('Ctrl Pts',(8.0815949378981,-5.,83.8945727603373));
#37610=CARTESIAN_POINT('Ctrl Pts',(8.0815949378981,5.,83.8945727603373));
#37611=CARTESIAN_POINT('Ctrl Pts',(8.06549029603877,-5.,83.8512554956866));
#37612=CARTESIAN_POINT('Ctrl Pts',(8.06549029603877,5.,83.8512554956866));
#37613=CARTESIAN_POINT('Ctrl Pts',(8.05016156282195,-5.,83.8082052043177));
#37614=CARTESIAN_POINT('Ctrl Pts',(8.05016156282195,5.,83.8082052043177));
#37615=CARTESIAN_POINT('Ctrl Pts',(8.03561745158609,-5.,83.7654259692167));
#37616=CARTESIAN_POINT('Ctrl Pts',(8.03561745158609,5.,83.7654259692167));
#37617=CARTESIAN_POINT('Ctrl Pts',(8.0218666223879,-5.,83.7229226047198));
#37618=CARTESIAN_POINT('Ctrl Pts',(8.0218666223879,5.,83.7229226047198));
#37619=CARTESIAN_POINT('Ctrl Pts',(8.00891630687788,-5.,83.6807003349195));
#37620=CARTESIAN_POINT('Ctrl Pts',(8.00891630687788,5.,83.6807003349195));
#37621=CARTESIAN_POINT('Ctrl Pts',(7.9967709548731,-5.,83.6387646520556));
#37622=CARTESIAN_POINT('Ctrl Pts',(7.9967709548731,5.,83.6387646520556));
#37623=CARTESIAN_POINT('Ctrl Pts',(7.98543275637429,-5.,83.597124711605));
#37624=CARTESIAN_POINT('Ctrl Pts',(7.98543275637429,5.,83.597124711605));
#37625=CARTESIAN_POINT('Ctrl Pts',(7.97490193183486,-5.,83.555796311625));
#37626=CARTESIAN_POINT('Ctrl Pts',(7.97490193183486,5.,83.555796311625));
#37627=CARTESIAN_POINT('Ctrl Pts',(7.96517686963337,-5.,83.5148053585083));
#37628=CARTESIAN_POINT('Ctrl Pts',(7.96517686963337,5.,83.5148053585083));
#37629=CARTESIAN_POINT('Ctrl Pts',(7.95625425867753,-5.,83.4741903350539));
#37630=CARTESIAN_POINT('Ctrl Pts',(7.95625425867753,5.,83.4741903350539));
#37631=CARTESIAN_POINT('Ctrl Pts',(7.94812873273393,-5.,83.4340071565454));
#37632=CARTESIAN_POINT('Ctrl Pts',(7.94812873273393,5.,83.4340071565454));
#37633=CARTESIAN_POINT('Ctrl Pts',(7.94079363473637,-5.,83.3943258897297));
#37634=CARTESIAN_POINT('Ctrl Pts',(7.94079363473637,5.,83.3943258897297));
#37635=CARTESIAN_POINT('Ctrl Pts',(7.93424318916526,-5.,83.3552175356154));
#37636=CARTESIAN_POINT('Ctrl Pts',(7.93424318916526,5.,83.3552175356154));
#37637=CARTESIAN_POINT('Ctrl Pts',(7.9284742300107,-5.,83.3167428227687));
#37638=CARTESIAN_POINT('Ctrl Pts',(7.9284742300107,5.,83.3167428227687));
#37639=CARTESIAN_POINT('Ctrl Pts',(7.92348781947404,-5.,83.2789409494337));
#37640=CARTESIAN_POINT('Ctrl Pts',(7.92348781947404,5.,83.2789409494337));
#37641=CARTESIAN_POINT('Ctrl Pts',(7.91929108795717,-5.,83.2418158609173));
#37642=CARTESIAN_POINT('Ctrl Pts',(7.91929108795717,5.,83.2418158609173));
#37643=CARTESIAN_POINT('Ctrl Pts',(7.91589792178468,-5.,83.2053296467483));
#37644=CARTESIAN_POINT('Ctrl Pts',(7.91589792178468,5.,83.2053296467483));
#37645=CARTESIAN_POINT('Ctrl Pts',(7.9133226348972,-5.,83.1694439714255));
#37646=CARTESIAN_POINT('Ctrl Pts',(7.9133226348972,5.,83.1694439714255));
#37647=CARTESIAN_POINT('Ctrl Pts',(7.91157405554035,-5.,83.1341575516226));
#37648=CARTESIAN_POINT('Ctrl Pts',(7.91157405554035,5.,83.1341575516226));
#37649=CARTESIAN_POINT('Ctrl Pts',(7.91064967462546,-5.,83.0995424858489));
#37650=CARTESIAN_POINT('Ctrl Pts',(7.91064967462546,5.,83.0995424858489));
#37651=CARTESIAN_POINT('Ctrl Pts',(7.91052851795315,-5.,83.0657878407806));
#37652=CARTESIAN_POINT('Ctrl Pts',(7.91052851795315,5.,83.0657878407806));
#37653=CARTESIAN_POINT('Ctrl Pts',(7.91116725541189,-5.,83.0332214727501));
#37654=CARTESIAN_POINT('Ctrl Pts',(7.91116725541189,5.,83.0332214727501));
#37655=CARTESIAN_POINT('Ctrl Pts',(7.91251100265399,-5.,83.00223709117));
#37656=CARTESIAN_POINT('Ctrl Pts',(7.91251100265399,5.,83.00223709117));
#37657=CARTESIAN_POINT('Ctrl Pts',(7.91450216351211,-5.,82.9732321669035));
#37658=CARTESIAN_POINT('Ctrl Pts',(7.91450216351211,5.,82.9732321669035));
#37659=CARTESIAN_POINT('Ctrl Pts',(7.91708913465533,-5.,82.9465474180553));
#37660=CARTESIAN_POINT('Ctrl Pts',(7.91708913465533,5.,82.9465474180553));
#37661=CARTESIAN_POINT('Ctrl Pts',(7.92023672685611,-5.,82.9223899429567));
#37662=CARTESIAN_POINT('Ctrl Pts',(7.92023672685611,5.,82.9223899429567));
#37663=CARTESIAN_POINT('Ctrl Pts',(7.92318784709605,-5.,82.9051562592444));
#37664=CARTESIAN_POINT('Ctrl Pts',(7.92318784709605,5.,82.9051562592444));
#37665=CARTESIAN_POINT('Ctrl Pts',(7.92564092628298,-5.,82.8934174141896));
#37666=CARTESIAN_POINT('Ctrl Pts',(7.92564092628298,5.,82.8934174141896));
#37667=CARTESIAN_POINT('Ctrl Pts',(7.92738267970764,-5.,82.8861177817404));
#37668=CARTESIAN_POINT('Ctrl Pts',(7.92738267970764,5.,82.8861177817404));
#37669=CARTESIAN_POINT('Ctrl Pts',(7.92828014771505,-5.,82.8825995361566));
#37670=CARTESIAN_POINT('Ctrl Pts',(7.92828014771505,5.,82.8825995361566));
#37671=CARTESIAN_POINT('',(7.92828014771505,0.,82.8825995361566));
#37672=CARTESIAN_POINT('Ctrl Pts',(8.07294956130202,4.8,83.871090717415));
#37673=CARTESIAN_POINT('Ctrl Pts',(8.07294956130202,3.13333333333333,83.871090717415));
#37674=CARTESIAN_POINT('Ctrl Pts',(8.07294956130202,1.46666666666667,83.871090717415));
#37675=CARTESIAN_POINT('Ctrl Pts',(8.07294956130202,-1.73333333333333,83.871090717415));
#37676=CARTESIAN_POINT('Ctrl Pts',(8.07294956130202,-3.26666666666667,83.871090717415));
#37677=CARTESIAN_POINT('Ctrl Pts',(8.07294956130202,-4.8,83.871090717415));
#37678=CARTESIAN_POINT('Origin',(9.31000000000056,0.,77.9999999999986));
#37679=CARTESIAN_POINT('',(7.3531668006526,0.,82.2182109750381));
#37680=CARTESIAN_POINT('',(8.09760744867255,0.,82.4891652120952));
#37681=CARTESIAN_POINT('Origin',(7.92828014771505,0.,82.8825995361566));
#37682=CARTESIAN_POINT('Ctrl Pts',(7.22998432988738,-5.,82.6284406437547));
#37683=CARTESIAN_POINT('Ctrl Pts',(7.22998432988738,5.,82.6284406437547));
#37684=CARTESIAN_POINT('Ctrl Pts',(7.22841034559216,-5.,82.6317126575429));
#37685=CARTESIAN_POINT('Ctrl Pts',(7.22841034559216,5.,82.6317126575429));
#37686=CARTESIAN_POINT('Ctrl Pts',(7.22505249282082,-5.,82.6384240779281));
#37687=CARTESIAN_POINT('Ctrl Pts',(7.22505249282082,5.,82.6384240779281));
#37688=CARTESIAN_POINT('Ctrl Pts',(7.21938607633931,-5.,82.64899336385));
#37689=CARTESIAN_POINT('Ctrl Pts',(7.21938607633931,5.,82.64899336385));
#37690=CARTESIAN_POINT('Ctrl Pts',(7.21056916724215,-5.,82.6640920750187));
#37691=CARTESIAN_POINT('Ctrl Pts',(7.21056916724215,5.,82.6640920750187));
#37692=CARTESIAN_POINT('Ctrl Pts',(7.19745223709537,-5.,82.6846210078579));
#37693=CARTESIAN_POINT('Ctrl Pts',(7.19745223709537,5.,82.6846210078579));
#37694=CARTESIAN_POINT('Ctrl Pts',(7.18228134605083,-5.,82.7067255844406));
#37695=CARTESIAN_POINT('Ctrl Pts',(7.18228134605083,5.,82.7067255844406));
#37696=CARTESIAN_POINT('Ctrl Pts',(7.16516265783049,-5.,82.7302245390343));
#37697=CARTESIAN_POINT('Ctrl Pts',(7.16516265783049,5.,82.7302245390343));
#37698=CARTESIAN_POINT('Ctrl Pts',(7.14627565136447,-5.,82.754823696445));
#37699=CARTESIAN_POINT('Ctrl Pts',(7.14627565136447,5.,82.754823696445));
#37700=CARTESIAN_POINT('Ctrl Pts',(7.12583169477743,-5.,82.7801815542262));
#37701=CARTESIAN_POINT('Ctrl Pts',(7.12583169477743,5.,82.7801815542262));
#37702=CARTESIAN_POINT('Ctrl Pts',(7.1040418157563,-5.,82.8059612344958));
#37703=CARTESIAN_POINT('Ctrl Pts',(7.1040418157563,5.,82.8059612344958));
#37704=CARTESIAN_POINT('Ctrl Pts',(7.08108356350195,-5.,82.8318837326766));
#37705=CARTESIAN_POINT('Ctrl Pts',(7.08108356350195,5.,82.8318837326766));
#37706=CARTESIAN_POINT('Ctrl Pts',(7.05706240056282,-5.,82.8577907333377));
#37707=CARTESIAN_POINT('Ctrl Pts',(7.05706240056282,5.,82.8577907333377));
#37708=CARTESIAN_POINT('Ctrl Pts',(7.03202274889278,-5.,82.883625393005));
#37709=CARTESIAN_POINT('Ctrl Pts',(7.03202274889278,5.,82.883625393005));
#37710=CARTESIAN_POINT('Ctrl Pts',(7.00597054641171,-5.,82.9093943694487));
#37711=CARTESIAN_POINT('Ctrl Pts',(7.00597054641171,5.,82.9093943694487));
#37712=CARTESIAN_POINT('Ctrl Pts',(6.97889211664698,-5.,82.9351362301886));
#37713=CARTESIAN_POINT('Ctrl Pts',(6.97889211664698,5.,82.9351362301886));
#37714=CARTESIAN_POINT('Ctrl Pts',(6.95077372875796,-5.,82.9608889422872));
#37715=CARTESIAN_POINT('Ctrl Pts',(6.95077372875796,5.,82.9608889422872));
#37716=CARTESIAN_POINT('Ctrl Pts',(6.92162338094528,-5.,82.9866540667982));
#37717=CARTESIAN_POINT('Ctrl Pts',(6.92162338094528,5.,82.9866540667982));
#37718=CARTESIAN_POINT('Ctrl Pts',(6.89146708305081,-5.,83.012402258895));
#37719=CARTESIAN_POINT('Ctrl Pts',(6.89146708305081,5.,83.012402258895));
#37720=CARTESIAN_POINT('Ctrl Pts',(6.86034144534373,-5.,83.0380849627259));
#37721=CARTESIAN_POINT('Ctrl Pts',(6.86034144534373,5.,83.0380849627259));
#37722=CARTESIAN_POINT('Ctrl Pts',(6.82828768209046,-5.,83.0636440759307));
#37723=CARTESIAN_POINT('Ctrl Pts',(6.82828768209046,5.,83.0636440759307));
#37724=CARTESIAN_POINT('Ctrl Pts',(6.7953457317203,-5.,83.0890216451884));
#37725=CARTESIAN_POINT('Ctrl Pts',(6.7953457317203,5.,83.0890216451884));
#37726=CARTESIAN_POINT('Ctrl Pts',(6.76154742510777,-5.,83.1141713875575));
#37727=CARTESIAN_POINT('Ctrl Pts',(6.76154742510777,5.,83.1141713875575));
#37728=CARTESIAN_POINT('Ctrl Pts',(6.72691496206891,-5.,83.1390616951735));
#37729=CARTESIAN_POINT('Ctrl Pts',(6.72691496206891,5.,83.1390616951735));
#37730=CARTESIAN_POINT('Ctrl Pts',(6.6914637603302,-5.,83.1636716866569));
#37731=CARTESIAN_POINT('Ctrl Pts',(6.6914637603302,5.,83.1636716866569));
#37732=CARTESIAN_POINT('Ctrl Pts',(6.65520414355774,-5.,83.1879894016978));
#37733=CARTESIAN_POINT('Ctrl Pts',(6.65520414355774,5.,83.1879894016978));
#37734=CARTESIAN_POINT('Ctrl Pts',(6.61814367441389,-5.,83.2120092344991));
#37735=CARTESIAN_POINT('Ctrl Pts',(6.61814367441389,5.,83.2120092344991));
#37736=CARTESIAN_POINT('Ctrl Pts',(6.58028929200272,-5.,83.2357298380487));
#37737=CARTESIAN_POINT('Ctrl Pts',(6.58028929200272,5.,83.2357298380487));
#37738=CARTESIAN_POINT('Ctrl Pts',(6.54164989408328,-5.,83.259151858876));
#37739=CARTESIAN_POINT('Ctrl Pts',(6.54164989408328,5.,83.259151858876));
#37740=CARTESIAN_POINT('Ctrl Pts',(6.50223520925582,-5.,83.282277175565));
#37741=CARTESIAN_POINT('Ctrl Pts',(6.50223520925582,5.,83.282277175565));
#37742=CARTESIAN_POINT('Ctrl Pts',(6.46205453683623,-5.,83.3051082611947));
#37743=CARTESIAN_POINT('Ctrl Pts',(6.46205453683623,5.,83.3051082611947));
#37744=CARTESIAN_POINT('Ctrl Pts',(6.42930346455563,-5.,83.3231397091032));
#37745=CARTESIAN_POINT('Ctrl Pts',(6.42930346455563,5.,83.3231397091032));
#37746=CARTESIAN_POINT('Ctrl Pts',(6.40440139687902,-5.,83.3365328421698));
#37747=CARTESIAN_POINT('Ctrl Pts',(6.40440139687902,5.,83.3365328421698));
#37748=CARTESIAN_POINT('Ctrl Pts',(6.38764972936484,-5.,83.3454037233548));
#37749=CARTESIAN_POINT('Ctrl Pts',(6.38764972936484,5.,83.3454037233548));
#37750=CARTESIAN_POINT('Ctrl Pts',(6.37923632332122,-5.,83.3498246953952));
#37751=CARTESIAN_POINT('Ctrl Pts',(6.37923632332122,5.,83.3498246953952));
#37752=CARTESIAN_POINT('Ctrl Pts',(6.48377124583838,-4.8,83.2926771136307));
#37753=CARTESIAN_POINT('Ctrl Pts',(6.48377124583838,-3.13333333333333,83.2926771136307));
#37754=CARTESIAN_POINT('Ctrl Pts',(6.48377124583838,-1.46666666666667,83.2926771136307));
#37755=CARTESIAN_POINT('Ctrl Pts',(6.48377124583838,1.73333333333333,83.2926771136307));
#37756=CARTESIAN_POINT('Ctrl Pts',(6.48377124583837,3.26666666666667,83.2926771136307));
#37757=CARTESIAN_POINT('Ctrl Pts',(6.48377124583837,4.8,83.2926771136307));
#37758=CARTESIAN_POINT('',(7.22998432988738,0.,82.6284406437547));
#37759=CARTESIAN_POINT('Origin',(7.3531668006526,0.,82.2182109750381));
#37760=CARTESIAN_POINT('Ctrl Pts',(12.2407636766788,-5.,83.3498246953952));
#37761=CARTESIAN_POINT('Ctrl Pts',(12.2407636766788,5.,83.3498246953952));
#37762=CARTESIAN_POINT('Ctrl Pts',(12.2323502706297,-5.,83.3454037233561));
#37763=CARTESIAN_POINT('Ctrl Pts',(12.2323502706297,5.,83.3454037233561));
#37764=CARTESIAN_POINT('Ctrl Pts',(12.2155986031059,-5.,83.3365328421734));
#37765=CARTESIAN_POINT('Ctrl Pts',(12.2155986031059,5.,83.3365328421734));
#37766=CARTESIAN_POINT('Ctrl Pts',(12.190696535419,-5.,83.3231397091095));
#37767=CARTESIAN_POINT('Ctrl Pts',(12.190696535419,5.,83.3231397091095));
#37768=CARTESIAN_POINT('Ctrl Pts',(12.1579454631325,-5.,83.3051082612026));
#37769=CARTESIAN_POINT('Ctrl Pts',(12.1579454631325,5.,83.3051082612026));
#37770=CARTESIAN_POINT('Ctrl Pts',(12.1177647907155,-5.,83.2822771755727));
#37771=CARTESIAN_POINT('Ctrl Pts',(12.1177647907155,5.,83.2822771755727));
#37772=CARTESIAN_POINT('Ctrl Pts',(12.0783501058969,-5.,83.2591518588818));
#37773=CARTESIAN_POINT('Ctrl Pts',(12.0783501058969,5.,83.2591518588818));
#37774=CARTESIAN_POINT('Ctrl Pts',(12.0397107079887,-5.,83.2357298380515));
#37775=CARTESIAN_POINT('Ctrl Pts',(12.0397107079887,5.,83.2357298380515));
#37776=CARTESIAN_POINT('Ctrl Pts',(12.0018563255876,-5.,83.2120092344988));
#37777=CARTESIAN_POINT('Ctrl Pts',(12.0018563255876,5.,83.2120092344988));
#37778=CARTESIAN_POINT('Ctrl Pts',(11.9647958564502,-5.,83.1879894016949));
#37779=CARTESIAN_POINT('Ctrl Pts',(11.9647958564502,5.,83.1879894016949));
#37780=CARTESIAN_POINT('Ctrl Pts',(11.92853623968,-5.,83.1636716866526));
#37781=CARTESIAN_POINT('Ctrl Pts',(11.92853623968,5.,83.1636716866526));
#37782=CARTESIAN_POINT('Ctrl Pts',(11.89308503794,-5.,83.1390616951692));
#37783=CARTESIAN_POINT('Ctrl Pts',(11.89308503794,5.,83.1390616951692));
#37784=CARTESIAN_POINT('Ctrl Pts',(11.8584525748976,-5.,83.1141713875545));
#37785=CARTESIAN_POINT('Ctrl Pts',(11.8584525748976,5.,83.1141713875545));
#37786=CARTESIAN_POINT('Ctrl Pts',(11.8246542682811,-5.,83.0890216451873));
#37787=CARTESIAN_POINT('Ctrl Pts',(11.8246542682811,5.,83.0890216451873));
#37788=CARTESIAN_POINT('Ctrl Pts',(11.791712317908,-5.,83.0636440759316));
#37789=CARTESIAN_POINT('Ctrl Pts',(11.791712317908,5.,83.0636440759316));
#37790=CARTESIAN_POINT('Ctrl Pts',(11.7596585546537,-5.,83.0380849627281));
#37791=CARTESIAN_POINT('Ctrl Pts',(11.7596585546537,5.,83.0380849627281));
#37792=CARTESIAN_POINT('Ctrl Pts',(11.7285329169469,-5.,83.012402258898));
#37793=CARTESIAN_POINT('Ctrl Pts',(11.7285329169469,5.,83.012402258898));
#37794=CARTESIAN_POINT('Ctrl Pts',(11.6983766190536,-5.,82.9866540668011));
#37795=CARTESIAN_POINT('Ctrl Pts',(11.6983766190536,5.,82.9866540668011));
#37796=CARTESIAN_POINT('Ctrl Pts',(11.669226271242,-5.,82.960888942289));
#37797=CARTESIAN_POINT('Ctrl Pts',(11.669226271242,5.,82.960888942289));
#37798=CARTESIAN_POINT('Ctrl Pts',(11.6411078833532,-5.,82.9351362301884));
#37799=CARTESIAN_POINT('Ctrl Pts',(11.6411078833532,5.,82.9351362301884));
#37800=CARTESIAN_POINT('Ctrl Pts',(11.6140294535877,-5.,82.9093943694462));
#37801=CARTESIAN_POINT('Ctrl Pts',(11.6140294535877,5.,82.9093943694462));
#37802=CARTESIAN_POINT('Ctrl Pts',(11.5879772511054,-5.,82.883625393001));
#37803=CARTESIAN_POINT('Ctrl Pts',(11.5879772511054,5.,82.883625393001));
#37804=CARTESIAN_POINT('Ctrl Pts',(11.5629375994346,-5.,82.8577907333339));
#37805=CARTESIAN_POINT('Ctrl Pts',(11.5629375994346,5.,82.8577907333339));
#37806=CARTESIAN_POINT('Ctrl Pts',(11.5389164364961,-5.,82.8318837326744));
#37807=CARTESIAN_POINT('Ctrl Pts',(11.5389164364961,5.,82.8318837326744));
#37808=CARTESIAN_POINT('Ctrl Pts',(11.515958184244,-5.,82.8059612344964));
#37809=CARTESIAN_POINT('Ctrl Pts',(11.515958184244,5.,82.8059612344964));
#37810=CARTESIAN_POINT('Ctrl Pts',(11.4941683052261,-5.,82.7801815542291));
#37811=CARTESIAN_POINT('Ctrl Pts',(11.4941683052261,5.,82.7801815542291));
#37812=CARTESIAN_POINT('Ctrl Pts',(11.4737243486416,-5.,82.7548236964487));
#37813=CARTESIAN_POINT('Ctrl Pts',(11.4737243486416,5.,82.7548236964487));
#37814=CARTESIAN_POINT('Ctrl Pts',(11.4548373421755,-5.,82.730224539037));
#37815=CARTESIAN_POINT('Ctrl Pts',(11.4548373421755,5.,82.730224539037));
#37816=CARTESIAN_POINT('Ctrl Pts',(11.4377186539515,-5.,82.7067255844413));
#37817=CARTESIAN_POINT('Ctrl Pts',(11.4377186539515,5.,82.7067255844413));
#37818=CARTESIAN_POINT('Ctrl Pts',(11.4225477629002,-5.,82.6846210078564));
#37819=CARTESIAN_POINT('Ctrl Pts',(11.4225477629002,5.,82.6846210078564));
#37820=CARTESIAN_POINT('Ctrl Pts',(11.4094308327472,-5.,82.6640920750159));
#37821=CARTESIAN_POINT('Ctrl Pts',(11.4094308327472,5.,82.6640920750159));
#37822=CARTESIAN_POINT('Ctrl Pts',(11.4006139236494,-5.,82.6489933638476));
#37823=CARTESIAN_POINT('Ctrl Pts',(11.4006139236494,5.,82.6489933638476));
#37824=CARTESIAN_POINT('Ctrl Pts',(11.3949475071716,-5.,82.6384240779267));
#37825=CARTESIAN_POINT('Ctrl Pts',(11.3949475071716,5.,82.6384240779267));
#37826=CARTESIAN_POINT('Ctrl Pts',(11.391589654405,-5.,82.6317126575424));
#37827=CARTESIAN_POINT('Ctrl Pts',(11.391589654405,5.,82.6317126575424));
#37828=CARTESIAN_POINT('Ctrl Pts',(11.3900156701126,-5.,82.6284406437547));
#37829=CARTESIAN_POINT('Ctrl Pts',(11.3900156701126,5.,82.6284406437547));
#37830=CARTESIAN_POINT('',(11.3900156701126,0.,82.6284406437547));
#37831=CARTESIAN_POINT('Ctrl Pts',(12.1362287541399,4.8,83.2926771136423));
#37832=CARTESIAN_POINT('Ctrl Pts',(12.1362287541399,3.13333333333333,83.2926771136423));
#37833=CARTESIAN_POINT('Ctrl Pts',(12.1362287541399,1.46666666666667,83.2926771136423));
#37834=CARTESIAN_POINT('Ctrl Pts',(12.1362287541399,-1.73333333333333,83.2926771136423));
#37835=CARTESIAN_POINT('Ctrl Pts',(12.1362287541399,-3.26666666666667,83.2926771136423));
#37836=CARTESIAN_POINT('Ctrl Pts',(12.1362287541399,-4.8,83.2926771136423));
#37837=CARTESIAN_POINT('Origin',(9.31000000000013,0.,78.0000000000003));
#37838=CARTESIAN_POINT('',(10.5223925513275,0.,82.4891652120952));
#37839=CARTESIAN_POINT('',(11.2668331993474,0.,82.2182109750381));
#37840=CARTESIAN_POINT('Origin',(11.3900156701126,0.,82.6284406437547));
#37841=CARTESIAN_POINT('Ctrl Pts',(10.691719852285,-5.,82.8825995361566));
#37842=CARTESIAN_POINT('Ctrl Pts',(10.691719852285,5.,82.8825995361566));
#37843=CARTESIAN_POINT('Ctrl Pts',(10.6926173202914,-5.,82.8861177817402));
#37844=CARTESIAN_POINT('Ctrl Pts',(10.6926173202914,5.,82.8861177817402));
#37845=CARTESIAN_POINT('Ctrl Pts',(10.6943590737144,-5.,82.8934174141892));
#37846=CARTESIAN_POINT('Ctrl Pts',(10.6943590737144,5.,82.8934174141892));
#37847=CARTESIAN_POINT('Ctrl Pts',(10.6968121528999,-5.,82.9051562592437));
#37848=CARTESIAN_POINT('Ctrl Pts',(10.6968121528999,5.,82.9051562592437));
#37849=CARTESIAN_POINT('Ctrl Pts',(10.69976327314,-5.,82.9223899429559));
#37850=CARTESIAN_POINT('Ctrl Pts',(10.69976327314,5.,82.9223899429559));
#37851=CARTESIAN_POINT('Ctrl Pts',(10.7029108653431,-5.,82.9465474180549));
#37852=CARTESIAN_POINT('Ctrl Pts',(10.7029108653431,5.,82.9465474180549));
#37853=CARTESIAN_POINT('Ctrl Pts',(10.7054978364887,-5.,82.9732321669037));
#37854=CARTESIAN_POINT('Ctrl Pts',(10.7054978364887,5.,82.9732321669037));
#37855=CARTESIAN_POINT('Ctrl Pts',(10.7074889973481,-5.,83.0022370911707));
#37856=CARTESIAN_POINT('Ctrl Pts',(10.7074889973481,5.,83.0022370911707));
#37857=CARTESIAN_POINT('Ctrl Pts',(10.7088327445902,-5.,83.0332214727508));
#37858=CARTESIAN_POINT('Ctrl Pts',(10.7088327445902,5.,83.0332214727508));
#37859=CARTESIAN_POINT('Ctrl Pts',(10.7094714820479,-5.,83.0657878407809));
#37860=CARTESIAN_POINT('Ctrl Pts',(10.7094714820479,5.,83.0657878407809));
#37861=CARTESIAN_POINT('Ctrl Pts',(10.7093503253746,-5.,83.0995424858489));
#37862=CARTESIAN_POINT('Ctrl Pts',(10.7093503253746,5.,83.0995424858489));
#37863=CARTESIAN_POINT('Ctrl Pts',(10.7084259444592,-5.,83.1341575516224));
#37864=CARTESIAN_POINT('Ctrl Pts',(10.7084259444592,5.,83.1341575516224));
#37865=CARTESIAN_POINT('Ctrl Pts',(10.7066773651025,-5.,83.1694439714256));
#37866=CARTESIAN_POINT('Ctrl Pts',(10.7066773651025,5.,83.1694439714256));
#37867=CARTESIAN_POINT('Ctrl Pts',(10.7041020782155,-5.,83.2053296467487));
#37868=CARTESIAN_POINT('Ctrl Pts',(10.7041020782155,5.,83.2053296467487));
#37869=CARTESIAN_POINT('Ctrl Pts',(10.7007089120433,-5.,83.2418158609177));
#37870=CARTESIAN_POINT('Ctrl Pts',(10.7007089120433,5.,83.2418158609177));
#37871=CARTESIAN_POINT('Ctrl Pts',(10.6965121805262,-5.,83.2789409494337));
#37872=CARTESIAN_POINT('Ctrl Pts',(10.6965121805262,5.,83.2789409494337));
#37873=CARTESIAN_POINT('Ctrl Pts',(10.6915257699886,-5.,83.3167428227683));
#37874=CARTESIAN_POINT('Ctrl Pts',(10.6915257699886,5.,83.3167428227683));
#37875=CARTESIAN_POINT('Ctrl Pts',(10.6857568108328,-5.,83.355217535615));
#37876=CARTESIAN_POINT('Ctrl Pts',(10.6857568108328,5.,83.355217535615));
#37877=CARTESIAN_POINT('Ctrl Pts',(10.6792063652607,-5.,83.3943258897293));
#37878=CARTESIAN_POINT('Ctrl Pts',(10.6792063652607,5.,83.3943258897293));
#37879=CARTESIAN_POINT('Ctrl Pts',(10.6718712672631,-5.,83.4340071565451));
#37880=CARTESIAN_POINT('Ctrl Pts',(10.6718712672631,5.,83.4340071565451));
#37881=CARTESIAN_POINT('Ctrl Pts',(10.6637457413209,-5.,83.4741903350538));
#37882=CARTESIAN_POINT('Ctrl Pts',(10.6637457413209,5.,83.4741903350538));
#37883=CARTESIAN_POINT('Ctrl Pts',(10.6548231303682,-5.,83.5148053585084));
#37884=CARTESIAN_POINT('Ctrl Pts',(10.6548231303682,5.,83.5148053585084));
#37885=CARTESIAN_POINT('Ctrl Pts',(10.6450980681707,-5.,83.555796311625));
#37886=CARTESIAN_POINT('Ctrl Pts',(10.6450980681707,5.,83.555796311625));
#37887=CARTESIAN_POINT('Ctrl Pts',(10.6345672436347,-5.,83.5971247116047));
#37888=CARTESIAN_POINT('Ctrl Pts',(10.6345672436347,5.,83.5971247116047));
#37889=CARTESIAN_POINT('Ctrl Pts',(10.6232290451371,-5.,83.638764652055));
#37890=CARTESIAN_POINT('Ctrl Pts',(10.6232290451371,5.,83.638764652055));
#37891=CARTESIAN_POINT('Ctrl Pts',(10.61108369313,-5.,83.680700334919));
#37892=CARTESIAN_POINT('Ctrl Pts',(10.61108369313,5.,83.680700334919));
#37893=CARTESIAN_POINT('Ctrl Pts',(10.5981333776136,-5.,83.7229226047197));
#37894=CARTESIAN_POINT('Ctrl Pts',(10.5981333776136,5.,83.7229226047197));
#37895=CARTESIAN_POINT('Ctrl Pts',(10.5843825484055,-5.,83.7654259692172));
#37896=CARTESIAN_POINT('Ctrl Pts',(10.5843825484055,5.,83.7654259692172));
#37897=CARTESIAN_POINT('Ctrl Pts',(10.5698384371585,-5.,83.8082052043188));
#37898=CARTESIAN_POINT('Ctrl Pts',(10.5698384371585,5.,83.8082052043188));
#37899=CARTESIAN_POINT('Ctrl Pts',(10.5545097039329,-5.,83.8512554956884));
#37900=CARTESIAN_POINT('Ctrl Pts',(10.5545097039329,5.,83.8512554956884));
#37901=CARTESIAN_POINT('Ctrl Pts',(10.5384050620711,-5.,83.8945727603393));
#37902=CARTESIAN_POINT('Ctrl Pts',(10.5384050620711,5.,83.8945727603393));
#37903=CARTESIAN_POINT('Ctrl Pts',(10.5249066764272,-5.,83.9294376342919));
#37904=CARTESIAN_POINT('Ctrl Pts',(10.5249066764272,5.,83.9294376342919));
#37905=CARTESIAN_POINT('Ctrl Pts',(10.5144395258211,-5.,83.9557041100372));
#37906=CARTESIAN_POINT('Ctrl Pts',(10.5144395258211,5.,83.9557041100372));
#37907=CARTESIAN_POINT('Ctrl Pts',(10.5073090964935,-5.,83.9732673636182));
#37908=CARTESIAN_POINT('Ctrl Pts',(10.5073090964935,5.,83.9732673636182));
#37909=CARTESIAN_POINT('Ctrl Pts',(10.5037057995804,-5.,83.9820620578567));
#37910=CARTESIAN_POINT('Ctrl Pts',(10.5037057995804,5.,83.9820620578567));
#37911=CARTESIAN_POINT('Ctrl Pts',(10.5470504386678,-4.8,83.8710907174214));
#37912=CARTESIAN_POINT('Ctrl Pts',(10.5470504386678,-3.13333333333333,83.8710907174214));
#37913=CARTESIAN_POINT('Ctrl Pts',(10.5470504386678,-1.46666666666667,83.8710907174214));
#37914=CARTESIAN_POINT('Ctrl Pts',(10.5470504386678,1.73333333333333,83.8710907174214));
#37915=CARTESIAN_POINT('Ctrl Pts',(10.5470504386678,3.26666666666667,83.8710907174214));
#37916=CARTESIAN_POINT('Ctrl Pts',(10.5470504386678,4.8,83.8710907174214));
#37917=CARTESIAN_POINT('',(10.691719852285,0.,82.8825995361566));
#37918=CARTESIAN_POINT('Origin',(10.5223925513275,0.,82.4891652120952));
#37919=CARTESIAN_POINT('Ctrl Pts',(14.9938962568098,-5.,80.2143449012797));
#37920=CARTESIAN_POINT('Ctrl Pts',(14.9938962568098,5.,80.2143449012797));
#37921=CARTESIAN_POINT('Ctrl Pts',(14.9846094678237,-5.,80.2163662733741));
#37922=CARTESIAN_POINT('Ctrl Pts',(14.9846094678237,5.,80.2163662733741));
#37923=CARTESIAN_POINT('Ctrl Pts',(14.9660748535191,-5.,80.2203385484548));
#37924=CARTESIAN_POINT('Ctrl Pts',(14.9660748535191,5.,80.2203385484548));
#37925=CARTESIAN_POINT('Ctrl Pts',(14.9383898229852,-5.,80.2260855538497));
#37926=CARTESIAN_POINT('Ctrl Pts',(14.9383898229852,5.,80.2260855538497));
#37927=CARTESIAN_POINT('Ctrl Pts',(14.9017106547708,-5.,80.233324646843));
#37928=CARTESIAN_POINT('Ctrl Pts',(14.9017106547708,5.,80.233324646843));
#37929=CARTESIAN_POINT('Ctrl Pts',(14.8562549349791,-5.,80.2416626589468));
#37930=CARTESIAN_POINT('Ctrl Pts',(14.8562549349791,5.,80.2416626589468));
#37931=CARTESIAN_POINT('Ctrl Pts',(14.8111968676331,-5.,80.2492829096502));
#37932=CARTESIAN_POINT('Ctrl Pts',(14.8111968676331,5.,80.2492829096502));
#37933=CARTESIAN_POINT('Ctrl Pts',(14.7665419867659,-5.,80.256177526979));
#37934=CARTESIAN_POINT('Ctrl Pts',(14.7665419867659,5.,80.256177526979));
#37935=CARTESIAN_POINT('Ctrl Pts',(14.7222965373946,-5.,80.26233881843));
#37936=CARTESIAN_POINT('Ctrl Pts',(14.7222965373946,5.,80.26233881843));
#37937=CARTESIAN_POINT('Ctrl Pts',(14.6784669200222,-5.,80.2677605693635));
#37938=CARTESIAN_POINT('Ctrl Pts',(14.6784669200222,5.,80.2677605693635));
#37939=CARTESIAN_POINT('Ctrl Pts',(14.6350593161548,-5.,80.2724393512806));
#37940=CARTESIAN_POINT('Ctrl Pts',(14.6350593161548,5.,80.2724393512806));
#37941=CARTESIAN_POINT('Ctrl Pts',(14.5920831224637,-5.,80.2763745972856));
#37942=CARTESIAN_POINT('Ctrl Pts',(14.5920831224637,5.,80.2763745972856));
#37943=CARTESIAN_POINT('Ctrl Pts',(14.5495539352719,-5.,80.2795688335829));
#37944=CARTESIAN_POINT('Ctrl Pts',(14.5495539352719,5.,80.2795688335829));
#37945=CARTESIAN_POINT('Ctrl Pts',(14.5074969875316,-5.,80.2820281459137));
#37946=CARTESIAN_POINT('Ctrl Pts',(14.5074969875316,5.,80.2820281459137));
#37947=CARTESIAN_POINT('Ctrl Pts',(14.4659496024287,-5.,80.28376247754));
#37948=CARTESIAN_POINT('Ctrl Pts',(14.4659496024287,5.,80.28376247754));
#37949=CARTESIAN_POINT('Ctrl Pts',(14.4249659139275,-5.,80.2847868227605));
#37950=CARTESIAN_POINT('Ctrl Pts',(14.4249659139275,5.,80.2847868227605));
#37951=CARTESIAN_POINT('Ctrl Pts',(14.3846137683172,-5.,80.2851199044676));
#37952=CARTESIAN_POINT('Ctrl Pts',(14.3846137683172,5.,80.2851199044676));
#37953=CARTESIAN_POINT('Ctrl Pts',(14.3449620850361,-5.,80.2847797396321));
#37954=CARTESIAN_POINT('Ctrl Pts',(14.3449620850361,5.,80.2847797396321));
#37955=CARTESIAN_POINT('Ctrl Pts',(14.306070120279,-5.,80.283779991567));
#37956=CARTESIAN_POINT('Ctrl Pts',(14.306070120279,5.,80.283779991567));
#37957=CARTESIAN_POINT('Ctrl Pts',(14.2679766612333,-5.,80.2821264209094));
#37958=CARTESIAN_POINT('Ctrl Pts',(14.2679766612333,5.,80.2821264209094));
#37959=CARTESIAN_POINT('Ctrl Pts',(14.2306868314505,-5.,80.2798126906777));
#37960=CARTESIAN_POINT('Ctrl Pts',(14.2306868314505,5.,80.2798126906777));
#37961=CARTESIAN_POINT('Ctrl Pts',(14.1941657077385,-5.,80.2768185424287));
#37962=CARTESIAN_POINT('Ctrl Pts',(14.1941657077385,5.,80.2768185424287));
#37963=CARTESIAN_POINT('Ctrl Pts',(14.1583780225859,-5.,80.2731232227952));
#37964=CARTESIAN_POINT('Ctrl Pts',(14.1583780225859,5.,80.2731232227952));
#37965=CARTESIAN_POINT('Ctrl Pts',(14.1233240451694,-5.,80.2687178148077));
#37966=CARTESIAN_POINT('Ctrl Pts',(14.1233240451694,5.,80.2687178148077));
#37967=CARTESIAN_POINT('Ctrl Pts',(14.0890743429602,-5.,80.2636173092121));
#37968=CARTESIAN_POINT('Ctrl Pts',(14.0890743429602,5.,80.2636173092121));
#37969=CARTESIAN_POINT('Ctrl Pts',(14.0558114681554,-5.,80.2578751926453));
#37970=CARTESIAN_POINT('Ctrl Pts',(14.0558114681554,5.,80.2578751926453));
#37971=CARTESIAN_POINT('Ctrl Pts',(14.023850772022,-5.,80.2515910685876));
#37972=CARTESIAN_POINT('Ctrl Pts',(14.023850772022,5.,80.2515910685876));
#37973=CARTESIAN_POINT('Ctrl Pts',(13.9935704520791,-5.,80.244887354488));
#37974=CARTESIAN_POINT('Ctrl Pts',(13.9935704520791,5.,80.244887354488));
#37975=CARTESIAN_POINT('Ctrl Pts',(13.9653519392474,-5.,80.2378897915872));
#37976=CARTESIAN_POINT('Ctrl Pts',(13.9653519392474,5.,80.2378897915872));
#37977=CARTESIAN_POINT('Ctrl Pts',(13.9395218145325,-5.,80.2307083643255));
#37978=CARTESIAN_POINT('Ctrl Pts',(13.9395218145325,5.,80.2307083643255));
#37979=CARTESIAN_POINT('Ctrl Pts',(13.9162779194248,-5.,80.2234136895821));
#37980=CARTESIAN_POINT('Ctrl Pts',(13.9162779194248,5.,80.2234136895821));
#37981=CARTESIAN_POINT('Ctrl Pts',(13.8998185107453,-5.,80.2175148057176));
#37982=CARTESIAN_POINT('Ctrl Pts',(13.8998185107453,5.,80.2175148057176));
#37983=CARTESIAN_POINT('Ctrl Pts',(13.8886839778468,-5.,80.2130605652718));
#37984=CARTESIAN_POINT('Ctrl Pts',(13.8886839778468,5.,80.2130605652718));
#37985=CARTESIAN_POINT('Ctrl Pts',(13.8817976955151,-5.,80.2100777051323));
#37986=CARTESIAN_POINT('Ctrl Pts',(13.8817976955151,5.,80.2100777051323));
#37987=CARTESIAN_POINT('Ctrl Pts',(13.8784887436653,-5.,80.2085829347521));
#37988=CARTESIAN_POINT('Ctrl Pts',(13.8784887436653,5.,80.2085829347521));
#37989=CARTESIAN_POINT('',(13.8784887436653,0.,80.2085829347521));
#37990=CARTESIAN_POINT('Ctrl Pts',(14.877084102819,4.8,80.237761066812));
#37991=CARTESIAN_POINT('Ctrl Pts',(14.877084102819,3.13333333333333,80.237761066812));
#37992=CARTESIAN_POINT('Ctrl Pts',(14.877084102819,1.46666666666667,80.237761066812));
#37993=CARTESIAN_POINT('Ctrl Pts',(14.877084102819,-1.73333333333333,80.237761066812));
#37994=CARTESIAN_POINT('Ctrl Pts',(14.877084102819,-3.26666666666667,80.237761066812));
#37995=CARTESIAN_POINT('Ctrl Pts',(14.877084102819,-4.8,80.237761066812));
#37996=CARTESIAN_POINT('Origin',(9.31000000000061,0.,78.0000000000004));
#37997=CARTESIAN_POINT('',(13.1243263529939,0.,80.659589154899));
#37998=CARTESIAN_POINT('',(13.5204349482691,0.,79.9735089425676));
#37999=CARTESIAN_POINT('Origin',(13.8784887436653,0.,80.2085829347521));
#38000=CARTESIAN_POINT('Ctrl Pts',(13.5069332996928,-5.,80.8521358415414));
#38001=CARTESIAN_POINT('Ctrl Pts',(13.5069332996928,5.,80.8521358415414));
#38002=CARTESIAN_POINT('Ctrl Pts',(13.5098822847458,-5.,80.8542540927002));
#38003=CARTESIAN_POINT('Ctrl Pts',(13.5098822847458,5.,80.8542540927002));
#38004=CARTESIAN_POINT('Ctrl Pts',(13.5159086585781,-5.,80.8587263580464));
#38005=CARTESIAN_POINT('Ctrl Pts',(13.5159086585781,5.,80.8587263580464));
#38006=CARTESIAN_POINT('Ctrl Pts',(13.5253334104161,-5.,80.8661420261559));
#38007=CARTESIAN_POINT('Ctrl Pts',(13.5253334104161,5.,80.8661420261559));
#38008=CARTESIAN_POINT('Ctrl Pts',(13.5386716980353,-5.,80.8774468502741));
#38009=CARTESIAN_POINT('Ctrl Pts',(13.5386716980353,5.,80.8774468502741));
#38010=CARTESIAN_POINT('Ctrl Pts',(13.5566110192161,-5.,80.8939293165766));
#38011=CARTESIAN_POINT('Ctrl Pts',(13.5566110192161,5.,80.8939293165766));
#38012=CARTESIAN_POINT('Ctrl Pts',(13.5757453800031,-5.,80.9127081471622));
#38013=CARTESIAN_POINT('Ctrl Pts',(13.5757453800031,5.,80.9127081471622));
#38014=CARTESIAN_POINT('Ctrl Pts',(13.5959147036475,-5.,80.9336473146984));
#38015=CARTESIAN_POINT('Ctrl Pts',(13.5959147036475,5.,80.9336473146984));
#38016=CARTESIAN_POINT('Ctrl Pts',(13.6168604503288,-5.,80.9565189839544));
#38017=CARTESIAN_POINT('Ctrl Pts',(13.6168604503288,5.,80.9565189839544));
#38018=CARTESIAN_POINT('Ctrl Pts',(13.6382830094757,-5.,80.9810556966881));
#38019=CARTESIAN_POINT('Ctrl Pts',(13.6382830094757,5.,80.9810556966881));
#38020=CARTESIAN_POINT('Ctrl Pts',(13.6598872657035,-5.,81.0069911329731));
#38021=CARTESIAN_POINT('Ctrl Pts',(13.6598872657035,5.,81.0069911329731));
#38022=CARTESIAN_POINT('Ctrl Pts',(13.6814292842305,-5.,81.0341019923499));
#38023=CARTESIAN_POINT('Ctrl Pts',(13.6814292842305,5.,81.0341019923499));
#38024=CARTESIAN_POINT('Ctrl Pts',(13.7027714681705,-5.,81.0622569232995));
#38025=CARTESIAN_POINT('Ctrl Pts',(13.7027714681705,5.,81.0622569232995));
#38026=CARTESIAN_POINT('Ctrl Pts',(13.7238655514223,-5.,81.091402307971));
#38027=CARTESIAN_POINT('Ctrl Pts',(13.7238655514223,5.,81.091402307971));
#38028=CARTESIAN_POINT('Ctrl Pts',(13.744719121722,-5.,81.1215334547618));
#38029=CARTESIAN_POINT('Ctrl Pts',(13.744719121722,5.,81.1215334547618));
#38030=CARTESIAN_POINT('Ctrl Pts',(13.7653677857709,-5.,81.1526705295447));
#38031=CARTESIAN_POINT('Ctrl Pts',(13.7653677857709,5.,81.1526705295447));
#38032=CARTESIAN_POINT('Ctrl Pts',(13.7858465494927,-5.,81.1848336474667));
#38033=CARTESIAN_POINT('Ctrl Pts',(13.7858465494927,5.,81.1848336474667));
#38034=CARTESIAN_POINT('Ctrl Pts',(13.8061583390971,-5.,81.2180152029123));
#38035=CARTESIAN_POINT('Ctrl Pts',(13.8061583390971,5.,81.2180152029123));
#38036=CARTESIAN_POINT('Ctrl Pts',(13.8262787721302,-5.,81.2521844855136));
#38037=CARTESIAN_POINT('Ctrl Pts',(13.8262787721302,5.,81.2521844855136));
#38038=CARTESIAN_POINT('Ctrl Pts',(13.8461663877157,-5.,81.2872970095613));
#38039=CARTESIAN_POINT('Ctrl Pts',(13.8461663877157,5.,81.2872970095613));
#38040=CARTESIAN_POINT('Ctrl Pts',(13.8657711229787,-5.,81.3233020975591));
#38041=CARTESIAN_POINT('Ctrl Pts',(13.8657711229787,5.,81.3233020975591));
#38042=CARTESIAN_POINT('Ctrl Pts',(13.8850428402732,-5.,81.3601503543448));
#38043=CARTESIAN_POINT('Ctrl Pts',(13.8850428402732,5.,81.3601503543448));
#38044=CARTESIAN_POINT('Ctrl Pts',(13.9039414871764,-5.,81.3978023956762));
#38045=CARTESIAN_POINT('Ctrl Pts',(13.9039414871764,5.,81.3978023956762));
#38046=CARTESIAN_POINT('Ctrl Pts',(13.9224397909821,-5.,81.4362308703506));
#38047=CARTESIAN_POINT('Ctrl Pts',(13.9224397909821,5.,81.4362308703506));
#38048=CARTESIAN_POINT('Ctrl Pts',(13.9405198648132,-5.,81.4754169688537));
#38049=CARTESIAN_POINT('Ctrl Pts',(13.9405198648132,5.,81.4754169688537));
#38050=CARTESIAN_POINT('Ctrl Pts',(13.9581717227552,-5.,81.515348447469));
#38051=CARTESIAN_POINT('Ctrl Pts',(13.9581717227552,5.,81.515348447469));
#38052=CARTESIAN_POINT('Ctrl Pts',(13.9753911574206,-5.,81.55601688499));
#38053=CARTESIAN_POINT('Ctrl Pts',(13.9753911574206,5.,81.55601688499));
#38054=CARTESIAN_POINT('Ctrl Pts',(13.9921780472216,-5.,81.5974152138281));
#38055=CARTESIAN_POINT('Ctrl Pts',(13.9921780472216,5.,81.5974152138281));
#38056=CARTESIAN_POINT('Ctrl Pts',(14.0085345739351,-5.,81.6395347836759));
#38057=CARTESIAN_POINT('Ctrl Pts',(14.0085345739351,5.,81.6395347836759));
#38058=CARTESIAN_POINT('Ctrl Pts',(14.0244642769442,-5.,81.6823663399542));
#38059=CARTESIAN_POINT('Ctrl Pts',(14.0244642769442,5.,81.6823663399542));
#38060=CARTESIAN_POINT('Ctrl Pts',(14.0399712065494,-5.,81.7259011540809));
#38061=CARTESIAN_POINT('Ctrl Pts',(14.0399712065494,5.,81.7259011540809));
#38062=CARTESIAN_POINT('Ctrl Pts',(14.052041552205,-5.,81.7612857920673));
#38063=CARTESIAN_POINT('Ctrl Pts',(14.052041552205,5.,81.7612857920673));
#38064=CARTESIAN_POINT('Ctrl Pts',(14.0609070147714,-5.,81.7881352345583));
#38065=CARTESIAN_POINT('Ctrl Pts',(14.0609070147714,5.,81.7881352345583));
#38066=CARTESIAN_POINT('Ctrl Pts',(14.0667342307623,-5.,81.8061728189791));
#38067=CARTESIAN_POINT('Ctrl Pts',(14.0667342307623,5.,81.8061728189791));
#38068=CARTESIAN_POINT('Ctrl Pts',(14.0696270656537,-5.,81.8152261002327));
#38069=CARTESIAN_POINT('Ctrl Pts',(14.0696270656537,5.,81.8152261002327));
#38070=CARTESIAN_POINT('Ctrl Pts',(14.0314999829639,-4.8,81.7023557245181));
#38071=CARTESIAN_POINT('Ctrl Pts',(14.0314999829639,-3.13333333333333,81.7023557245181));
#38072=CARTESIAN_POINT('Ctrl Pts',(14.0314999829639,-1.46666666666667,81.7023557245181));
#38073=CARTESIAN_POINT('Ctrl Pts',(14.0314999829639,1.73333333333333,81.7023557245181));
#38074=CARTESIAN_POINT('Ctrl Pts',(14.0314999829639,3.26666666666667,81.7023557245181));
#38075=CARTESIAN_POINT('Ctrl Pts',(14.0314999829639,4.8,81.7023557245181));
#38076=CARTESIAN_POINT('',(13.5069332996928,0.,80.8521358415414));
#38077=CARTESIAN_POINT('Origin',(13.1243263529939,0.,80.659589154899));
#38078=CARTESIAN_POINT('Ctrl Pts',(3.21153406965502,-5.,77.8632034487949));
#38079=CARTESIAN_POINT('Ctrl Pts',(3.21153406965502,5.,77.8632034487949));
#38080=CARTESIAN_POINT('Ctrl Pts',(3.21956944675077,-5.,77.8581277114052));
#38081=CARTESIAN_POINT('Ctrl Pts',(3.21956944675077,5.,77.8581277114052));
#38082=CARTESIAN_POINT('Ctrl Pts',(3.23562768892862,-5.,77.8480557822981));
#38083=CARTESIAN_POINT('Ctrl Pts',(3.23562768892862,5.,77.8480557822981));
#38084=CARTESIAN_POINT('Ctrl Pts',(3.2596775161963,-5.,77.833186525534));
#38085=CARTESIAN_POINT('Ctrl Pts',(3.2596775161963,5.,77.833186525534));
#38086=CARTESIAN_POINT('Ctrl Pts',(3.29166874426794,-5.,77.8138389888443));
#38087=CARTESIAN_POINT('Ctrl Pts',(3.29166874426794,5.,77.8138389888443));
#38088=CARTESIAN_POINT('Ctrl Pts',(3.33153138063963,-5.,77.7904570486231));
#38089=CARTESIAN_POINT('Ctrl Pts',(3.33153138063963,5.,77.7904570486231));
#38090=CARTESIAN_POINT('Ctrl Pts',(3.37126583481311,-5.,77.7678855886958));
#38091=CARTESIAN_POINT('Ctrl Pts',(3.37126583481311,5.,77.7678855886958));
#38092=CARTESIAN_POINT('Ctrl Pts',(3.41086959886361,-5.,77.7461338990146));
#38093=CARTESIAN_POINT('Ctrl Pts',(3.41086959886361,5.,77.7461338990146));
#38094=CARTESIAN_POINT('Ctrl Pts',(3.45033943537775,-5.,77.7252113440577));
#38095=CARTESIAN_POINT('Ctrl Pts',(3.45033943537775,5.,77.7252113440577));
#38096=CARTESIAN_POINT('Ctrl Pts',(3.48967145537702,-5.,77.7051259527562));
#38097=CARTESIAN_POINT('Ctrl Pts',(3.48967145537702,5.,77.7051259527562));
#38098=CARTESIAN_POINT('Ctrl Pts',(3.52886102276024,-5.,77.6858830610395));
#38099=CARTESIAN_POINT('Ctrl Pts',(3.52886102276024,5.,77.6858830610395));
#38100=CARTESIAN_POINT('Ctrl Pts',(3.56789950143585,-5.,77.6674864154709));
#38101=CARTESIAN_POINT('Ctrl Pts',(3.56789950143585,5.,77.6674864154709));
#38102=CARTESIAN_POINT('Ctrl Pts',(3.60677137164422,-5.,77.6499389764635));
#38103=CARTESIAN_POINT('Ctrl Pts',(3.60677137164422,5.,77.6499389764635));
#38104=CARTESIAN_POINT('Ctrl Pts',(3.64545084072427,-5.,77.6332436554839));
#38105=CARTESIAN_POINT('Ctrl Pts',(3.64545084072427,5.,77.6332436554839));
#38106=CARTESIAN_POINT('Ctrl Pts',(3.68389943556033,-5.,77.6174038742161));
#38107=CARTESIAN_POINT('Ctrl Pts',(3.68389943556033,5.,77.6174038742161));
#38108=CARTESIAN_POINT('Ctrl Pts',(3.72206115851557,-5.,77.6024240575425));
#38109=CARTESIAN_POINT('Ctrl Pts',(3.72206115851557,5.,77.6024240575425));
#38110=CARTESIAN_POINT('Ctrl Pts',(3.75986585132557,-5.,77.5883098164954));
#38111=CARTESIAN_POINT('Ctrl Pts',(3.75986585132557,5.,77.5883098164954));
#38112=CARTESIAN_POINT('Ctrl Pts',(3.79724258873478,-5.,77.5750677924921));
#38113=CARTESIAN_POINT('Ctrl Pts',(3.79724258873478,5.,77.5750677924921));
#38114=CARTESIAN_POINT('Ctrl Pts',(3.834131015004,-5.,77.5627054130235));
#38115=CARTESIAN_POINT('Ctrl Pts',(3.834131015004,5.,77.5627054130235));
#38116=CARTESIAN_POINT('Ctrl Pts',(3.87049271184419,-5.,77.5512305308539));
#38117=CARTESIAN_POINT('Ctrl Pts',(3.87049271184419,5.,77.5512305308539));
#38118=CARTESIAN_POINT('Ctrl Pts',(3.90632503206606,-5.,77.5406508531519));
#38119=CARTESIAN_POINT('Ctrl Pts',(3.90632503206606,5.,77.5406508531519));
#38120=CARTESIAN_POINT('Ctrl Pts',(3.94166772153233,-5.,77.5309734721948));
#38121=CARTESIAN_POINT('Ctrl Pts',(3.94166772153233,5.,77.5309734721948));
#38122=CARTESIAN_POINT('Ctrl Pts',(3.97656101893436,-5.,77.5222058275747));
#38123=CARTESIAN_POINT('Ctrl Pts',(3.97656101893436,5.,77.5222058275747));
#38124=CARTESIAN_POINT('Ctrl Pts',(4.01100772111374,-5.,77.5143563905724));
#38125=CARTESIAN_POINT('Ctrl Pts',(4.01100772111374,5.,77.5143563905724));
#38126=CARTESIAN_POINT('Ctrl Pts',(4.04493638920223,-5.,77.5074352099941));
#38127=CARTESIAN_POINT('Ctrl Pts',(4.04493638920223,5.,77.5074352099941));
#38128=CARTESIAN_POINT('Ctrl Pts',(4.07815718673909,-5.,77.5014544613682));
#38129=CARTESIAN_POINT('Ctrl Pts',(4.07815718673909,5.,77.5014544613682));
#38130=CARTESIAN_POINT('Ctrl Pts',(4.11033971406609,-5.,77.4964284045146));
#38131=CARTESIAN_POINT('Ctrl Pts',(4.11033971406609,5.,77.4964284045146));
#38132=CARTESIAN_POINT('Ctrl Pts',(4.1410867125286,-5.,77.4923713558191));
#38133=CARTESIAN_POINT('Ctrl Pts',(4.1410867125286,5.,77.4923713558191));
#38134=CARTESIAN_POINT('Ctrl Pts',(4.16999674826609,-5.,77.4892956142181));
#38135=CARTESIAN_POINT('Ctrl Pts',(4.16999674826609,5.,77.4892956142181));
#38136=CARTESIAN_POINT('Ctrl Pts',(4.19672531862458,-5.,77.487209525431));
#38137=CARTESIAN_POINT('Ctrl Pts',(4.19672531862458,5.,77.487209525431));
#38138=CARTESIAN_POINT('Ctrl Pts',(4.22106236102637,-5.,77.4861143970901));
#38139=CARTESIAN_POINT('Ctrl Pts',(4.22106236102637,5.,77.4861143970901));
#38140=CARTESIAN_POINT('Ctrl Pts',(4.23854668300876,-5.,77.4860280854099));
#38141=CARTESIAN_POINT('Ctrl Pts',(4.23854668300876,5.,77.4860280854099));
#38142=CARTESIAN_POINT('Ctrl Pts',(4.25053316137149,-5.,77.4864054677697));
#38143=CARTESIAN_POINT('Ctrl Pts',(4.25053316137149,5.,77.4864054677697));
#38144=CARTESIAN_POINT('Ctrl Pts',(4.25802434832342,-5.,77.4868531921852));
#38145=CARTESIAN_POINT('Ctrl Pts',(4.25802434832342,5.,77.4868531921852));
#38146=CARTESIAN_POINT('Ctrl Pts',(4.2616449875437,-5.,77.4871260887099));
#38147=CARTESIAN_POINT('Ctrl Pts',(4.2616449875437,5.,77.4871260887099));
#38148=CARTESIAN_POINT('',(4.2616449875437,0.,77.4871260887099));
#38149=CARTESIAN_POINT('Ctrl Pts',(3.3132927884967,4.8,77.8012473408872));
#38150=CARTESIAN_POINT('Ctrl Pts',(3.3132927884967,3.13333333333333,77.8012473408872));
#38151=CARTESIAN_POINT('Ctrl Pts',(3.3132927884967,1.46666666666667,77.8012473408872));
#38152=CARTESIAN_POINT('Ctrl Pts',(3.3132927884967,-1.73333333333333,77.8012473408872));
#38153=CARTESIAN_POINT('Ctrl Pts',(3.3132927884967,-3.26666666666667,77.8012473408872));
#38154=CARTESIAN_POINT('Ctrl Pts',(3.3132927884967,-4.8,77.8012473408872));
#38155=CARTESIAN_POINT('Origin',(9.3100000000004,0.,78.0000000000001));
#38156=CARTESIAN_POINT('',(4.81607260887647,0.,76.805380142761));
#38157=CARTESIAN_POINT('',(4.67850553742098,0.,77.5855617740846));
#38158=CARTESIAN_POINT('Origin',(4.2616449875437,0.,77.4871260887099));
#38159=CARTESIAN_POINT('Ctrl Pts',(4.39068483903982,-5.,76.7553047249138));
#38160=CARTESIAN_POINT('Ctrl Pts',(4.39068483903982,5.,76.7553047249138));
#38161=CARTESIAN_POINT('Ctrl Pts',(4.38718921497661,-5.,76.754322832203));
#38162=CARTESIAN_POINT('Ctrl Pts',(4.38718921497661,5.,76.754322832203));
#38163=CARTESIAN_POINT('Ctrl Pts',(4.37999667111321,-5.,76.752181418671));
#38164=CARTESIAN_POINT('Ctrl Pts',(4.37999667111321,5.,76.752181418671));
#38165=CARTESIAN_POINT('Ctrl Pts',(4.36860399348183,-5.,76.7484364250207));
#38166=CARTESIAN_POINT('Ctrl Pts',(4.36860399348183,5.,76.7484364250207));
#38167=CARTESIAN_POINT('Ctrl Pts',(4.3522036254681,-5.,76.7423753282649));
#38168=CARTESIAN_POINT('Ctrl Pts',(4.3522036254681,5.,76.7423753282649));
#38169=CARTESIAN_POINT('Ctrl Pts',(4.32970884225672,-5.,76.7330224855494));
#38170=CARTESIAN_POINT('Ctrl Pts',(4.32970884225672,5.,76.7330224855494));
#38171=CARTESIAN_POINT('Ctrl Pts',(4.30530568630539,-5.,76.7219204938829));
#38172=CARTESIAN_POINT('Ctrl Pts',(4.30530568630539,5.,76.7219204938829));
#38173=CARTESIAN_POINT('Ctrl Pts',(4.27919110463543,-5.,76.7091424276514));
#38174=CARTESIAN_POINT('Ctrl Pts',(4.27919110463543,5.,76.7091424276514));
#38175=CARTESIAN_POINT('Ctrl Pts',(4.25168596944519,-5.,76.6948139561091));
#38176=CARTESIAN_POINT('Ctrl Pts',(4.25168596944519,5.,76.6948139561091));
#38177=CARTESIAN_POINT('Ctrl Pts',(4.22316329868605,-5.,76.6790839349482));
#38178=CARTESIAN_POINT('Ctrl Pts',(4.22316329868605,5.,76.6790839349482));
#38179=CARTESIAN_POINT('Ctrl Pts',(4.19399149688978,-5.,76.6621016876446));
#38180=CARTESIAN_POINT('Ctrl Pts',(4.19399149688978,5.,76.6621016876446));
#38181=CARTESIAN_POINT('Ctrl Pts',(4.16447616102936,-5.,76.6439936173946));
#38182=CARTESIAN_POINT('Ctrl Pts',(4.16447616102936,5.,76.6439936173946));
#38183=CARTESIAN_POINT('Ctrl Pts',(4.13479151474963,-5.,76.6248360933485));
#38184=CARTESIAN_POINT('Ctrl Pts',(4.13479151474963,5.,76.6248360933485));
#38185=CARTESIAN_POINT('Ctrl Pts',(4.1050012517344,-5.,76.6046629918244));
#38186=CARTESIAN_POINT('Ctrl Pts',(4.1050012517344,5.,76.6046629918244));
#38187=CARTESIAN_POINT('Ctrl Pts',(4.075099846465,-5.,76.5834813166402));
#38188=CARTESIAN_POINT('Ctrl Pts',(4.075099846465,5.,76.5834813166402));
#38189=CARTESIAN_POINT('Ctrl Pts',(4.04504694245075,-5.,76.561284296277));
#38190=CARTESIAN_POINT('Ctrl Pts',(4.04504694245075,5.,76.561284296277));
#38191=CARTESIAN_POINT('Ctrl Pts',(4.01480276509665,-5.,76.5380650014064));
#38192=CARTESIAN_POINT('Ctrl Pts',(4.01480276509665,5.,76.5380650014064));
#38193=CARTESIAN_POINT('Ctrl Pts',(3.98436716593925,-5.,76.5138315797934));
#38194=CARTESIAN_POINT('Ctrl Pts',(3.98436716593925,5.,76.5138315797934));
#38195=CARTESIAN_POINT('Ctrl Pts',(3.95377356055623,-5.,76.4886045504577));
#38196=CARTESIAN_POINT('Ctrl Pts',(3.95377356055623,5.,76.4886045504577));
#38197=CARTESIAN_POINT('Ctrl Pts',(3.92307612443753,-5.,76.4624115358435));
#38198=CARTESIAN_POINT('Ctrl Pts',(3.92307612443753,5.,76.4624115358435));
#38199=CARTESIAN_POINT('Ctrl Pts',(3.89233923402299,-5.,76.4352830347124));
#38200=CARTESIAN_POINT('Ctrl Pts',(3.89233923402299,5.,76.4352830347124));
#38201=CARTESIAN_POINT('Ctrl Pts',(3.86162689742974,-5.,76.4072483152511));
#38202=CARTESIAN_POINT('Ctrl Pts',(3.86162689742974,5.,76.4072483152511));
#38203=CARTESIAN_POINT('Ctrl Pts',(3.83099022182655,-5.,76.3783306878011));
#38204=CARTESIAN_POINT('Ctrl Pts',(3.83099022182655,5.,76.3783306878011));
#38205=CARTESIAN_POINT('Ctrl Pts',(3.80046418983392,-5.,76.3485465262618));
#38206=CARTESIAN_POINT('Ctrl Pts',(3.80046418983392,5.,76.3485465262618));
#38207=CARTESIAN_POINT('Ctrl Pts',(3.77007204284776,-5.,76.3179073881124));
#38208=CARTESIAN_POINT('Ctrl Pts',(3.77007204284776,5.,76.3179073881124));
#38209=CARTESIAN_POINT('Ctrl Pts',(3.73982735215308,-5.,76.2864213632901));
#38210=CARTESIAN_POINT('Ctrl Pts',(3.73982735215308,5.,76.2864213632901));
#38211=CARTESIAN_POINT('Ctrl Pts',(3.70973695162212,-5.,76.2540949261254));
#38212=CARTESIAN_POINT('Ctrl Pts',(3.70973695162212,5.,76.2540949261254));
#38213=CARTESIAN_POINT('Ctrl Pts',(3.67980337276852,-5.,76.2209346763969));
#38214=CARTESIAN_POINT('Ctrl Pts',(3.67980337276852,5.,76.2209346763969));
#38215=CARTESIAN_POINT('Ctrl Pts',(3.65002752397655,-5.,76.1869494889609));
#38216=CARTESIAN_POINT('Ctrl Pts',(3.65002752397655,5.,76.1869494889609));
#38217=CARTESIAN_POINT('Ctrl Pts',(3.62040924457333,-5.,76.1521492708398));
#38218=CARTESIAN_POINT('Ctrl Pts',(3.62040924457333,5.,76.1521492708398));
#38219=CARTESIAN_POINT('Ctrl Pts',(3.59094771387985,-5.,76.1165436095273));
#38220=CARTESIAN_POINT('Ctrl Pts',(3.59094771387985,5.,76.1165436095273));
#38221=CARTESIAN_POINT('Ctrl Pts',(3.56750304019246,-5.,76.0874212277101));
#38222=CARTESIAN_POINT('Ctrl Pts',(3.56750304019246,5.,76.0874212277101));
#38223=CARTESIAN_POINT('Ctrl Pts',(3.54998918028979,-5.,76.0652231715713));
#38224=CARTESIAN_POINT('Ctrl Pts',(3.54998918028979,5.,76.0652231715713));
#38225=CARTESIAN_POINT('Ctrl Pts',(3.53834417123289,-5.,76.0502664119026));
#38226=CARTESIAN_POINT('Ctrl Pts',(3.53834417123289,5.,76.0502664119026));
#38227=CARTESIAN_POINT('Ctrl Pts',(3.53252939109094,-5.,76.0427485181531));
#38228=CARTESIAN_POINT('Ctrl Pts',(3.53252939109094,5.,76.0427485181531));
#38229=CARTESIAN_POINT('Ctrl Pts',(3.60696107145242,-4.8,76.1357717469497));
#38230=CARTESIAN_POINT('Ctrl Pts',(3.60696107145242,-3.13333333333333,76.1357717469497));
#38231=CARTESIAN_POINT('Ctrl Pts',(3.60696107145242,-1.46666666666667,76.1357717469497));
#38232=CARTESIAN_POINT('Ctrl Pts',(3.60696107145242,1.73333333333333,76.1357717469497));
#38233=CARTESIAN_POINT('Ctrl Pts',(3.60696107145241,3.26666666666667,76.1357717469497));
#38234=CARTESIAN_POINT('Ctrl Pts',(3.60696107145241,4.8,76.1357717469497));
#38235=CARTESIAN_POINT('',(4.39068483903982,0.,76.7553047249138));
#38236=CARTESIAN_POINT('Origin',(4.81607260887647,0.,76.805380142761));
#38237=CARTESIAN_POINT('Ctrl Pts',(14.0696270656537,-5.,74.1847738997673));
#38238=CARTESIAN_POINT('Ctrl Pts',(14.0696270656537,5.,74.1847738997673));
#38239=CARTESIAN_POINT('Ctrl Pts',(14.0667342307623,-5.,74.1938271809842));
#38240=CARTESIAN_POINT('Ctrl Pts',(14.0667342307623,5.,74.1938271809842));
#38241=CARTESIAN_POINT('Ctrl Pts',(14.0609070147712,-5.,74.211864765341));
#38242=CARTESIAN_POINT('Ctrl Pts',(14.0609070147712,5.,74.211864765341));
#38243=CARTESIAN_POINT('Ctrl Pts',(14.0520415522048,-5.,74.238714207763));
#38244=CARTESIAN_POINT('Ctrl Pts',(14.0520415522048,5.,74.238714207763));
#38245=CARTESIAN_POINT('Ctrl Pts',(14.0399712065491,-5.,74.2740988457103));
#38246=CARTESIAN_POINT('Ctrl Pts',(14.0399712065491,5.,74.2740988457103));
#38247=CARTESIAN_POINT('Ctrl Pts',(14.0244642769439,-5.,74.3176336598548));
#38248=CARTESIAN_POINT('Ctrl Pts',(14.0244642769439,5.,74.3176336598548));
#38249=CARTESIAN_POINT('Ctrl Pts',(14.008534573935,-5.,74.3604652161928));
#38250=CARTESIAN_POINT('Ctrl Pts',(14.008534573935,5.,74.3604652161928));
#38251=CARTESIAN_POINT('Ctrl Pts',(13.9921780472215,-5.,74.4025847861155));
#38252=CARTESIAN_POINT('Ctrl Pts',(13.9921780472215,5.,74.4025847861155));
#38253=CARTESIAN_POINT('Ctrl Pts',(13.9753911574206,-5.,74.4439831150199));
#38254=CARTESIAN_POINT('Ctrl Pts',(13.9753911574206,5.,74.4439831150199));
#38255=CARTESIAN_POINT('Ctrl Pts',(13.9581717227553,-5.,74.4846515525832));
#38256=CARTESIAN_POINT('Ctrl Pts',(13.9581717227553,5.,74.4846515525832));
#38257=CARTESIAN_POINT('Ctrl Pts',(13.9405198648132,-5.,74.5245830312134));
#38258=CARTESIAN_POINT('Ctrl Pts',(13.9405198648132,5.,74.5245830312134));
#38259=CARTESIAN_POINT('Ctrl Pts',(13.922439790982,-5.,74.5637691297076));
#38260=CARTESIAN_POINT('Ctrl Pts',(13.922439790982,5.,74.5637691297076));
#38261=CARTESIAN_POINT('Ctrl Pts',(13.9039414871763,-5.,74.6021976043591));
#38262=CARTESIAN_POINT('Ctrl Pts',(13.9039414871763,5.,74.6021976043591));
#38263=CARTESIAN_POINT('Ctrl Pts',(13.8850428402731,-5.,74.6398496456646));
#38264=CARTESIAN_POINT('Ctrl Pts',(13.8850428402731,5.,74.6398496456646));
#38265=CARTESIAN_POINT('Ctrl Pts',(13.8657711229787,-5.,74.6766979024311));
#38266=CARTESIAN_POINT('Ctrl Pts',(13.8657711229787,5.,74.6766979024311));
#38267=CARTESIAN_POINT('Ctrl Pts',(13.8461663877159,-5.,74.7127029904214));
#38268=CARTESIAN_POINT('Ctrl Pts',(13.8461663877159,5.,74.7127029904214));
#38269=CARTESIAN_POINT('Ctrl Pts',(13.8262787721306,-5.,74.7478155144712));
#38270=CARTESIAN_POINT('Ctrl Pts',(13.8262787721306,5.,74.7478155144712));
#38271=CARTESIAN_POINT('Ctrl Pts',(13.8061583390975,-5.,74.78198479708));
#38272=CARTESIAN_POINT('Ctrl Pts',(13.8061583390975,5.,74.78198479708));
#38273=CARTESIAN_POINT('Ctrl Pts',(13.785846549493,-5.,74.8151663525327));
#38274=CARTESIAN_POINT('Ctrl Pts',(13.785846549493,5.,74.8151663525327));
#38275=CARTESIAN_POINT('Ctrl Pts',(13.7653677857709,-5.,74.8473294704568));
#38276=CARTESIAN_POINT('Ctrl Pts',(13.7653677857709,5.,74.8473294704568));
#38277=CARTESIAN_POINT('Ctrl Pts',(13.7447191217217,-5.,74.8784665452351));
#38278=CARTESIAN_POINT('Ctrl Pts',(13.7447191217217,5.,74.8784665452351));
#38279=CARTESIAN_POINT('Ctrl Pts',(13.7238655514216,-5.,74.9085976920185));
#38280=CARTESIAN_POINT('Ctrl Pts',(13.7238655514216,5.,74.9085976920185));
#38281=CARTESIAN_POINT('Ctrl Pts',(13.7027714681697,-5.,74.9377430766853));
#38282=CARTESIAN_POINT('Ctrl Pts',(13.7027714681697,5.,74.9377430766853));
#38283=CARTESIAN_POINT('Ctrl Pts',(13.6814292842299,-5.,74.9658980076382));
#38284=CARTESIAN_POINT('Ctrl Pts',(13.6814292842299,5.,74.9658980076382));
#38285=CARTESIAN_POINT('Ctrl Pts',(13.6598872657036,-5.,74.9930088670283));
#38286=CARTESIAN_POINT('Ctrl Pts',(13.6598872657036,5.,74.9930088670283));
#38287=CARTESIAN_POINT('Ctrl Pts',(13.6382830094766,-5.,75.0189443033331));
#38288=CARTESIAN_POINT('Ctrl Pts',(13.6382830094766,5.,75.0189443033331));
#38289=CARTESIAN_POINT('Ctrl Pts',(13.6168604503304,-5.,75.0434810160819));
#38290=CARTESIAN_POINT('Ctrl Pts',(13.6168604503304,5.,75.0434810160819));
#38291=CARTESIAN_POINT('Ctrl Pts',(13.5959147036489,-5.,75.0663526853374));
#38292=CARTESIAN_POINT('Ctrl Pts',(13.5959147036489,5.,75.0663526853374));
#38293=CARTESIAN_POINT('Ctrl Pts',(13.5757453800036,-5.,75.0872918528514));
#38294=CARTESIAN_POINT('Ctrl Pts',(13.5757453800036,5.,75.0872918528514));
#38295=CARTESIAN_POINT('Ctrl Pts',(13.556611019215,-5.,75.1060706833974));
#38296=CARTESIAN_POINT('Ctrl Pts',(13.556611019215,5.,75.1060706833974));
#38297=CARTESIAN_POINT('Ctrl Pts',(13.5386716980329,-5.,75.1225531496632));
#38298=CARTESIAN_POINT('Ctrl Pts',(13.5386716980329,5.,75.1225531496632));
#38299=CARTESIAN_POINT('Ctrl Pts',(13.5253334104135,-5.,75.1338579737778));
#38300=CARTESIAN_POINT('Ctrl Pts',(13.5253334104135,5.,75.1338579737778));
#38301=CARTESIAN_POINT('Ctrl Pts',(13.5159086585763,-5.,75.1412736419094));
#38302=CARTESIAN_POINT('Ctrl Pts',(13.5159086585763,5.,75.1412736419094));
#38303=CARTESIAN_POINT('Ctrl Pts',(13.5098822847451,-5.,75.145745907283));
#38304=CARTESIAN_POINT('Ctrl Pts',(13.5098822847451,5.,75.145745907283));
#38305=CARTESIAN_POINT('Ctrl Pts',(13.5069332996928,-5.,75.1478641584586));
#38306=CARTESIAN_POINT('Ctrl Pts',(13.5069332996928,5.,75.1478641584586));
#38307=CARTESIAN_POINT('',(13.5069332996928,0.,75.1478641584586));
#38308=CARTESIAN_POINT('Ctrl Pts',(14.0314999829165,4.8,74.2976442754215));
#38309=CARTESIAN_POINT('Ctrl Pts',(14.0314999829165,3.13333333333333,74.2976442754215));
#38310=CARTESIAN_POINT('Ctrl Pts',(14.0314999829165,1.46666666666667,74.2976442754215));
#38311=CARTESIAN_POINT('Ctrl Pts',(14.0314999829165,-1.73333333333333,74.2976442754215));
#38312=CARTESIAN_POINT('Ctrl Pts',(14.0314999829165,-3.26666666666667,74.2976442754215));
#38313=CARTESIAN_POINT('Ctrl Pts',(14.0314999829165,-4.8,74.2976442754215));
#38314=CARTESIAN_POINT('Origin',(9.31000000000134,0.,77.9999999999992));
#38315=CARTESIAN_POINT('',(13.5204349482691,0.,76.0264910574324));
#38316=CARTESIAN_POINT('',(13.1243263529939,0.,75.340410845101));
#38317=CARTESIAN_POINT('Origin',(13.5069332996928,0.,75.1478641584586));
#38318=CARTESIAN_POINT('Ctrl Pts',(13.8784887436653,-5.,75.7914170652479));
#38319=CARTESIAN_POINT('Ctrl Pts',(13.8784887436653,5.,75.7914170652479));
#38320=CARTESIAN_POINT('Ctrl Pts',(13.8817976955159,-5.,75.7899222948501));
#38321=CARTESIAN_POINT('Ctrl Pts',(13.8817976955159,5.,75.7899222948501));
#38322=CARTESIAN_POINT('Ctrl Pts',(13.8886839778489,-5.,75.7869394346819));
#38323=CARTESIAN_POINT('Ctrl Pts',(13.8886839778489,5.,75.7869394346819));
#38324=CARTESIAN_POINT('Ctrl Pts',(13.8998185107484,-5.,75.7824851942128));
#38325=CARTESIAN_POINT('Ctrl Pts',(13.8998185107484,5.,75.7824851942128));
#38326=CARTESIAN_POINT('Ctrl Pts',(13.9162779194277,-5.,75.7765863103522));
#38327=CARTESIAN_POINT('Ctrl Pts',(13.9162779194277,5.,75.7765863103522));
#38328=CARTESIAN_POINT('Ctrl Pts',(13.9395218145337,-5.,75.7692916356475));
#38329=CARTESIAN_POINT('Ctrl Pts',(13.9395218145337,5.,75.7692916356475));
#38330=CARTESIAN_POINT('Ctrl Pts',(13.9653519392467,-5.,75.762110208427));
#38331=CARTESIAN_POINT('Ctrl Pts',(13.9653519392467,5.,75.762110208427));
#38332=CARTESIAN_POINT('Ctrl Pts',(13.9935704520776,-5.,75.7551126455491));
#38333=CARTESIAN_POINT('Ctrl Pts',(13.9935704520776,5.,75.7551126455491));
#38334=CARTESIAN_POINT('Ctrl Pts',(14.0238507720205,-5.,75.7484089314496));
#38335=CARTESIAN_POINT('Ctrl Pts',(14.0238507720205,5.,75.7484089314496));
#38336=CARTESIAN_POINT('Ctrl Pts',(14.0558114681545,-5.,75.7421248073761));
#38337=CARTESIAN_POINT('Ctrl Pts',(14.0558114681545,5.,75.7421248073761));
#38338=CARTESIAN_POINT('Ctrl Pts',(14.0890743429601,-5.,75.7363826907892));
#38339=CARTESIAN_POINT('Ctrl Pts',(14.0890743429601,5.,75.7363826907892));
#38340=CARTESIAN_POINT('Ctrl Pts',(14.1233240451699,-5.,75.7312821851806));
#38341=CARTESIAN_POINT('Ctrl Pts',(14.1233240451699,5.,75.7312821851806));
#38342=CARTESIAN_POINT('Ctrl Pts',(14.1583780225866,-5.,75.7268767771904));
#38343=CARTESIAN_POINT('Ctrl Pts',(14.1583780225866,5.,75.7268767771904));
#38344=CARTESIAN_POINT('Ctrl Pts',(14.1941657077391,-5.,75.7231814575622));
#38345=CARTESIAN_POINT('Ctrl Pts',(14.1941657077391,5.,75.7231814575622));
#38346=CARTESIAN_POINT('Ctrl Pts',(14.2306868314508,-5.,75.7201873093207));
#38347=CARTESIAN_POINT('Ctrl Pts',(14.2306868314508,5.,75.7201873093207));
#38348=CARTESIAN_POINT('Ctrl Pts',(14.2679766612333,-5.,75.7178735790925));
#38349=CARTESIAN_POINT('Ctrl Pts',(14.2679766612333,5.,75.7178735790925));
#38350=CARTESIAN_POINT('Ctrl Pts',(14.3060701202788,-5.,75.7162200084309));
#38351=CARTESIAN_POINT('Ctrl Pts',(14.3060701202788,5.,75.7162200084309));
#38352=CARTESIAN_POINT('Ctrl Pts',(14.3449620850358,-5.,75.7152202603571));
#38353=CARTESIAN_POINT('Ctrl Pts',(14.3449620850358,5.,75.7152202603571));
#38354=CARTESIAN_POINT('Ctrl Pts',(14.384613768317,-5.,75.7148800955132));
#38355=CARTESIAN_POINT('Ctrl Pts',(14.384613768317,5.,75.7148800955132));
#38356=CARTESIAN_POINT('Ctrl Pts',(14.4249659139274,-5.,75.7152131772188));
#38357=CARTESIAN_POINT('Ctrl Pts',(14.4249659139274,5.,75.7152131772188));
#38358=CARTESIAN_POINT('Ctrl Pts',(14.4659496024287,-5.,75.7162375224487));
#38359=CARTESIAN_POINT('Ctrl Pts',(14.4659496024287,5.,75.7162375224487));
#38360=CARTESIAN_POINT('Ctrl Pts',(14.5074969875316,-5.,75.7179718540974));
#38361=CARTESIAN_POINT('Ctrl Pts',(14.5074969875316,5.,75.7179718540974));
#38362=CARTESIAN_POINT('Ctrl Pts',(14.5495539352719,-5.,75.7204311664575));
#38363=CARTESIAN_POINT('Ctrl Pts',(14.5495539352719,5.,75.7204311664575));
#38364=CARTESIAN_POINT('Ctrl Pts',(14.5920831224634,-5.,75.7236254027807));
#38365=CARTESIAN_POINT('Ctrl Pts',(14.5920831224634,5.,75.7236254027807));
#38366=CARTESIAN_POINT('Ctrl Pts',(14.6350593161544,-5.,75.7275606487953));
#38367=CARTESIAN_POINT('Ctrl Pts',(14.6350593161544,5.,75.7275606487953));
#38368=CARTESIAN_POINT('Ctrl Pts',(14.6784669200218,-5.,75.7322394306956));
#38369=CARTESIAN_POINT('Ctrl Pts',(14.6784669200218,5.,75.7322394306956));
#38370=CARTESIAN_POINT('Ctrl Pts',(14.7222965373945,-5.,75.7376611815812));
#38371=CARTESIAN_POINT('Ctrl Pts',(14.7222965373945,5.,75.7376611815812));
#38372=CARTESIAN_POINT('Ctrl Pts',(14.7665419867663,-5.,75.7438224729572));
#38373=CARTESIAN_POINT('Ctrl Pts',(14.7665419867663,5.,75.7438224729572));
#38374=CARTESIAN_POINT('Ctrl Pts',(14.8111968676342,-5.,75.7507170902014));
#38375=CARTESIAN_POINT('Ctrl Pts',(14.8111968676342,5.,75.7507170902014));
#38376=CARTESIAN_POINT('Ctrl Pts',(14.8562549349808,-5.,75.7583373408378));
#38377=CARTESIAN_POINT('Ctrl Pts',(14.8562549349808,5.,75.7583373408378));
#38378=CARTESIAN_POINT('Ctrl Pts',(14.9017106547726,-5.,75.7666753529216));
#38379=CARTESIAN_POINT('Ctrl Pts',(14.9017106547726,5.,75.7666753529216));
#38380=CARTESIAN_POINT('Ctrl Pts',(14.9383898229867,-5.,75.7739144459592));
#38381=CARTESIAN_POINT('Ctrl Pts',(14.9383898229867,5.,75.7739144459592));
#38382=CARTESIAN_POINT('Ctrl Pts',(14.96607485352,-5.,75.7796614514317));
#38383=CARTESIAN_POINT('Ctrl Pts',(14.96607485352,5.,75.7796614514317));
#38384=CARTESIAN_POINT('Ctrl Pts',(14.984609467824,-5.,75.7836337265846));
#38385=CARTESIAN_POINT('Ctrl Pts',(14.984609467824,5.,75.7836337265846));
#38386=CARTESIAN_POINT('Ctrl Pts',(14.9938962568098,-5.,75.7856550987203));
#38387=CARTESIAN_POINT('Ctrl Pts',(14.9938962568098,5.,75.7856550987203));
#38388=CARTESIAN_POINT('Ctrl Pts',(14.8770841027247,-4.8,75.7622389329533));
#38389=CARTESIAN_POINT('Ctrl Pts',(14.8770841027247,-3.13333333333333,75.7622389329533));
#38390=CARTESIAN_POINT('Ctrl Pts',(14.8770841027247,-1.46666666666667,75.7622389329533));
#38391=CARTESIAN_POINT('Ctrl Pts',(14.8770841027247,1.73333333333333,75.7622389329533));
#38392=CARTESIAN_POINT('Ctrl Pts',(14.8770841027247,3.26666666666667,75.7622389329533));
#38393=CARTESIAN_POINT('Ctrl Pts',(14.8770841027247,4.8,75.7622389329533));
#38394=CARTESIAN_POINT('',(13.8784887436653,0.,75.7914170652479));
#38395=CARTESIAN_POINT('Origin',(13.5204349482691,0.,76.0264910574324));
#38396=CARTESIAN_POINT('Ctrl Pts',(10.5037057995804,-5.,72.0179379421433));
#38397=CARTESIAN_POINT('Ctrl Pts',(10.5037057995804,5.,72.0179379421433));
#38398=CARTESIAN_POINT('Ctrl Pts',(10.507309096492,-5.,72.0267326363238));
#38399=CARTESIAN_POINT('Ctrl Pts',(10.507309096492,5.,72.0267326363238));
#38400=CARTESIAN_POINT('Ctrl Pts',(10.514439525817,-5.,72.0442958898031));
#38401=CARTESIAN_POINT('Ctrl Pts',(10.514439525817,5.,72.0442958898031));
#38402=CARTESIAN_POINT('Ctrl Pts',(10.5249066764203,-5.,72.070562365439));
#38403=CARTESIAN_POINT('Ctrl Pts',(10.5249066764203,5.,72.070562365439));
#38404=CARTESIAN_POINT('Ctrl Pts',(10.5384050620625,-5.,72.1054272393282));
#38405=CARTESIAN_POINT('Ctrl Pts',(10.5384050620625,5.,72.1054272393282));
#38406=CARTESIAN_POINT('Ctrl Pts',(10.554509703925,-5.,72.1487445040063));
#38407=CARTESIAN_POINT('Ctrl Pts',(10.554509703925,5.,72.1487445040063));
#38408=CARTESIAN_POINT('Ctrl Pts',(10.5698384371529,-5.,72.1917947954702));
#38409=CARTESIAN_POINT('Ctrl Pts',(10.5698384371529,5.,72.1917947954702));
#38410=CARTESIAN_POINT('Ctrl Pts',(10.584382548403,-5.,72.2345740306915));
#38411=CARTESIAN_POINT('Ctrl Pts',(10.584382548403,5.,72.2345740306915));
#38412=CARTESIAN_POINT('Ctrl Pts',(10.598133377614,-5.,72.2770773952961));
#38413=CARTESIAN_POINT('Ctrl Pts',(10.598133377614,5.,72.2770773952961));
#38414=CARTESIAN_POINT('Ctrl Pts',(10.6110836931323,-5.,72.3192996651659));
#38415=CARTESIAN_POINT('Ctrl Pts',(10.6110836931323,5.,72.3192996651659));
#38416=CARTESIAN_POINT('Ctrl Pts',(10.6232290451402,-5.,72.3612353480546));
#38417=CARTESIAN_POINT('Ctrl Pts',(10.6232290451402,5.,72.3612353480546));
#38418=CARTESIAN_POINT('Ctrl Pts',(10.6345672436375,-5.,72.4028752884915));
#38419=CARTESIAN_POINT('Ctrl Pts',(10.6345672436375,5.,72.4028752884915));
#38420=CARTESIAN_POINT('Ctrl Pts',(10.6450980681725,-5.,72.4442036884342));
#38421=CARTESIAN_POINT('Ctrl Pts',(10.6450980681725,5.,72.4442036884342));
#38422=CARTESIAN_POINT('Ctrl Pts',(10.6548231303688,-5.,72.4851946415082));
#38423=CARTESIAN_POINT('Ctrl Pts',(10.6548231303688,5.,72.4851946415082));
#38424=CARTESIAN_POINT('Ctrl Pts',(10.6637457413204,-5.,72.5258096649296));
#38425=CARTESIAN_POINT('Ctrl Pts',(10.6637457413204,5.,72.5258096649296));
#38426=CARTESIAN_POINT('Ctrl Pts',(10.6718712672619,-5.,72.5659928434235));
#38427=CARTESIAN_POINT('Ctrl Pts',(10.6718712672619,5.,72.5659928434235));
#38428=CARTESIAN_POINT('Ctrl Pts',(10.6792063652593,-5.,72.6056741102406));
#38429=CARTESIAN_POINT('Ctrl Pts',(10.6792063652593,5.,72.6056741102406));
#38430=CARTESIAN_POINT('Ctrl Pts',(10.6857568108318,-5.,72.6447824643664));
#38431=CARTESIAN_POINT('Ctrl Pts',(10.6857568108318,5.,72.6447824643664));
#38432=CARTESIAN_POINT('Ctrl Pts',(10.6915257699882,-5.,72.6832571772262));
#38433=CARTESIAN_POINT('Ctrl Pts',(10.6915257699882,5.,72.6832571772262));
#38434=CARTESIAN_POINT('Ctrl Pts',(10.6965121805263,-5.,72.721059050569));
#38435=CARTESIAN_POINT('Ctrl Pts',(10.6965121805263,5.,72.721059050569));
#38436=CARTESIAN_POINT('Ctrl Pts',(10.7007089120438,-5.,72.7581841390844));
#38437=CARTESIAN_POINT('Ctrl Pts',(10.7007089120438,5.,72.7581841390844));
#38438=CARTESIAN_POINT('Ctrl Pts',(10.704102078216,-5.,72.794670353247));
#38439=CARTESIAN_POINT('Ctrl Pts',(10.704102078216,5.,72.794670353247));
#38440=CARTESIAN_POINT('Ctrl Pts',(10.7066773651029,-5.,72.8305560285639));
#38441=CARTESIAN_POINT('Ctrl Pts',(10.7066773651029,5.,72.8305560285639));
#38442=CARTESIAN_POINT('Ctrl Pts',(10.7084259444594,-5.,72.8658424483676));
#38443=CARTESIAN_POINT('Ctrl Pts',(10.7084259444594,5.,72.8658424483676));
#38444=CARTESIAN_POINT('Ctrl Pts',(10.7093503253745,-5.,72.9004575141518));
#38445=CARTESIAN_POINT('Ctrl Pts',(10.7093503253745,5.,72.9004575141518));
#38446=CARTESIAN_POINT('Ctrl Pts',(10.7094714820477,-5.,72.9342121592384));
#38447=CARTESIAN_POINT('Ctrl Pts',(10.7094714820477,5.,72.9342121592384));
#38448=CARTESIAN_POINT('Ctrl Pts',(10.7088327445899,-5.,72.966778527284));
#38449=CARTESIAN_POINT('Ctrl Pts',(10.7088327445899,5.,72.966778527284));
#38450=CARTESIAN_POINT('Ctrl Pts',(10.707488997348,-5.,72.9977629088648));
#38451=CARTESIAN_POINT('Ctrl Pts',(10.707488997348,5.,72.9977629088648));
#38452=CARTESIAN_POINT('Ctrl Pts',(10.7054978364887,-5.,73.0267678331103));
#38453=CARTESIAN_POINT('Ctrl Pts',(10.7054978364887,5.,73.0267678331103));
#38454=CARTESIAN_POINT('Ctrl Pts',(10.7029108653431,-5.,73.0534525819188));
#38455=CARTESIAN_POINT('Ctrl Pts',(10.7029108653431,5.,73.0534525819188));
#38456=CARTESIAN_POINT('Ctrl Pts',(10.6997632731399,-5.,73.0776100569794));
#38457=CARTESIAN_POINT('Ctrl Pts',(10.6997632731399,5.,73.0776100569794));
#38458=CARTESIAN_POINT('Ctrl Pts',(10.6968121528997,-5.,73.0948437406871));
#38459=CARTESIAN_POINT('Ctrl Pts',(10.6968121528997,5.,73.0948437406871));
#38460=CARTESIAN_POINT('Ctrl Pts',(10.6943590737142,-5.,73.1065825857645));
#38461=CARTESIAN_POINT('Ctrl Pts',(10.6943590737142,5.,73.1065825857645));
#38462=CARTESIAN_POINT('Ctrl Pts',(10.6926173202913,-5.,73.1138822182422));
#38463=CARTESIAN_POINT('Ctrl Pts',(10.6926173202913,5.,73.1138822182422));
#38464=CARTESIAN_POINT('Ctrl Pts',(10.691719852285,-5.,73.1174004638434));
#38465=CARTESIAN_POINT('Ctrl Pts',(10.691719852285,5.,73.1174004638434));
#38466=CARTESIAN_POINT('',(10.691719852285,0.,73.1174004638434));
#38467=CARTESIAN_POINT('Ctrl Pts',(10.5470504387829,4.8,72.1289092826028));
#38468=CARTESIAN_POINT('Ctrl Pts',(10.5470504387829,3.13333333333333,72.1289092826028));
#38469=CARTESIAN_POINT('Ctrl Pts',(10.5470504387829,1.46666666666667,72.1289092826028));
#38470=CARTESIAN_POINT('Ctrl Pts',(10.5470504387829,-1.73333333333333,72.1289092826028));
#38471=CARTESIAN_POINT('Ctrl Pts',(10.5470504387829,-3.26666666666667,72.1289092826028));
#38472=CARTESIAN_POINT('Ctrl Pts',(10.5470504387829,-4.8,72.1289092826028));
#38473=CARTESIAN_POINT('Origin',(9.31000000000015,0.,77.9999999999997));
#38474=CARTESIAN_POINT('',(11.2668331993474,0.,73.7817890249619));
#38475=CARTESIAN_POINT('',(10.5223925513275,0.,73.5108347879048));
#38476=CARTESIAN_POINT('Origin',(10.691719852285,0.,73.1174004638434));
#38477=CARTESIAN_POINT('Ctrl Pts',(11.3900156701126,-5.,73.3715593562453));
#38478=CARTESIAN_POINT('Ctrl Pts',(11.3900156701126,5.,73.3715593562453));
#38479=CARTESIAN_POINT('Ctrl Pts',(11.3915896544057,-5.,73.3682873424408));
#38480=CARTESIAN_POINT('Ctrl Pts',(11.3915896544057,5.,73.3682873424408));
#38481=CARTESIAN_POINT('Ctrl Pts',(11.3949475071735,-5.,73.361575922029));
#38482=CARTESIAN_POINT('Ctrl Pts',(11.3949475071735,5.,73.361575922029));
#38483=CARTESIAN_POINT('Ctrl Pts',(11.4006139236521,-5.,73.3510066360857));
#38484=CARTESIAN_POINT('Ctrl Pts',(11.4006139236521,5.,73.3510066360857));
#38485=CARTESIAN_POINT('Ctrl Pts',(11.4094308327498,-5.,73.3359079249211));
#38486=CARTESIAN_POINT('Ctrl Pts',(11.4094308327498,5.,73.3359079249211));
#38487=CARTESIAN_POINT('Ctrl Pts',(11.4225477629013,-5.,73.3153789921175));
#38488=CARTESIAN_POINT('Ctrl Pts',(11.4225477629013,5.,73.3153789921175));
#38489=CARTESIAN_POINT('Ctrl Pts',(11.4377186539509,-5.,73.2932744155724));
#38490=CARTESIAN_POINT('Ctrl Pts',(11.4377186539509,5.,73.2932744155724));
#38491=CARTESIAN_POINT('Ctrl Pts',(11.454837342174,-5.,73.2697754609989));
#38492=CARTESIAN_POINT('Ctrl Pts',(11.454837342174,5.,73.2697754609989));
#38493=CARTESIAN_POINT('Ctrl Pts',(11.47372434864,-5.,73.2451763035876));
#38494=CARTESIAN_POINT('Ctrl Pts',(11.47372434864,5.,73.2451763035876));
#38495=CARTESIAN_POINT('Ctrl Pts',(11.4941683052251,-5.,73.2198184457917));
#38496=CARTESIAN_POINT('Ctrl Pts',(11.4941683052251,5.,73.2198184457917));
#38497=CARTESIAN_POINT('Ctrl Pts',(11.5159581842438,-5.,73.1940387655048));
#38498=CARTESIAN_POINT('Ctrl Pts',(11.5159581842438,5.,73.1940387655048));
#38499=CARTESIAN_POINT('Ctrl Pts',(11.5389164364967,-5.,73.1681162673142));
#38500=CARTESIAN_POINT('Ctrl Pts',(11.5389164364967,5.,73.1681162673142));
#38501=CARTESIAN_POINT('Ctrl Pts',(11.5629375994355,-5.,73.1422092666525));
#38502=CARTESIAN_POINT('Ctrl Pts',(11.5629375994355,5.,73.1422092666525));
#38503=CARTESIAN_POINT('Ctrl Pts',(11.5879772511062,-5.,73.116374606991));
#38504=CARTESIAN_POINT('Ctrl Pts',(11.5879772511062,5.,73.116374606991));
#38505=CARTESIAN_POINT('Ctrl Pts',(11.6140294535881,-5.,73.0906056305532));
#38506=CARTESIAN_POINT('Ctrl Pts',(11.6140294535881,5.,73.0906056305532));
#38507=CARTESIAN_POINT('Ctrl Pts',(11.6411078833532,-5.,73.0648637698139));
#38508=CARTESIAN_POINT('Ctrl Pts',(11.6411078833532,5.,73.0648637698139));
#38509=CARTESIAN_POINT('Ctrl Pts',(11.6692262712418,-5.,73.039111057708));
#38510=CARTESIAN_POINT('Ctrl Pts',(11.6692262712418,5.,73.039111057708));
#38511=CARTESIAN_POINT('Ctrl Pts',(11.6983766190533,-5.,73.0133459331853));
#38512=CARTESIAN_POINT('Ctrl Pts',(11.6983766190533,5.,73.0133459331853));
#38513=CARTESIAN_POINT('Ctrl Pts',(11.7285329169467,-5.,72.9875977410784));
#38514=CARTESIAN_POINT('Ctrl Pts',(11.7285329169467,5.,72.9875977410784));
#38515=CARTESIAN_POINT('Ctrl Pts',(11.7596585546536,-5.,72.9619150372466));
#38516=CARTESIAN_POINT('Ctrl Pts',(11.7596585546536,5.,72.9619150372466));
#38517=CARTESIAN_POINT('Ctrl Pts',(11.7917123179081,-5.,72.9363559240547));
#38518=CARTESIAN_POINT('Ctrl Pts',(11.7917123179081,5.,72.9363559240547));
#38519=CARTESIAN_POINT('Ctrl Pts',(11.8246542682811,-5.,72.9109783548261));
#38520=CARTESIAN_POINT('Ctrl Pts',(11.8246542682811,5.,72.9109783548261));
#38521=CARTESIAN_POINT('Ctrl Pts',(11.8584525748975,-5.,72.8858286124943));
#38522=CARTESIAN_POINT('Ctrl Pts',(11.8584525748975,5.,72.8858286124943));
#38523=CARTESIAN_POINT('Ctrl Pts',(11.8930850379397,-5.,72.8609383049106));
#38524=CARTESIAN_POINT('Ctrl Pts',(11.8930850379397,5.,72.8609383049106));
#38525=CARTESIAN_POINT('Ctrl Pts',(11.9285362396797,-5.,72.8363283134386));
#38526=CARTESIAN_POINT('Ctrl Pts',(11.9285362396797,5.,72.8363283134386));
#38527=CARTESIAN_POINT('Ctrl Pts',(11.9647958564499,-5.,72.8120105983759));
#38528=CARTESIAN_POINT('Ctrl Pts',(11.9647958564499,5.,72.8120105983759));
#38529=CARTESIAN_POINT('Ctrl Pts',(12.0018563255875,-5.,72.7879907655145));
#38530=CARTESIAN_POINT('Ctrl Pts',(12.0018563255875,5.,72.7879907655145));
#38531=CARTESIAN_POINT('Ctrl Pts',(12.0397107079891,-5.,72.7642701618722));
#38532=CARTESIAN_POINT('Ctrl Pts',(12.0397107079891,5.,72.7642701618722));
#38533=CARTESIAN_POINT('Ctrl Pts',(12.0783501058978,-5.,72.7408481409417));
#38534=CARTESIAN_POINT('Ctrl Pts',(12.0783501058978,5.,72.7408481409417));
#38535=CARTESIAN_POINT('Ctrl Pts',(12.1177647907168,-5.,72.7177228241715));
#38536=CARTESIAN_POINT('Ctrl Pts',(12.1177647907168,5.,72.7177228241715));
#38537=CARTESIAN_POINT('Ctrl Pts',(12.1579454631339,-5.,72.6948917385186));
#38538=CARTESIAN_POINT('Ctrl Pts',(12.1579454631339,5.,72.6948917385186));
#38539=CARTESIAN_POINT('Ctrl Pts',(12.1906965354202,-5.,72.6768602906647));
#38540=CARTESIAN_POINT('Ctrl Pts',(12.1906965354202,5.,72.6768602906647));
#38541=CARTESIAN_POINT('Ctrl Pts',(12.2155986031066,-5.,72.6634671576927));
#38542=CARTESIAN_POINT('Ctrl Pts',(12.2155986031066,5.,72.6634671576927));
#38543=CARTESIAN_POINT('Ctrl Pts',(12.2323502706299,-5.,72.6545962765953));
#38544=CARTESIAN_POINT('Ctrl Pts',(12.2323502706299,5.,72.6545962765953));
#38545=CARTESIAN_POINT('Ctrl Pts',(12.2407636766788,-5.,72.6501753046048));
#38546=CARTESIAN_POINT('Ctrl Pts',(12.2407636766788,5.,72.6501753046048));
#38547=CARTESIAN_POINT('Ctrl Pts',(12.1362287539071,-4.8,72.7073228862334));
#38548=CARTESIAN_POINT('Ctrl Pts',(12.1362287539071,-3.13333333333333,72.7073228862334));
#38549=CARTESIAN_POINT('Ctrl Pts',(12.1362287539071,-1.46666666666667,72.7073228862334));
#38550=CARTESIAN_POINT('Ctrl Pts',(12.1362287539071,1.73333333333333,72.7073228862334));
#38551=CARTESIAN_POINT('Ctrl Pts',(12.1362287539072,3.26666666666667,72.7073228862334));
#38552=CARTESIAN_POINT('Ctrl Pts',(12.1362287539072,4.8,72.7073228862334));
#38553=CARTESIAN_POINT('',(11.3900156701126,0.,73.3715593562453));
#38554=CARTESIAN_POINT('Origin',(11.2668331993474,0.,73.7817890249619));
#38555=CARTESIAN_POINT('Ctrl Pts',(6.37923632332121,-5.,72.6501753046048));
#38556=CARTESIAN_POINT('Ctrl Pts',(6.37923632332121,5.,72.6501753046048));
#38557=CARTESIAN_POINT('Ctrl Pts',(6.38764972936496,-5.,72.6545962765957));
#38558=CARTESIAN_POINT('Ctrl Pts',(6.38764972936496,5.,72.6545962765957));
#38559=CARTESIAN_POINT('Ctrl Pts',(6.40440139687937,-5.,72.6634671576939));
#38560=CARTESIAN_POINT('Ctrl Pts',(6.40440139687937,5.,72.6634671576939));
#38561=CARTESIAN_POINT('Ctrl Pts',(6.42930346455622,-5.,72.6768602906668));
#38562=CARTESIAN_POINT('Ctrl Pts',(6.42930346455622,5.,72.6768602906668));
#38563=CARTESIAN_POINT('Ctrl Pts',(6.462054536837,-5.,72.6948917385213));
#38564=CARTESIAN_POINT('Ctrl Pts',(6.462054536837,5.,72.6948917385213));
#38565=CARTESIAN_POINT('Ctrl Pts',(6.50223520925657,-5.,72.7177228241743));
#38566=CARTESIAN_POINT('Ctrl Pts',(6.50223520925657,5.,72.7177228241743));
#38567=CARTESIAN_POINT('Ctrl Pts',(6.54164989408384,-5.,72.7408481409439));
#38568=CARTESIAN_POINT('Ctrl Pts',(6.54164989408384,5.,72.7408481409439));
#38569=CARTESIAN_POINT('Ctrl Pts',(6.58028929200299,-5.,72.7642701618733));
#38570=CARTESIAN_POINT('Ctrl Pts',(6.58028929200299,5.,72.7642701618733));
#38571=CARTESIAN_POINT('Ctrl Pts',(6.61814367441384,-5.,72.7879907655144));
#38572=CARTESIAN_POINT('Ctrl Pts',(6.61814367441384,5.,72.7879907655144));
#38573=CARTESIAN_POINT('Ctrl Pts',(6.65520414355746,-5.,72.8120105983748));
#38574=CARTESIAN_POINT('Ctrl Pts',(6.65520414355746,5.,72.8120105983748));
#38575=CARTESIAN_POINT('Ctrl Pts',(6.6914637603298,-5.,72.8363283134371));
#38576=CARTESIAN_POINT('Ctrl Pts',(6.6914637603298,5.,72.8363283134371));
#38577=CARTESIAN_POINT('Ctrl Pts',(6.72691496206853,-5.,72.860938304909));
#38578=CARTESIAN_POINT('Ctrl Pts',(6.72691496206853,5.,72.860938304909));
#38579=CARTESIAN_POINT('Ctrl Pts',(6.76154742510752,-5.,72.8858286124932));
#38580=CARTESIAN_POINT('Ctrl Pts',(6.76154742510752,5.,72.8858286124932));
#38581=CARTESIAN_POINT('Ctrl Pts',(6.79534573172022,-5.,72.9109783548257));
#38582=CARTESIAN_POINT('Ctrl Pts',(6.79534573172022,5.,72.9109783548257));
#38583=CARTESIAN_POINT('Ctrl Pts',(6.82828768209052,-5.,72.9363559240551));
#38584=CARTESIAN_POINT('Ctrl Pts',(6.82828768209052,5.,72.9363559240551));
#38585=CARTESIAN_POINT('Ctrl Pts',(6.86034144534386,-5.,72.9619150372476));
#38586=CARTESIAN_POINT('Ctrl Pts',(6.86034144534386,5.,72.9619150372476));
#38587=CARTESIAN_POINT('Ctrl Pts',(6.89146708305094,-5.,72.9875977410796));
#38588=CARTESIAN_POINT('Ctrl Pts',(6.89146708305094,5.,72.9875977410796));
#38589=CARTESIAN_POINT('Ctrl Pts',(6.92162338094535,-5.,73.0133459331862));
#38590=CARTESIAN_POINT('Ctrl Pts',(6.92162338094535,5.,73.0133459331862));
#38591=CARTESIAN_POINT('Ctrl Pts',(6.95077372875798,-5.,73.0391110577085));
#38592=CARTESIAN_POINT('Ctrl Pts',(6.95077372875798,5.,73.0391110577085));
#38593=CARTESIAN_POINT('Ctrl Pts',(6.97889211664697,-5.,73.0648637698137));
#38594=CARTESIAN_POINT('Ctrl Pts',(6.97889211664697,5.,73.0648637698137));
#38595=CARTESIAN_POINT('Ctrl Pts',(7.0059705464117,-5.,73.0906056305525));
#38596=CARTESIAN_POINT('Ctrl Pts',(7.0059705464117,5.,73.0906056305525));
#38597=CARTESIAN_POINT('Ctrl Pts',(7.03202274889284,-5.,73.1163746069901));
#38598=CARTESIAN_POINT('Ctrl Pts',(7.03202274889284,5.,73.1163746069901));
#38599=CARTESIAN_POINT('Ctrl Pts',(7.05706240056292,-5.,73.1422092666518));
#38600=CARTESIAN_POINT('Ctrl Pts',(7.05706240056292,5.,73.1422092666518));
#38601=CARTESIAN_POINT('Ctrl Pts',(7.08108356350204,-5.,73.1681162673139));
#38602=CARTESIAN_POINT('Ctrl Pts',(7.08108356350204,5.,73.1681162673139));
#38603=CARTESIAN_POINT('Ctrl Pts',(7.10404181575629,-5.,73.1940387655049));
#38604=CARTESIAN_POINT('Ctrl Pts',(7.10404181575629,5.,73.1940387655049));
#38605=CARTESIAN_POINT('Ctrl Pts',(7.12583169477727,-5.,73.2198184457921));
#38606=CARTESIAN_POINT('Ctrl Pts',(7.12583169477727,5.,73.2198184457921));
#38607=CARTESIAN_POINT('Ctrl Pts',(7.14627565136417,-5.,73.2451763035882));
#38608=CARTESIAN_POINT('Ctrl Pts',(7.14627565136417,5.,73.2451763035882));
#38609=CARTESIAN_POINT('Ctrl Pts',(7.16516265783021,-5.,73.2697754609995));
#38610=CARTESIAN_POINT('Ctrl Pts',(7.16516265783021,5.,73.2697754609995));
#38611=CARTESIAN_POINT('Ctrl Pts',(7.18228134605072,-5.,73.2932744155726));
#38612=CARTESIAN_POINT('Ctrl Pts',(7.18228134605072,5.,73.2932744155726));
#38613=CARTESIAN_POINT('Ctrl Pts',(7.19745223709556,-5.,73.3153789921172));
#38614=CARTESIAN_POINT('Ctrl Pts',(7.19745223709556,5.,73.3153789921172));
#38615=CARTESIAN_POINT('Ctrl Pts',(7.21056916724262,-5.,73.3359079249202));
#38616=CARTESIAN_POINT('Ctrl Pts',(7.21056916724262,5.,73.3359079249202));
#38617=CARTESIAN_POINT('Ctrl Pts',(7.21938607633981,-5.,73.3510066360849));
#38618=CARTESIAN_POINT('Ctrl Pts',(7.21938607633981,5.,73.3510066360849));
#38619=CARTESIAN_POINT('Ctrl Pts',(7.22505249282115,-5.,73.3615759220285));
#38620=CARTESIAN_POINT('Ctrl Pts',(7.22505249282115,5.,73.3615759220285));
#38621=CARTESIAN_POINT('Ctrl Pts',(7.22841034559228,-5.,73.3682873424406));
#38622=CARTESIAN_POINT('Ctrl Pts',(7.22841034559228,5.,73.3682873424406));
#38623=CARTESIAN_POINT('Ctrl Pts',(7.22998432988738,-5.,73.3715593562453));
#38624=CARTESIAN_POINT('Ctrl Pts',(7.22998432988738,5.,73.3715593562453));
#38625=CARTESIAN_POINT('',(7.22998432988738,0.,73.3715593562453));
#38626=CARTESIAN_POINT('Ctrl Pts',(6.48377124607659,4.8,72.7073228862421));
#38627=CARTESIAN_POINT('Ctrl Pts',(6.48377124607659,3.13333333333333,72.7073228862421));
#38628=CARTESIAN_POINT('Ctrl Pts',(6.48377124607659,1.46666666666667,72.7073228862421));
#38629=CARTESIAN_POINT('Ctrl Pts',(6.48377124607659,-1.73333333333333,72.7073228862421));
#38630=CARTESIAN_POINT('Ctrl Pts',(6.48377124607658,-3.26666666666667,72.7073228862421));
#38631=CARTESIAN_POINT('Ctrl Pts',(6.48377124607658,-4.8,72.7073228862421));
#38632=CARTESIAN_POINT('Origin',(9.30999999999986,0.,77.9999999999997));
#38633=CARTESIAN_POINT('',(8.09760744867254,0.,73.5108347879048));
#38634=CARTESIAN_POINT('',(7.3531668006526,0.,73.7817890249619));
#38635=CARTESIAN_POINT('Origin',(7.22998432988738,0.,73.3715593562453));
#38636=CARTESIAN_POINT('Ctrl Pts',(7.92828014771504,-5.,73.1174004638434));
#38637=CARTESIAN_POINT('Ctrl Pts',(7.92828014771504,5.,73.1174004638434));
#38638=CARTESIAN_POINT('Ctrl Pts',(7.92738267970718,-5.,73.1138822182422));
#38639=CARTESIAN_POINT('Ctrl Pts',(7.92738267970718,5.,73.1138822182422));
#38640=CARTESIAN_POINT('Ctrl Pts',(7.92564092628179,-5.,73.1065825857644));
#38641=CARTESIAN_POINT('Ctrl Pts',(7.92564092628179,5.,73.1065825857644));
#38642=CARTESIAN_POINT('Ctrl Pts',(7.92318784709425,-5.,73.094843740687));
#38643=CARTESIAN_POINT('Ctrl Pts',(7.92318784709425,5.,73.094843740687));
#38644=CARTESIAN_POINT('Ctrl Pts',(7.92023672685439,-5.,73.0776100569793));
#38645=CARTESIAN_POINT('Ctrl Pts',(7.92023672685439,5.,73.0776100569793));
#38646=CARTESIAN_POINT('Ctrl Pts',(7.91708913465458,-5.,73.0534525819187));
#38647=CARTESIAN_POINT('Ctrl Pts',(7.91708913465458,5.,73.0534525819187));
#38648=CARTESIAN_POINT('Ctrl Pts',(7.91450216351248,-5.,73.0267678331104));
#38649=CARTESIAN_POINT('Ctrl Pts',(7.91450216351248,5.,73.0267678331104));
#38650=CARTESIAN_POINT('Ctrl Pts',(7.91251100265505,-5.,72.9977629088649));
#38651=CARTESIAN_POINT('Ctrl Pts',(7.91251100265505,5.,72.9977629088649));
#38652=CARTESIAN_POINT('Ctrl Pts',(7.91116725541302,-5.,72.9667785272839));
#38653=CARTESIAN_POINT('Ctrl Pts',(7.91116725541302,5.,72.9667785272839));
#38654=CARTESIAN_POINT('Ctrl Pts',(7.91052851795384,-5.,72.9342121592381));
#38655=CARTESIAN_POINT('Ctrl Pts',(7.91052851795384,5.,72.9342121592381));
#38656=CARTESIAN_POINT('Ctrl Pts',(7.91064967462551,-5.,72.9004575141517));
#38657=CARTESIAN_POINT('Ctrl Pts',(7.91064967462551,5.,72.9004575141517));
#38658=CARTESIAN_POINT('Ctrl Pts',(7.91157405553992,-5.,72.865842448368));
#38659=CARTESIAN_POINT('Ctrl Pts',(7.91157405553992,5.,72.865842448368));
#38660=CARTESIAN_POINT('Ctrl Pts',(7.91332263489659,-5.,72.8305560285648));
#38661=CARTESIAN_POINT('Ctrl Pts',(7.91332263489659,5.,72.8305560285648));
#38662=CARTESIAN_POINT('Ctrl Pts',(7.91589792178415,-5.,72.7946703532482));
#38663=CARTESIAN_POINT('Ctrl Pts',(7.91589792178415,5.,72.7946703532482));
#38664=CARTESIAN_POINT('Ctrl Pts',(7.91929108795688,-5.,72.7581841390853));
#38665=CARTESIAN_POINT('Ctrl Pts',(7.91929108795688,5.,72.7581841390853));
#38666=CARTESIAN_POINT('Ctrl Pts',(7.92348781947401,-5.,72.7210590505692));
#38667=CARTESIAN_POINT('Ctrl Pts',(7.92348781947401,5.,72.7210590505692));
#38668=CARTESIAN_POINT('Ctrl Pts',(7.92847423001087,-5.,72.6832571772255));
#38669=CARTESIAN_POINT('Ctrl Pts',(7.92847423001087,5.,72.6832571772255));
#38670=CARTESIAN_POINT('Ctrl Pts',(7.93424318916555,-5.,72.644782464365));
#38671=CARTESIAN_POINT('Ctrl Pts',(7.93424318916555,5.,72.644782464365));
#38672=CARTESIAN_POINT('Ctrl Pts',(7.94079363473673,-5.,72.605674110239));
#38673=CARTESIAN_POINT('Ctrl Pts',(7.94079363473673,5.,72.605674110239));
#38674=CARTESIAN_POINT('Ctrl Pts',(7.94812873273426,-5.,72.5659928434222));
#38675=CARTESIAN_POINT('Ctrl Pts',(7.94812873273426,5.,72.5659928434222));
#38676=CARTESIAN_POINT('Ctrl Pts',(7.95625425867768,-5.,72.525809664929));
#38677=CARTESIAN_POINT('Ctrl Pts',(7.95625425867768,5.,72.525809664929));
#38678=CARTESIAN_POINT('Ctrl Pts',(7.96517686963318,-5.,72.4851946415088));
#38679=CARTESIAN_POINT('Ctrl Pts',(7.96517686963318,5.,72.4851946415088));
#38680=CARTESIAN_POINT('Ctrl Pts',(7.97490193183421,-5.,72.4442036884359));
#38681=CARTESIAN_POINT('Ctrl Pts',(7.97490193183421,5.,72.4442036884359));
#38682=CARTESIAN_POINT('Ctrl Pts',(7.98543275637321,-5.,72.4028752884941));
#38683=CARTESIAN_POINT('Ctrl Pts',(7.98543275637321,5.,72.4028752884941));
#38684=CARTESIAN_POINT('Ctrl Pts',(7.99677095487184,-5.,72.3612353480572));
#38685=CARTESIAN_POINT('Ctrl Pts',(7.99677095487184,5.,72.3612353480572));
#38686=CARTESIAN_POINT('Ctrl Pts',(8.00891630687688,-5.,72.3192996651676));
#38687=CARTESIAN_POINT('Ctrl Pts',(8.00891630687688,5.,72.3192996651676));
#38688=CARTESIAN_POINT('Ctrl Pts',(8.0218666223877,-5.,72.2770773952963));
#38689=CARTESIAN_POINT('Ctrl Pts',(8.0218666223877,5.,72.2770773952963));
#38690=CARTESIAN_POINT('Ctrl Pts',(8.03561745158717,-5.,72.2345740306898));
#38691=CARTESIAN_POINT('Ctrl Pts',(8.03561745158717,5.,72.2345740306898));
#38692=CARTESIAN_POINT('Ctrl Pts',(8.05016156282452,-5.,72.1917947954671));
#38693=CARTESIAN_POINT('Ctrl Pts',(8.05016156282452,5.,72.1917947954671));
#38694=CARTESIAN_POINT('Ctrl Pts',(8.06549029604253,-5.,72.1487445040024));
#38695=CARTESIAN_POINT('Ctrl Pts',(8.06549029604253,5.,72.1487445040024));
#38696=CARTESIAN_POINT('Ctrl Pts',(8.0815949379022,-5.,72.1054272393244));
#38697=CARTESIAN_POINT('Ctrl Pts',(8.0815949379022,5.,72.1054272393244));
#38698=CARTESIAN_POINT('Ctrl Pts',(8.09509332355121,-5.,72.0705623654361));
#38699=CARTESIAN_POINT('Ctrl Pts',(8.09509332355121,5.,72.0705623654361));
#38700=CARTESIAN_POINT('Ctrl Pts',(8.10556047416611,-5.,72.0442958898015));
#38701=CARTESIAN_POINT('Ctrl Pts',(8.10556047416611,5.,72.0442958898015));
#38702=CARTESIAN_POINT('Ctrl Pts',(8.11269090350187,-5.,72.0267326363232));
#38703=CARTESIAN_POINT('Ctrl Pts',(8.11269090350187,5.,72.0267326363232));
#38704=CARTESIAN_POINT('Ctrl Pts',(8.11629420041963,-5.,72.0179379421433));
#38705=CARTESIAN_POINT('Ctrl Pts',(8.11629420041963,5.,72.0179379421433));
#38706=CARTESIAN_POINT('Ctrl Pts',(8.07294956118024,-4.8,72.1289092826106));
#38707=CARTESIAN_POINT('Ctrl Pts',(8.07294956118024,-3.13333333333333,72.1289092826106));
#38708=CARTESIAN_POINT('Ctrl Pts',(8.07294956118024,-1.46666666666667,72.1289092826106));
#38709=CARTESIAN_POINT('Ctrl Pts',(8.07294956118024,1.73333333333333,72.1289092826106));
#38710=CARTESIAN_POINT('Ctrl Pts',(8.07294956118024,3.26666666666667,72.1289092826106));
#38711=CARTESIAN_POINT('Ctrl Pts',(8.07294956118024,4.8,72.1289092826106));
#38712=CARTESIAN_POINT('',(7.92828014771504,0.,73.1174004638434));
#38713=CARTESIAN_POINT('Origin',(8.09760744867254,0.,73.5108347879048));
#38714=CARTESIAN_POINT('Ctrl Pts',(3.62610374319018,-5.,75.7856550987203));
#38715=CARTESIAN_POINT('Ctrl Pts',(3.62610374319018,5.,75.7856550987203));
#38716=CARTESIAN_POINT('Ctrl Pts',(3.63539053217141,-5.,75.7836337265843));
#38717=CARTESIAN_POINT('Ctrl Pts',(3.63539053217141,5.,75.7836337265843));
#38718=CARTESIAN_POINT('Ctrl Pts',(3.65392514646738,-5.,75.7796614514307));
#38719=CARTESIAN_POINT('Ctrl Pts',(3.65392514646738,5.,75.7796614514307));
#38720=CARTESIAN_POINT('Ctrl Pts',(3.68161017699202,-5.,75.7739144459574));
#38721=CARTESIAN_POINT('Ctrl Pts',(3.68161017699202,5.,75.7739144459574));
#38722=CARTESIAN_POINT('Ctrl Pts',(3.71828934520109,-5.,75.7666753529192));
#38723=CARTESIAN_POINT('Ctrl Pts',(3.71828934520109,5.,75.7666753529192));
#38724=CARTESIAN_POINT('Ctrl Pts',(3.76374506499515,-5.,75.7583373408352));
#38725=CARTESIAN_POINT('Ctrl Pts',(3.76374506499515,5.,75.7583373408352));
#38726=CARTESIAN_POINT('Ctrl Pts',(3.80880313234912,-5.,75.7507170901994));
#38727=CARTESIAN_POINT('Ctrl Pts',(3.80880313234912,5.,75.7507170901994));
#38728=CARTESIAN_POINT('Ctrl Pts',(3.85345801322648,-5.,75.7438224729561));
#38729=CARTESIAN_POINT('Ctrl Pts',(3.85345801322648,5.,75.7438224729561));
#38730=CARTESIAN_POINT('Ctrl Pts',(3.89770346260673,-5.,75.7376611815813));
#38731=CARTESIAN_POINT('Ctrl Pts',(3.89770346260673,5.,75.7376611815813));
#38732=CARTESIAN_POINT('Ctrl Pts',(3.94153307998487,-5.,75.7322394306968));
#38733=CARTESIAN_POINT('Ctrl Pts',(3.94153307998487,5.,75.7322394306968));
#38734=CARTESIAN_POINT('Ctrl Pts',(3.98494068385426,-5.,75.7275606487971));
#38735=CARTESIAN_POINT('Ctrl Pts',(3.98494068385426,5.,75.7275606487971));
#38736=CARTESIAN_POINT('Ctrl Pts',(4.02791687754424,-5.,75.7236254027825));
#38737=CARTESIAN_POINT('Ctrl Pts',(4.02791687754424,5.,75.7236254027825));
#38738=CARTESIAN_POINT('Ctrl Pts',(4.07044606473286,-5.,75.7204311664588));
#38739=CARTESIAN_POINT('Ctrl Pts',(4.07044606473286,5.,75.7204311664588));
#38740=CARTESIAN_POINT('Ctrl Pts',(4.11250301246975,-5.,75.7179718540979));
#38741=CARTESIAN_POINT('Ctrl Pts',(4.11250301246975,5.,75.7179718540979));
#38742=CARTESIAN_POINT('Ctrl Pts',(4.1540503975699,-5.,75.7162375224483));
#38743=CARTESIAN_POINT('Ctrl Pts',(4.1540503975699,5.,75.7162375224483));
#38744=CARTESIAN_POINT('Ctrl Pts',(4.19503408607005,-5.,75.7152131772181));
#38745=CARTESIAN_POINT('Ctrl Pts',(4.19503408607005,5.,75.7152131772181));
#38746=CARTESIAN_POINT('Ctrl Pts',(4.23538623168054,-5.,75.7148800955126));
#38747=CARTESIAN_POINT('Ctrl Pts',(4.23538623168054,5.,75.7148800955126));
#38748=CARTESIAN_POINT('Ctrl Pts',(4.27503791496266,-5.,75.7152202603568));
#38749=CARTESIAN_POINT('Ctrl Pts',(4.27503791496266,5.,75.7152202603568));
#38750=CARTESIAN_POINT('Ctrl Pts',(4.31392987972073,-5.,75.7162200084309));
#38751=CARTESIAN_POINT('Ctrl Pts',(4.31392987972073,5.,75.7162200084309));
#38752=CARTESIAN_POINT('Ctrl Pts',(4.35202333876694,-5.,75.7178735790926));
#38753=CARTESIAN_POINT('Ctrl Pts',(4.35202333876694,5.,75.7178735790926));
#38754=CARTESIAN_POINT('Ctrl Pts',(4.38931316854928,-5.,75.7201873093206));
#38755=CARTESIAN_POINT('Ctrl Pts',(4.38931316854928,5.,75.7201873093206));
#38756=CARTESIAN_POINT('Ctrl Pts',(4.4258342922605,-5.,75.7231814575618));
#38757=CARTESIAN_POINT('Ctrl Pts',(4.4258342922605,5.,75.7231814575618));
#38758=CARTESIAN_POINT('Ctrl Pts',(4.46162197741249,-5.,75.7268767771899));
#38759=CARTESIAN_POINT('Ctrl Pts',(4.46162197741249,5.,75.7268767771899));
#38760=CARTESIAN_POINT('Ctrl Pts',(4.49667595482926,-5.,75.7312821851802));
#38761=CARTESIAN_POINT('Ctrl Pts',(4.49667595482926,5.,75.7312821851802));
#38762=CARTESIAN_POINT('Ctrl Pts',(4.53092565703999,-5.,75.7363826907893));
#38763=CARTESIAN_POINT('Ctrl Pts',(4.53092565703999,5.,75.7363826907893));
#38764=CARTESIAN_POINT('Ctrl Pts',(4.56418853184706,-5.,75.7421248073767));
#38765=CARTESIAN_POINT('Ctrl Pts',(4.56418853184706,5.,75.7421248073767));
#38766=CARTESIAN_POINT('Ctrl Pts',(4.59614922798229,-5.,75.7484089314505));
#38767=CARTESIAN_POINT('Ctrl Pts',(4.59614922798229,5.,75.7484089314505));
#38768=CARTESIAN_POINT('Ctrl Pts',(4.62642954792518,-5.,75.7551126455498));
#38769=CARTESIAN_POINT('Ctrl Pts',(4.62642954792518,5.,75.7551126455498));
#38770=CARTESIAN_POINT('Ctrl Pts',(4.6546480607543,-5.,75.7621102084272));
#38771=CARTESIAN_POINT('Ctrl Pts',(4.6546480607543,5.,75.7621102084272));
#38772=CARTESIAN_POINT('Ctrl Pts',(4.68047818546433,-5.,75.7692916356471));
#38773=CARTESIAN_POINT('Ctrl Pts',(4.68047818546433,5.,75.7692916356471));
#38774=CARTESIAN_POINT('Ctrl Pts',(4.70372208056759,-5.,75.7765863103517));
#38775=CARTESIAN_POINT('Ctrl Pts',(4.70372208056759,5.,75.7765863103517));
#38776=CARTESIAN_POINT('Ctrl Pts',(4.72018148924664,-5.,75.7824851942125));
#38777=CARTESIAN_POINT('Ctrl Pts',(4.72018148924664,5.,75.7824851942125));
#38778=CARTESIAN_POINT('Ctrl Pts',(4.73131602214788,-5.,75.7869394346818));
#38779=CARTESIAN_POINT('Ctrl Pts',(4.73131602214788,5.,75.7869394346818));
#38780=CARTESIAN_POINT('Ctrl Pts',(4.73820230448285,-5.,75.7899222948501));
#38781=CARTESIAN_POINT('Ctrl Pts',(4.73820230448285,5.,75.7899222948501));
#38782=CARTESIAN_POINT('Ctrl Pts',(4.7415112563347,-5.,75.7914170652479));
#38783=CARTESIAN_POINT('Ctrl Pts',(4.7415112563347,5.,75.7914170652479));
#38784=CARTESIAN_POINT('',(4.7415112563347,0.,75.7914170652479));
#38785=CARTESIAN_POINT('Ctrl Pts',(3.74291589727827,4.8,75.7622389329459));
#38786=CARTESIAN_POINT('Ctrl Pts',(3.74291589727827,3.13333333333333,75.7622389329459));
#38787=CARTESIAN_POINT('Ctrl Pts',(3.74291589727827,1.46666666666667,75.7622389329459));
#38788=CARTESIAN_POINT('Ctrl Pts',(3.74291589727827,-1.73333333333333,75.7622389329459));
#38789=CARTESIAN_POINT('Ctrl Pts',(3.74291589727829,-3.26666666666667,75.7622389329459));
#38790=CARTESIAN_POINT('Ctrl Pts',(3.74291589727829,-4.8,75.7622389329459));
#38791=CARTESIAN_POINT('Origin',(9.30999999999911,0.,77.9999999999995));
#38792=CARTESIAN_POINT('',(5.49567364700612,0.,75.340410845101));
#38793=CARTESIAN_POINT('',(5.09956505173093,0.,76.0264910574324));
#38794=CARTESIAN_POINT('Origin',(4.7415112563347,0.,75.7914170652479));
#38795=CARTESIAN_POINT('Ctrl Pts',(5.11306670030725,-5.,75.1478641584586));
#38796=CARTESIAN_POINT('Ctrl Pts',(5.11306670030725,5.,75.1478641584586));
#38797=CARTESIAN_POINT('Ctrl Pts',(5.11011771525268,-5.,75.1457459072827));
#38798=CARTESIAN_POINT('Ctrl Pts',(5.11011771525268,5.,75.1457459072827));
#38799=CARTESIAN_POINT('Ctrl Pts',(5.10409134141779,-5.,75.1412736419087));
#38800=CARTESIAN_POINT('Ctrl Pts',(5.10409134141779,5.,75.1412736419087));
#38801=CARTESIAN_POINT('Ctrl Pts',(5.09466658957769,-5.,75.1338579737766));
#38802=CARTESIAN_POINT('Ctrl Pts',(5.09466658957769,5.,75.1338579737766));
#38803=CARTESIAN_POINT('Ctrl Pts',(5.08132830195882,-5.,75.1225531496621));
#38804=CARTESIAN_POINT('Ctrl Pts',(5.08132830195882,5.,75.1225531496621));
#38805=CARTESIAN_POINT('Ctrl Pts',(5.06338898078153,-5.,75.1060706833968));
#38806=CARTESIAN_POINT('Ctrl Pts',(5.06338898078153,5.,75.1060706833968));
#38807=CARTESIAN_POINT('Ctrl Pts',(5.04425461999816,-5.,75.0872918528516));
#38808=CARTESIAN_POINT('Ctrl Pts',(5.04425461999816,5.,75.0872918528516));
#38809=CARTESIAN_POINT('Ctrl Pts',(5.02408529635579,-5.,75.0663526853382));
#38810=CARTESIAN_POINT('Ctrl Pts',(5.02408529635579,5.,75.0663526853382));
#38811=CARTESIAN_POINT('Ctrl Pts',(5.0031395496744,-5.,75.0434810160829));
#38812=CARTESIAN_POINT('Ctrl Pts',(5.0031395496744,5.,75.0434810160829));
#38813=CARTESIAN_POINT('Ctrl Pts',(4.98171699052613,-5.,75.0189443033335));
#38814=CARTESIAN_POINT('Ctrl Pts',(4.98171699052613,5.,75.0189443033335));
#38815=CARTESIAN_POINT('Ctrl Pts',(4.96011273429656,-5.,74.9930088670284));
#38816=CARTESIAN_POINT('Ctrl Pts',(4.96011273429656,5.,74.9930088670284));
#38817=CARTESIAN_POINT('Ctrl Pts',(4.93857071576856,-5.,74.9658980076381));
#38818=CARTESIAN_POINT('Ctrl Pts',(4.93857071576856,5.,74.9658980076381));
#38819=CARTESIAN_POINT('Ctrl Pts',(4.9172285318284,-5.,74.9377430766853));
#38820=CARTESIAN_POINT('Ctrl Pts',(4.9172285318284,5.,74.9377430766853));
#38821=CARTESIAN_POINT('Ctrl Pts',(4.89613444857711,-5.,74.9085976920187));
#38822=CARTESIAN_POINT('Ctrl Pts',(4.89613444857711,5.,74.9085976920187));
#38823=CARTESIAN_POINT('Ctrl Pts',(4.87528087827799,-5.,74.8784665452354));
#38824=CARTESIAN_POINT('Ctrl Pts',(4.87528087827799,5.,74.8784665452354));
#38825=CARTESIAN_POINT('Ctrl Pts',(4.85463221422931,-5.,74.847329470457));
#38826=CARTESIAN_POINT('Ctrl Pts',(4.85463221422931,5.,74.847329470457));
#38827=CARTESIAN_POINT('Ctrl Pts',(4.8341534505069,-5.,74.8151663525323));
#38828=CARTESIAN_POINT('Ctrl Pts',(4.8341534505069,5.,74.8151663525323));
#38829=CARTESIAN_POINT('Ctrl Pts',(4.81384166090143,-5.,74.7819847970791));
#38830=CARTESIAN_POINT('Ctrl Pts',(4.81384166090143,5.,74.7819847970791));
#38831=CARTESIAN_POINT('Ctrl Pts',(4.79372122786737,-5.,74.7478155144698));
#38832=CARTESIAN_POINT('Ctrl Pts',(4.79372122786737,5.,74.7478155144698));
#38833=CARTESIAN_POINT('Ctrl Pts',(4.77383361228174,-5.,74.7127029904203));
#38834=CARTESIAN_POINT('Ctrl Pts',(4.77383361228174,5.,74.7127029904203));
#38835=CARTESIAN_POINT('Ctrl Pts',(4.75422887701992,-5.,74.6766979024307));
#38836=CARTESIAN_POINT('Ctrl Pts',(4.75422887701992,5.,74.6766979024307));
#38837=CARTESIAN_POINT('Ctrl Pts',(4.7349571597282,-5.,74.6398496456652));
#38838=CARTESIAN_POINT('Ctrl Pts',(4.7349571597282,5.,74.6398496456652));
#38839=CARTESIAN_POINT('Ctrl Pts',(4.7160585128285,-5.,74.6021976043606));
#38840=CARTESIAN_POINT('Ctrl Pts',(4.7160585128285,5.,74.6021976043606));
#38841=CARTESIAN_POINT('Ctrl Pts',(4.69756020902596,-5.,74.5637691297098));
#38842=CARTESIAN_POINT('Ctrl Pts',(4.69756020902596,5.,74.5637691297098));
#38843=CARTESIAN_POINT('Ctrl Pts',(4.67948013519603,-5.,74.5245830312156));
#38844=CARTESIAN_POINT('Ctrl Pts',(4.67948013519603,5.,74.5245830312156));
#38845=CARTESIAN_POINT('Ctrl Pts',(4.66182827725193,-5.,74.4846515525847));
#38846=CARTESIAN_POINT('Ctrl Pts',(4.66182827725193,5.,74.4846515525847));
#38847=CARTESIAN_POINT('Ctrl Pts',(4.64460884258076,-5.,74.4439831150201));
#38848=CARTESIAN_POINT('Ctrl Pts',(4.64460884258076,5.,74.4439831150201));
#38849=CARTESIAN_POINT('Ctrl Pts',(4.62782195277069,-5.,74.402584786114));
#38850=CARTESIAN_POINT('Ctrl Pts',(4.62782195277069,5.,74.402584786114));
#38851=CARTESIAN_POINT('Ctrl Pts',(4.611465426047,-5.,74.3604652161898));
#38852=CARTESIAN_POINT('Ctrl Pts',(4.611465426047,5.,74.3604652161898));
#38853=CARTESIAN_POINT('Ctrl Pts',(4.59553572302984,-5.,74.3176336598508));
#38854=CARTESIAN_POINT('Ctrl Pts',(4.59553572302984,5.,74.3176336598508));
#38855=CARTESIAN_POINT('Ctrl Pts',(4.58002879342221,-5.,74.2740988457063));
#38856=CARTESIAN_POINT('Ctrl Pts',(4.58002879342221,5.,74.2740988457063));
#38857=CARTESIAN_POINT('Ctrl Pts',(4.5679584477719,-5.,74.2387142077601));
#38858=CARTESIAN_POINT('Ctrl Pts',(4.5679584477719,5.,74.2387142077601));
#38859=CARTESIAN_POINT('Ctrl Pts',(4.55909298521491,-5.,74.2118647653393));
#38860=CARTESIAN_POINT('Ctrl Pts',(4.55909298521491,5.,74.2118647653393));
#38861=CARTESIAN_POINT('Ctrl Pts',(4.55326576923269,-5.,74.1938271809836));
#38862=CARTESIAN_POINT('Ctrl Pts',(4.55326576923269,5.,74.1938271809836));
#38863=CARTESIAN_POINT('Ctrl Pts',(4.55037293434634,-5.,74.1847738997673));
#38864=CARTESIAN_POINT('Ctrl Pts',(4.55037293434634,5.,74.1847738997673));
#38865=CARTESIAN_POINT('Ctrl Pts',(4.58850001706627,-4.8,74.2976442754434));
#38866=CARTESIAN_POINT('Ctrl Pts',(4.58850001706627,-3.13333333333333,74.2976442754434));
#38867=CARTESIAN_POINT('Ctrl Pts',(4.58850001706627,-1.46666666666667,74.2976442754434));
#38868=CARTESIAN_POINT('Ctrl Pts',(4.58850001706627,1.73333333333333,74.2976442754434));
#38869=CARTESIAN_POINT('Ctrl Pts',(4.58850001706627,3.26666666666667,74.2976442754434));
#38870=CARTESIAN_POINT('Ctrl Pts',(4.58850001706627,4.8,74.2976442754434));
#38871=CARTESIAN_POINT('',(5.11306670030725,0.,75.1478641584586));
#38872=CARTESIAN_POINT('Origin',(5.49567364700612,0.,75.340410845101));
#38873=CARTESIAN_POINT('Ctrl Pts',(4.7262351906713,-5.,73.9751894239903));
#38874=CARTESIAN_POINT('Ctrl Pts',(4.7262351906713,5.,73.9751894239903));
#38875=CARTESIAN_POINT('Ctrl Pts',(4.73565326772794,-5.,73.9764662244033));
#38876=CARTESIAN_POINT('Ctrl Pts',(4.73565326772794,5.,73.9764662244033));
#38877=CARTESIAN_POINT('Ctrl Pts',(4.75442870611518,-5.,73.9790727181826));
#38878=CARTESIAN_POINT('Ctrl Pts',(4.75442870611518,5.,73.9790727181826));
#38879=CARTESIAN_POINT('Ctrl Pts',(4.78240971662693,-5.,73.9831411376458));
#38880=CARTESIAN_POINT('Ctrl Pts',(4.78240971662693,5.,73.9831411376458));
#38881=CARTESIAN_POINT('Ctrl Pts',(4.81935277595994,-5.,73.9888836296986));
#38882=CARTESIAN_POINT('Ctrl Pts',(4.81935277595994,5.,73.9888836296986));
#38883=CARTESIAN_POINT('Ctrl Pts',(4.86491894851451,-5.,73.9965952330726));
#38884=CARTESIAN_POINT('Ctrl Pts',(4.86491894851451,5.,73.9965952330726));
#38885=CARTESIAN_POINT('Ctrl Pts',(4.90986596114075,-5.,74.0048453064445));
#38886=CARTESIAN_POINT('Ctrl Pts',(4.90986596114075,5.,74.0048453064445));
#38887=CARTESIAN_POINT('Ctrl Pts',(4.95418592117643,-5.,74.0136393542666));
#38888=CARTESIAN_POINT('Ctrl Pts',(4.95418592117643,5.,74.0136393542666));
#38889=CARTESIAN_POINT('Ctrl Pts',(4.99787032923525,-5.,74.0229824691756));
#38890=CARTESIAN_POINT('Ctrl Pts',(4.99787032923525,5.,74.0229824691756));
#38891=CARTESIAN_POINT('Ctrl Pts',(5.04091104528079,-5.,74.0328783019017));
#38892=CARTESIAN_POINT('Ctrl Pts',(5.04091104528079,5.,74.0328783019017));
#38893=CARTESIAN_POINT('Ctrl Pts',(5.08330108798191,-5.,74.0433279599757));
#38894=CARTESIAN_POINT('Ctrl Pts',(5.08330108798191,5.,74.0433279599757));
#38895=CARTESIAN_POINT('Ctrl Pts',(5.12503143346602,-5.,74.0543287622593));
#38896=CARTESIAN_POINT('Ctrl Pts',(5.12503143346602,5.,74.0543287622593));
#38897=CARTESIAN_POINT('Ctrl Pts',(5.16608828999564,-5.,74.0658730006512));
#38898=CARTESIAN_POINT('Ctrl Pts',(5.16608828999564,5.,74.0658730006512));
#38899=CARTESIAN_POINT('Ctrl Pts',(5.20645002779749,-5.,74.077946326262));
#38900=CARTESIAN_POINT('Ctrl Pts',(5.20645002779749,5.,74.077946326262));
#38901=CARTESIAN_POINT('Ctrl Pts',(5.24608497534436,-5.,74.0905266302121));
#38902=CARTESIAN_POINT('Ctrl Pts',(5.24608497534436,5.,74.0905266302121));
#38903=CARTESIAN_POINT('Ctrl Pts',(5.28494739170145,-5.,74.1035813075707));
#38904=CARTESIAN_POINT('Ctrl Pts',(5.28494739170145,5.,74.1035813075707));
#38905=CARTESIAN_POINT('Ctrl Pts',(5.32297992581768,-5.,74.1170695597742));
#38906=CARTESIAN_POINT('Ctrl Pts',(5.32297992581768,5.,74.1170695597742));
#38907=CARTESIAN_POINT('Ctrl Pts',(5.36012397677248,-5.,74.1309508845677));
#38908=CARTESIAN_POINT('Ctrl Pts',(5.36012397677248,5.,74.1309508845677));
#38909=CARTESIAN_POINT('Ctrl Pts',(5.39632853508533,-5.,74.145192175818));
#38910=CARTESIAN_POINT('Ctrl Pts',(5.39632853508533,5.,74.145192175818));
#38911=CARTESIAN_POINT('Ctrl Pts',(5.43155912297689,-5.,74.1597747542928));
#38912=CARTESIAN_POINT('Ctrl Pts',(5.43155912297689,5.,74.1597747542928));
#38913=CARTESIAN_POINT('Ctrl Pts',(5.46580875850843,-5.,74.1747028224456));
#38914=CARTESIAN_POINT('Ctrl Pts',(5.46580875850843,5.,74.1747028224456));
#38915=CARTESIAN_POINT('Ctrl Pts',(5.49910332995037,-5.,74.1900073614232));
#38916=CARTESIAN_POINT('Ctrl Pts',(5.49910332995037,5.,74.1900073614232));
#38917=CARTESIAN_POINT('Ctrl Pts',(5.53146887985283,-5.,74.2057199352147));
#38918=CARTESIAN_POINT('Ctrl Pts',(5.53146887985283,5.,74.2057199352147));
#38919=CARTESIAN_POINT('Ctrl Pts',(5.5629021054891,-5.,74.2218488309718));
#38920=CARTESIAN_POINT('Ctrl Pts',(5.5629021054891,5.,74.2218488309718));
#38921=CARTESIAN_POINT('Ctrl Pts',(5.59334182226426,-5.,74.2383558265072));
#38922=CARTESIAN_POINT('Ctrl Pts',(5.59334182226426,5.,74.2383558265072));
#38923=CARTESIAN_POINT('Ctrl Pts',(5.6226347807329,-5.,74.2551282242929));
#38924=CARTESIAN_POINT('Ctrl Pts',(5.6226347807329,5.,74.2551282242929));
#38925=CARTESIAN_POINT('Ctrl Pts',(5.65051871403349,-5.,74.2719645711806));
#38926=CARTESIAN_POINT('Ctrl Pts',(5.65051871403349,5.,74.2719645711806));
#38927=CARTESIAN_POINT('Ctrl Pts',(5.67668010198173,-5.,74.2886204812191));
#38928=CARTESIAN_POINT('Ctrl Pts',(5.67668010198173,5.,74.2886204812191));
#38929=CARTESIAN_POINT('Ctrl Pts',(5.70080352279343,-5.,74.3048473392295));
#38930=CARTESIAN_POINT('Ctrl Pts',(5.70080352279343,5.,74.3048473392295));
#38931=CARTESIAN_POINT('Ctrl Pts',(5.72261970760114,-5.,74.3204300963653));
#38932=CARTESIAN_POINT('Ctrl Pts',(5.72261970760114,5.,74.3204300963653));
#38933=CARTESIAN_POINT('Ctrl Pts',(5.74196689861132,-5.,74.335234728705));
#38934=CARTESIAN_POINT('Ctrl Pts',(5.74196689861132,5.,74.335234728705));
#38935=CARTESIAN_POINT('Ctrl Pts',(5.75541614638509,-5.,74.3464073156572));
#38936=CARTESIAN_POINT('Ctrl Pts',(5.75541614638509,5.,74.3464073156572));
#38937=CARTESIAN_POINT('Ctrl Pts',(5.76435574482978,-5.,74.3544011670878));
#38938=CARTESIAN_POINT('Ctrl Pts',(5.76435574482978,5.,74.3544011670878));
#38939=CARTESIAN_POINT('Ctrl Pts',(5.7698065352688,-5.,74.3595593860371));
#38940=CARTESIAN_POINT('Ctrl Pts',(5.7698065352688,5.,74.3595593860371));
#38941=CARTESIAN_POINT('Ctrl Pts',(5.77240469132477,-5.,74.3620957389297));
#38942=CARTESIAN_POINT('Ctrl Pts',(5.77240469132477,5.,74.3620957389297));
#38943=CARTESIAN_POINT('',(5.77240469132477,0.,74.3620957389297));
#38944=CARTESIAN_POINT('Ctrl Pts',(4.84401151027683,4.8,73.9931375354699));
#38945=CARTESIAN_POINT('Ctrl Pts',(4.84401151027683,3.13333333333333,73.9931375354699));
#38946=CARTESIAN_POINT('Ctrl Pts',(4.84401151027683,1.46666666666667,73.9931375354699));
#38947=CARTESIAN_POINT('Ctrl Pts',(4.84401151027683,-1.73333333333333,73.9931375354699));
#38948=CARTESIAN_POINT('Ctrl Pts',(4.84401151027683,-3.26666666666667,73.9931375354699));
#38949=CARTESIAN_POINT('Ctrl Pts',(4.84401151027683,-4.8,73.9931375354699));
#38950=CARTESIAN_POINT('Origin',(9.30999999999964,0.,77.9999999999996));
#38951=CARTESIAN_POINT('',(6.63533873676838,0.,74.1962272508773));
#38952=CARTESIAN_POINT('',(6.02846516020394,0.,74.7054546451438));
#38953=CARTESIAN_POINT('Origin',(5.77240469132477,0.,74.3620957389297));
#38954=CARTESIAN_POINT('Ctrl Pts',(6.34166065765632,-5.,73.8844332675354));
#38955=CARTESIAN_POINT('Ctrl Pts',(6.34166065765632,5.,73.8844332675354));
#38956=CARTESIAN_POINT('Ctrl Pts',(6.33961400273085,-5.,73.8814341502491));
#38957=CARTESIAN_POINT('Ctrl Pts',(6.33961400273085,5.,73.8814341502491));
#38958=CARTESIAN_POINT('Ctrl Pts',(6.33548066854957,-5.,73.8751704542422));
#38959=CARTESIAN_POINT('Ctrl Pts',(6.33548066854957,5.,73.8751704542422));
#38960=CARTESIAN_POINT('Ctrl Pts',(6.32916060666778,-5.,73.8649785506499));
#38961=CARTESIAN_POINT('Ctrl Pts',(6.32916060666778,5.,73.8649785506499));
#38962=CARTESIAN_POINT('Ctrl Pts',(6.32049319378265,-5.,73.8497935278061));
#38963=CARTESIAN_POINT('Ctrl Pts',(6.32049319378265,5.,73.8497935278061));
#38964=CARTESIAN_POINT('Ctrl Pts',(6.30927308152859,-5.,73.8281694666761));
#38965=CARTESIAN_POINT('Ctrl Pts',(6.30927308152859,5.,73.8281694666761));
#38966=CARTESIAN_POINT('Ctrl Pts',(6.2977154022156,-5.,73.8039788013597));
#38967=CARTESIAN_POINT('Ctrl Pts',(6.2977154022156,5.,73.8039788013597));
#38968=CARTESIAN_POINT('Ctrl Pts',(6.28592405469892,-5.,73.7774041051942));
#38969=CARTESIAN_POINT('Ctrl Pts',(6.28592405469892,5.,73.7774041051942));
#38970=CARTESIAN_POINT('Ctrl Pts',(6.27406406270235,-5.,73.7487478990875));
#38971=CARTESIAN_POINT('Ctrl Pts',(6.27406406270235,5.,73.7487478990875));
#38972=CARTESIAN_POINT('Ctrl Pts',(6.26232549196199,-5.,73.7183639844318));
#38973=CARTESIAN_POINT('Ctrl Pts',(6.26232549196199,5.,73.7183639844318));
#38974=CARTESIAN_POINT('Ctrl Pts',(6.2508945734459,-5.,73.6866035555112));
#38975=CARTESIAN_POINT('Ctrl Pts',(6.2508945734459,5.,73.6866035555112));
#38976=CARTESIAN_POINT('Ctrl Pts',(6.23992415761167,-5.,73.6537598767373));
#38977=CARTESIAN_POINT('Ctrl Pts',(6.23992415761167,5.,73.6537598767373));
#38978=CARTESIAN_POINT('Ctrl Pts',(6.22949861837158,-5.,73.6200034390727));
#38979=CARTESIAN_POINT('Ctrl Pts',(6.22949861837158,5.,73.6200034390727));
#38980=CARTESIAN_POINT('Ctrl Pts',(6.21964497263984,-5.,73.5854011347937));
#38981=CARTESIAN_POINT('Ctrl Pts',(6.21964497263984,5.,73.5854011347937));
#38982=CARTESIAN_POINT('Ctrl Pts',(6.21035448565475,-5.,73.5499547774018));
#38983=CARTESIAN_POINT('Ctrl Pts',(6.21035448565475,5.,73.5499547774018));
#38984=CARTESIAN_POINT('Ctrl Pts',(6.20160059519737,-5.,73.5136332389612));
#38985=CARTESIAN_POINT('Ctrl Pts',(6.20160059519737,5.,73.5136332389612));
#38986=CARTESIAN_POINT('Ctrl Pts',(6.19335728624555,-5.,73.4764056446824));
#38987=CARTESIAN_POINT('Ctrl Pts',(6.19335728624555,5.,73.4764056446824));
#38988=CARTESIAN_POINT('Ctrl Pts',(6.18561920778822,-5.,73.4382781406853));
#38989=CARTESIAN_POINT('Ctrl Pts',(6.18561920778822,5.,73.4382781406853));
#38990=CARTESIAN_POINT('Ctrl Pts',(6.17839876827287,-5.,73.3992879245705));
#38991=CARTESIAN_POINT('Ctrl Pts',(6.17839876827287,5.,73.3992879245705));
#38992=CARTESIAN_POINT('Ctrl Pts',(6.17171971316999,-5.,73.3594909796912));
#38993=CARTESIAN_POINT('Ctrl Pts',(6.17171971316999,5.,73.3594909796912));
#38994=CARTESIAN_POINT('Ctrl Pts',(6.16561175346892,-5.,73.3189520498319));
#38995=CARTESIAN_POINT('Ctrl Pts',(6.16561175346892,5.,73.3189520498319));
#38996=CARTESIAN_POINT('Ctrl Pts',(6.16010510900493,-5.,73.2777346993489));
#38997=CARTESIAN_POINT('Ctrl Pts',(6.16010510900493,5.,73.2777346993489));
#38998=CARTESIAN_POINT('Ctrl Pts',(6.15522394653979,-5.,73.235889636054));
#38999=CARTESIAN_POINT('Ctrl Pts',(6.15522394653979,5.,73.235889636054));
#39000=CARTESIAN_POINT('Ctrl Pts',(6.15098453937228,-5.,73.1934518894766));
#39001=CARTESIAN_POINT('Ctrl Pts',(6.15098453937228,5.,73.1934518894766));
#39002=CARTESIAN_POINT('Ctrl Pts',(6.14739726243605,-5.,73.1504452524406));
#39003=CARTESIAN_POINT('Ctrl Pts',(6.14739726243605,5.,73.1504452524406));
#39004=CARTESIAN_POINT('Ctrl Pts',(6.14446731182389,-5.,73.1068846456515));
#39005=CARTESIAN_POINT('Ctrl Pts',(6.14446731182389,5.,73.1068846456515));
#39006=CARTESIAN_POINT('Ctrl Pts',(6.14219576096471,-5.,73.0627794214626));
#39007=CARTESIAN_POINT('Ctrl Pts',(6.14219576096471,5.,73.0627794214626));
#39008=CARTESIAN_POINT('Ctrl Pts',(6.14058030685598,-5.,73.0181362628236));
#39009=CARTESIAN_POINT('Ctrl Pts',(6.14058030685598,5.,73.0181362628236));
#39010=CARTESIAN_POINT('Ctrl Pts',(6.13961594071856,-5.,72.9729625521674));
#39011=CARTESIAN_POINT('Ctrl Pts',(6.13961594071856,5.,72.9729625521674));
#39012=CARTESIAN_POINT('Ctrl Pts',(6.13929617136756,-5.,72.927265775435));
#39013=CARTESIAN_POINT('Ctrl Pts',(6.13929617136756,5.,72.927265775435));
#39014=CARTESIAN_POINT('Ctrl Pts',(6.13961420741408,-5.,72.8810527495506));
#39015=CARTESIAN_POINT('Ctrl Pts',(6.13961420741408,5.,72.8810527495506));
#39016=CARTESIAN_POINT('Ctrl Pts',(6.14037405162642,-5.,72.8436737650304));
#39017=CARTESIAN_POINT('Ctrl Pts',(6.14037405162642,5.,72.8436737650304));
#39018=CARTESIAN_POINT('Ctrl Pts',(6.14122629204115,-5.,72.815411375335));
#39019=CARTESIAN_POINT('Ctrl Pts',(6.14122629204115,5.,72.815411375335));
#39020=CARTESIAN_POINT('Ctrl Pts',(6.14191971738286,-5.,72.7964685651683));
#39021=CARTESIAN_POINT('Ctrl Pts',(6.14191971738286,5.,72.7964685651683));
#39022=CARTESIAN_POINT('Ctrl Pts',(6.14229774633381,-5.,72.7869718558099));
#39023=CARTESIAN_POINT('Ctrl Pts',(6.14229774633381,5.,72.7869718558099));
#39024=CARTESIAN_POINT('Ctrl Pts',(6.13952154251132,-4.8,72.9060755452598));
#39025=CARTESIAN_POINT('Ctrl Pts',(6.13952154251132,-3.13333333333333,72.9060755452598));
#39026=CARTESIAN_POINT('Ctrl Pts',(6.13952154251132,-1.46666666666667,72.9060755452598));
#39027=CARTESIAN_POINT('Ctrl Pts',(6.13952154251132,1.73333333333333,72.9060755452598));
#39028=CARTESIAN_POINT('Ctrl Pts',(6.13952154251132,3.26666666666667,72.9060755452598));
#39029=CARTESIAN_POINT('Ctrl Pts',(6.13952154251132,4.8,72.9060755452598));
#39030=CARTESIAN_POINT('',(6.34166065765632,0.,73.8844332675354));
#39031=CARTESIAN_POINT('Origin',(6.63533873676838,0.,74.1962272508773));
#39032=CARTESIAN_POINT('Ctrl Pts',(8.38573080884383,-5.,71.9704289984876));
#39033=CARTESIAN_POINT('Ctrl Pts',(8.38573080884383,5.,71.9704289984876));
#39034=CARTESIAN_POINT('Ctrl Pts',(8.39212476293556,-5.,71.9774609075814));
#39035=CARTESIAN_POINT('Ctrl Pts',(8.39212476293556,5.,71.9774609075814));
#39036=CARTESIAN_POINT('Ctrl Pts',(8.40483216124376,-5.,71.991526216807));
#39037=CARTESIAN_POINT('Ctrl Pts',(8.40483216124376,5.,71.991526216807));
#39038=CARTESIAN_POINT('Ctrl Pts',(8.42365172920544,-5.,72.0126286537798));
#39039=CARTESIAN_POINT('Ctrl Pts',(8.42365172920544,5.,72.0126286537798));
#39040=CARTESIAN_POINT('Ctrl Pts',(8.44826055176072,-5.,72.040774198702));
#39041=CARTESIAN_POINT('Ctrl Pts',(8.44826055176072,5.,72.040774198702));
#39042=CARTESIAN_POINT('Ctrl Pts',(8.47820934194863,-5.,72.0759710007559));
#39043=CARTESIAN_POINT('Ctrl Pts',(8.47820934194863,5.,72.0759710007559));
#39044=CARTESIAN_POINT('Ctrl Pts',(8.5073377062906,-5.,72.1111823064372));
#39045=CARTESIAN_POINT('Ctrl Pts',(8.5073377062906,5.,72.1111823064372));
#39046=CARTESIAN_POINT('Ctrl Pts',(8.5356360604508,-5.,72.1464072590907));
#39047=CARTESIAN_POINT('Ctrl Pts',(8.5356360604508,5.,72.1464072590907));
#39048=CARTESIAN_POINT('Ctrl Pts',(8.56309462002684,-5.,72.1816442965978));
#39049=CARTESIAN_POINT('Ctrl Pts',(8.56309462002684,5.,72.1816442965978));
#39050=CARTESIAN_POINT('Ctrl Pts',(8.58970480273757,-5.,72.2168909832624));
#39051=CARTESIAN_POINT('Ctrl Pts',(8.58970480273757,5.,72.2168909832624));
#39052=CARTESIAN_POINT('Ctrl Pts',(8.61546054866421,-5.,72.2521436799883));
#39053=CARTESIAN_POINT('Ctrl Pts',(8.61546054866421,5.,72.2521436799883));
#39054=CARTESIAN_POINT('Ctrl Pts',(8.6403566685235,-5.,72.2873945324713));
#39055=CARTESIAN_POINT('Ctrl Pts',(8.6403566685235,5.,72.2873945324713));
#39056=CARTESIAN_POINT('Ctrl Pts',(8.66438755190754,-5.,72.322628770807));
#39057=CARTESIAN_POINT('Ctrl Pts',(8.66438755190754,5.,72.322628770807));
#39058=CARTESIAN_POINT('Ctrl Pts',(8.68754585274241,-5.,72.3578214997599));
#39059=CARTESIAN_POINT('Ctrl Pts',(8.68754585274241,5.,72.3578214997599));
#39060=CARTESIAN_POINT('Ctrl Pts',(8.7098215205491,-5.,72.3929354248824));
#39061=CARTESIAN_POINT('Ctrl Pts',(8.7098215205491,5.,72.3929354248824));
#39062=CARTESIAN_POINT('Ctrl Pts',(8.73120047378673,-5.,72.4279161676434));
#39063=CARTESIAN_POINT('Ctrl Pts',(8.73120047378673,5.,72.4279161676434));
#39064=CARTESIAN_POINT('Ctrl Pts',(8.75166500381177,-5.,72.4626956099856));
#39065=CARTESIAN_POINT('Ctrl Pts',(8.75166500381177,5.,72.4626956099856));
#39066=CARTESIAN_POINT('Ctrl Pts',(8.77119625406051,-5.,72.4972050574356));
#39067=CARTESIAN_POINT('Ctrl Pts',(8.77119625406051,5.,72.4972050574356));
#39068=CARTESIAN_POINT('Ctrl Pts',(8.78977642921376,-5.,72.5313863609611));
#39069=CARTESIAN_POINT('Ctrl Pts',(8.78977642921376,5.,72.5313863609611));
#39070=CARTESIAN_POINT('Ctrl Pts',(8.80739112453777,-5.,72.5652030495491));
#39071=CARTESIAN_POINT('Ctrl Pts',(8.80739112453777,5.,72.5652030495491));
#39072=CARTESIAN_POINT('Ctrl Pts',(8.82403229027104,-5.,72.5986538545611));
#39073=CARTESIAN_POINT('Ctrl Pts',(8.82403229027104,5.,72.5986538545611));
#39074=CARTESIAN_POINT('Ctrl Pts',(8.83969984368247,-5.,72.6317791495918));
#39075=CARTESIAN_POINT('Ctrl Pts',(8.83969984368247,5.,72.6317791495918));
#39076=CARTESIAN_POINT('Ctrl Pts',(8.85439344558271,-5.,72.6646198538891));
#39077=CARTESIAN_POINT('Ctrl Pts',(8.85439344558271,5.,72.6646198538891));
#39078=CARTESIAN_POINT('Ctrl Pts',(8.86810523905958,-5.,72.697180192828));
#39079=CARTESIAN_POINT('Ctrl Pts',(8.86810523905958,5.,72.697180192828));
#39080=CARTESIAN_POINT('Ctrl Pts',(8.88081292274355,-5.,72.7293915578161));
#39081=CARTESIAN_POINT('Ctrl Pts',(8.88081292274355,5.,72.7293915578161));
#39082=CARTESIAN_POINT('Ctrl Pts',(8.892471541323,-5.,72.7610691106936));
#39083=CARTESIAN_POINT('Ctrl Pts',(8.892471541323,5.,72.7610691106936));
#39084=CARTESIAN_POINT('Ctrl Pts',(8.90300967831155,-5.,72.7918899475057));
#39085=CARTESIAN_POINT('Ctrl Pts',(8.90300967831155,5.,72.7918899475057));
#39086=CARTESIAN_POINT('Ctrl Pts',(8.91234425157306,-5.,72.8214653308615));
#39087=CARTESIAN_POINT('Ctrl Pts',(8.91234425157306,5.,72.8214653308615));
#39088=CARTESIAN_POINT('Ctrl Pts',(8.92039344075756,-5.,72.8494020612689));
#39089=CARTESIAN_POINT('Ctrl Pts',(8.92039344075756,5.,72.8494020612689));
#39090=CARTESIAN_POINT('Ctrl Pts',(8.92708920468011,-5.,72.875362319063));
#39091=CARTESIAN_POINT('Ctrl Pts',(8.92708920468011,5.,72.875362319063));
#39092=CARTESIAN_POINT('Ctrl Pts',(8.93239377860217,-5.,72.8991394600597));
#39093=CARTESIAN_POINT('Ctrl Pts',(8.93239377860217,5.,72.8991394600597));
#39094=CARTESIAN_POINT('Ctrl Pts',(8.93551489966184,-5.,72.9163431680377));
#39095=CARTESIAN_POINT('Ctrl Pts',(8.93551489966184,5.,72.9163431680377));
#39096=CARTESIAN_POINT('Ctrl Pts',(8.9372246807253,-5.,72.928213076623));
#39097=CARTESIAN_POINT('Ctrl Pts',(8.9372246807253,5.,72.928213076623));
#39098=CARTESIAN_POINT('Ctrl Pts',(8.93808458922835,-5.,72.9356682021451));
#39099=CARTESIAN_POINT('Ctrl Pts',(8.93808458922835,5.,72.9356682021451));
#39100=CARTESIAN_POINT('Ctrl Pts',(8.93844455602745,-5.,72.9392812237066));
#39101=CARTESIAN_POINT('Ctrl Pts',(8.93844455602745,5.,72.9392812237066));
#39102=CARTESIAN_POINT('',(8.93844455602745,0.,72.9392812237066));
#39103=CARTESIAN_POINT('Ctrl Pts',(8.46441588028027,4.8,72.0598832085154));
#39104=CARTESIAN_POINT('Ctrl Pts',(8.46441588028027,3.13333333333333,72.0598832085154));
#39105=CARTESIAN_POINT('Ctrl Pts',(8.46441588028027,1.46666666666667,72.0598832085154));
#39106=CARTESIAN_POINT('Ctrl Pts',(8.46441588028027,-1.73333333333333,72.0598832085154));
#39107=CARTESIAN_POINT('Ctrl Pts',(8.46441588028027,-3.26666666666667,72.0598832085153));
#39108=CARTESIAN_POINT('Ctrl Pts',(8.46441588028027,-4.8,72.0598832085153));
#39109=CARTESIAN_POINT('Origin',(9.31,0.,77.9999999999998));
#39110=CARTESIAN_POINT('',(9.70610859527519,0.,73.3669019025333));
#39111=CARTESIAN_POINT('',(8.91389140472481,0.,73.3669019025333));
#39112=CARTESIAN_POINT('Origin',(8.93844455602745,0.,72.9392812237066));
#39113=CARTESIAN_POINT('Ctrl Pts',(9.68155544397255,-5.,72.9392812237066));
#39114=CARTESIAN_POINT('Ctrl Pts',(9.68155544397255,5.,72.9392812237066));
#39115=CARTESIAN_POINT('Ctrl Pts',(9.6819154107701,-5.,72.9356682021447));
#39116=CARTESIAN_POINT('Ctrl Pts',(9.6819154107701,5.,72.9356682021447));
#39117=CARTESIAN_POINT('Ctrl Pts',(9.68277531927063,-5.,72.9282130766218));
#39118=CARTESIAN_POINT('Ctrl Pts',(9.68277531927063,5.,72.9282130766218));
#39119=CARTESIAN_POINT('Ctrl Pts',(9.68448510033203,-5.,72.9163431680359));
#39120=CARTESIAN_POINT('Ctrl Pts',(9.68448510033203,5.,72.9163431680359));
#39121=CARTESIAN_POINT('Ctrl Pts',(9.68760622139204,-5.,72.8991394600578));
#39122=CARTESIAN_POINT('Ctrl Pts',(9.68760622139204,5.,72.8991394600578));
#39123=CARTESIAN_POINT('Ctrl Pts',(9.69291079531749,-5.,72.875362319062));
#39124=CARTESIAN_POINT('Ctrl Pts',(9.69291079531749,5.,72.875362319062));
#39125=CARTESIAN_POINT('Ctrl Pts',(9.69960655924369,-5.,72.8494020612693));
#39126=CARTESIAN_POINT('Ctrl Pts',(9.69960655924369,5.,72.8494020612693));
#39127=CARTESIAN_POINT('Ctrl Pts',(9.70765574843018,-5.,72.8214653308631));
#39128=CARTESIAN_POINT('Ctrl Pts',(9.70765574843018,5.,72.8214653308631));
#39129=CARTESIAN_POINT('Ctrl Pts',(9.7169903216916,-5.,72.7918899475077));
#39130=CARTESIAN_POINT('Ctrl Pts',(9.7169903216916,5.,72.7918899475077));
#39131=CARTESIAN_POINT('Ctrl Pts',(9.72752845867869,-5.,72.7610691106953));
#39132=CARTESIAN_POINT('Ctrl Pts',(9.72752845867869,5.,72.7610691106953));
#39133=CARTESIAN_POINT('Ctrl Pts',(9.73918707725648,-5.,72.7293915578165));
#39134=CARTESIAN_POINT('Ctrl Pts',(9.73918707725648,5.,72.7293915578165));
#39135=CARTESIAN_POINT('Ctrl Pts',(9.75189476093958,-5.,72.6971801928267));
#39136=CARTESIAN_POINT('Ctrl Pts',(9.75189476093958,5.,72.6971801928267));
#39137=CARTESIAN_POINT('Ctrl Pts',(9.76560655441652,-5.,72.6646198538862));
#39138=CARTESIAN_POINT('Ctrl Pts',(9.76560655441652,5.,72.6646198538862));
#39139=CARTESIAN_POINT('Ctrl Pts',(9.78030015631738,-5.,72.6317791495885));
#39140=CARTESIAN_POINT('Ctrl Pts',(9.78030015631738,5.,72.6317791495885));
#39141=CARTESIAN_POINT('Ctrl Pts',(9.79596770972936,-5.,72.5986538545587));
#39142=CARTESIAN_POINT('Ctrl Pts',(9.79596770972936,5.,72.5986538545587));
#39143=CARTESIAN_POINT('Ctrl Pts',(9.81260887546254,-5.,72.5652030495487));
#39144=CARTESIAN_POINT('Ctrl Pts',(9.81260887546254,5.,72.5652030495487));
#39145=CARTESIAN_POINT('Ctrl Pts',(9.83022357078552,-5.,72.5313863609631));
#39146=CARTESIAN_POINT('Ctrl Pts',(9.83022357078552,5.,72.5313863609631));
#39147=CARTESIAN_POINT('Ctrl Pts',(9.84880374593723,-5.,72.4972050574394));
#39148=CARTESIAN_POINT('Ctrl Pts',(9.84880374593723,5.,72.4972050574394));
#39149=CARTESIAN_POINT('Ctrl Pts',(9.86833499618467,-5.,72.46269560999));
#39150=CARTESIAN_POINT('Ctrl Pts',(9.86833499618467,5.,72.46269560999));
#39151=CARTESIAN_POINT('Ctrl Pts',(9.88879952620961,-5.,72.4279161676469));
#39152=CARTESIAN_POINT('Ctrl Pts',(9.88879952620961,5.,72.4279161676469));
#39153=CARTESIAN_POINT('Ctrl Pts',(9.91017847944898,-5.,72.3929354248836));
#39154=CARTESIAN_POINT('Ctrl Pts',(9.91017847944898,5.,72.3929354248836));
#39155=CARTESIAN_POINT('Ctrl Pts',(9.9324541472595,-5.,72.3578214997584));
#39156=CARTESIAN_POINT('Ctrl Pts',(9.9324541472595,5.,72.3578214997584));
#39157=CARTESIAN_POINT('Ctrl Pts',(9.95561244809927,-5.,72.322628770803));
#39158=CARTESIAN_POINT('Ctrl Pts',(9.95561244809927,5.,72.322628770803));
#39159=CARTESIAN_POINT('Ctrl Pts',(9.97964333148752,-5.,72.2873945324658));
#39160=CARTESIAN_POINT('Ctrl Pts',(9.97964333148752,5.,72.2873945324658));
#39161=CARTESIAN_POINT('Ctrl Pts',(10.0045394513483,-5.,72.2521436799828));
#39162=CARTESIAN_POINT('Ctrl Pts',(10.0045394513483,5.,72.2521436799828));
#39163=CARTESIAN_POINT('Ctrl Pts',(10.0302951972721,-5.,72.2168909832587));
#39164=CARTESIAN_POINT('Ctrl Pts',(10.0302951972721,5.,72.2168909832587));
#39165=CARTESIAN_POINT('Ctrl Pts',(10.0569053799749,-5.,72.1816442965973));
#39166=CARTESIAN_POINT('Ctrl Pts',(10.0569053799749,5.,72.1816442965973));
#39167=CARTESIAN_POINT('Ctrl Pts',(10.0843639395388,-5.,72.1464072590943));
#39168=CARTESIAN_POINT('Ctrl Pts',(10.0843639395388,5.,72.1464072590943));
#39169=CARTESIAN_POINT('Ctrl Pts',(10.1126622936855,-5.,72.1111823064446));
#39170=CARTESIAN_POINT('Ctrl Pts',(10.1126622936855,5.,72.1111823064446));
#39171=CARTESIAN_POINT('Ctrl Pts',(10.1417906580168,-5.,72.0759710007657));
#39172=CARTESIAN_POINT('Ctrl Pts',(10.1417906580168,5.,72.0759710007657));
#39173=CARTESIAN_POINT('Ctrl Pts',(10.1717394482016,-5.,72.0407741987119));
#39174=CARTESIAN_POINT('Ctrl Pts',(10.1717394482016,5.,72.0407741987119));
#39175=CARTESIAN_POINT('Ctrl Pts',(10.1963482707641,-5.,72.0126286537873));
#39176=CARTESIAN_POINT('Ctrl Pts',(10.1963482707641,5.,72.0126286537873));
#39177=CARTESIAN_POINT('Ctrl Pts',(10.2151678387382,-5.,71.9915262168113));
#39178=CARTESIAN_POINT('Ctrl Pts',(10.2151678387382,5.,71.9915262168113));
#39179=CARTESIAN_POINT('Ctrl Pts',(10.2278752370579,-5.,71.9774609075829));
#39180=CARTESIAN_POINT('Ctrl Pts',(10.2278752370579,5.,71.9774609075829));
#39181=CARTESIAN_POINT('Ctrl Pts',(10.2342691911562,-5.,71.9704289984876));
#39182=CARTESIAN_POINT('Ctrl Pts',(10.2342691911562,5.,71.9704289984876));
#39183=CARTESIAN_POINT('Ctrl Pts',(10.1555841196958,-4.8,72.059883208512));
#39184=CARTESIAN_POINT('Ctrl Pts',(10.1555841196958,-3.13333333333333,72.059883208512));
#39185=CARTESIAN_POINT('Ctrl Pts',(10.1555841196958,-1.46666666666667,72.059883208512));
#39186=CARTESIAN_POINT('Ctrl Pts',(10.1555841196958,1.73333333333333,72.059883208512));
#39187=CARTESIAN_POINT('Ctrl Pts',(10.1555841196958,3.26666666666667,72.059883208512));
#39188=CARTESIAN_POINT('Ctrl Pts',(10.1555841196958,4.8,72.059883208512));
#39189=CARTESIAN_POINT('',(9.68155544397255,0.,72.9392812237066));
#39190=CARTESIAN_POINT('Origin',(9.70610859527519,0.,73.3669019025333));
#39191=CARTESIAN_POINT('Ctrl Pts',(12.4777022536662,-5.,72.7869718558099));
#39192=CARTESIAN_POINT('Ctrl Pts',(12.4777022536662,5.,72.7869718558099));
#39193=CARTESIAN_POINT('Ctrl Pts',(12.4780802826126,-5.,72.7964685651569));
#39194=CARTESIAN_POINT('Ctrl Pts',(12.4780802826126,5.,72.7964685651569));
#39195=CARTESIAN_POINT('Ctrl Pts',(12.4787737079463,-5.,72.8154113753035));
#39196=CARTESIAN_POINT('Ctrl Pts',(12.4787737079463,5.,72.8154113753035));
#39197=CARTESIAN_POINT('Ctrl Pts',(12.4796259483525,-5.,72.8436737649773));
#39198=CARTESIAN_POINT('Ctrl Pts',(12.4796259483525,5.,72.8436737649773));
#39199=CARTESIAN_POINT('Ctrl Pts',(12.4803857925599,-5.,72.8810527494849));
#39200=CARTESIAN_POINT('Ctrl Pts',(12.4803857925599,5.,72.8810527494849));
#39201=CARTESIAN_POINT('Ctrl Pts',(12.4807038286085,-5.,72.9272657753747));
#39202=CARTESIAN_POINT('Ctrl Pts',(12.4807038286085,5.,72.9272657753747));
#39203=CARTESIAN_POINT('Ctrl Pts',(12.4803840592649,-5.,72.9729625521258));
#39204=CARTESIAN_POINT('Ctrl Pts',(12.4803840592649,5.,72.9729625521258));
#39205=CARTESIAN_POINT('Ctrl Pts',(12.4794196931369,-5.,73.0181362628057));
#39206=CARTESIAN_POINT('Ctrl Pts',(12.4794196931369,5.,73.0181362628057));
#39207=CARTESIAN_POINT('Ctrl Pts',(12.4778042390365,-5.,73.0627794214657));
#39208=CARTESIAN_POINT('Ctrl Pts',(12.4778042390365,5.,73.0627794214657));
#39209=CARTESIAN_POINT('Ctrl Pts',(12.4755326881828,-5.,73.106884645668));
#39210=CARTESIAN_POINT('Ctrl Pts',(12.4755326881828,5.,73.106884645668));
#39211=CARTESIAN_POINT('Ctrl Pts',(12.4726027375726,-5.,73.1504452524619));
#39212=CARTESIAN_POINT('Ctrl Pts',(12.4726027375726,5.,73.1504452524619));
#39213=CARTESIAN_POINT('Ctrl Pts',(12.4690154606353,-5.,73.1934518894953));
#39214=CARTESIAN_POINT('Ctrl Pts',(12.4690154606353,5.,73.1934518894953));
#39215=CARTESIAN_POINT('Ctrl Pts',(12.4647760534649,-5.,73.2358896360656));
#39216=CARTESIAN_POINT('Ctrl Pts',(12.4647760534649,5.,73.2358896360656));
#39217=CARTESIAN_POINT('Ctrl Pts',(12.4598948909964,-5.,73.2777346993523));
#39218=CARTESIAN_POINT('Ctrl Pts',(12.4598948909964,5.,73.2777346993523));
#39219=CARTESIAN_POINT('Ctrl Pts',(12.4543882465297,-5.,73.3189520498286));
#39220=CARTESIAN_POINT('Ctrl Pts',(12.4543882465297,5.,73.3189520498286));
#39221=CARTESIAN_POINT('Ctrl Pts',(12.4482802868274,-5.,73.3594909796843));
#39222=CARTESIAN_POINT('Ctrl Pts',(12.4482802868274,5.,73.3594909796843));
#39223=CARTESIAN_POINT('Ctrl Pts',(12.4416012317246,-5.,73.3992879245629));
#39224=CARTESIAN_POINT('Ctrl Pts',(12.4416012317246,5.,73.3992879245629));
#39225=CARTESIAN_POINT('Ctrl Pts',(12.4343807922101,-5.,73.4382781406794));
#39226=CARTESIAN_POINT('Ctrl Pts',(12.4343807922101,5.,73.4382781406794));
#39227=CARTESIAN_POINT('Ctrl Pts',(12.4266427137538,-5.,73.4764056446796));
#39228=CARTESIAN_POINT('Ctrl Pts',(12.4266427137538,5.,73.4764056446796));
#39229=CARTESIAN_POINT('Ctrl Pts',(12.4183994048028,-5.,73.5136332389618));
#39230=CARTESIAN_POINT('Ctrl Pts',(12.4183994048028,5.,73.5136332389618));
#39231=CARTESIAN_POINT('Ctrl Pts',(12.4096455143457,-5.,73.5499547774051));
#39232=CARTESIAN_POINT('Ctrl Pts',(12.4096455143457,5.,73.5499547774051));
#39233=CARTESIAN_POINT('Ctrl Pts',(12.4003550273604,-5.,73.5854011347984));
#39234=CARTESIAN_POINT('Ctrl Pts',(12.4003550273604,5.,73.5854011347984));
#39235=CARTESIAN_POINT('Ctrl Pts',(12.3905013816283,-5.,73.6200034390768));
#39236=CARTESIAN_POINT('Ctrl Pts',(12.3905013816283,5.,73.6200034390768));
#39237=CARTESIAN_POINT('Ctrl Pts',(12.380075842388,-5.,73.6537598767393));
#39238=CARTESIAN_POINT('Ctrl Pts',(12.380075842388,5.,73.6537598767393));
#39239=CARTESIAN_POINT('Ctrl Pts',(12.3691054265541,-5.,73.6866035555106));
#39240=CARTESIAN_POINT('Ctrl Pts',(12.3691054265541,5.,73.6866035555106));
#39241=CARTESIAN_POINT('Ctrl Pts',(12.3576745080387,-5.,73.7183639844293));
#39242=CARTESIAN_POINT('Ctrl Pts',(12.3576745080387,5.,73.7183639844293));
#39243=CARTESIAN_POINT('Ctrl Pts',(12.3459359372991,-5.,73.7487478990847));
#39244=CARTESIAN_POINT('Ctrl Pts',(12.3459359372991,5.,73.7487478990847));
#39245=CARTESIAN_POINT('Ctrl Pts',(12.3340759453026,-5.,73.7774041051921));
#39246=CARTESIAN_POINT('Ctrl Pts',(12.3340759453026,5.,73.7774041051921));
#39247=CARTESIAN_POINT('Ctrl Pts',(12.322284597785,-5.,73.8039788013593));
#39248=CARTESIAN_POINT('Ctrl Pts',(12.322284597785,5.,73.8039788013593));
#39249=CARTESIAN_POINT('Ctrl Pts',(12.3107269184702,-5.,73.8281694666772));
#39250=CARTESIAN_POINT('Ctrl Pts',(12.3107269184702,5.,73.8281694666772));
#39251=CARTESIAN_POINT('Ctrl Pts',(12.2995068062144,-5.,73.8497935278081));
#39252=CARTESIAN_POINT('Ctrl Pts',(12.2995068062144,5.,73.8497935278081));
#39253=CARTESIAN_POINT('Ctrl Pts',(12.2908393933291,-5.,73.8649785506518));
#39254=CARTESIAN_POINT('Ctrl Pts',(12.2908393933291,5.,73.8649785506518));
#39255=CARTESIAN_POINT('Ctrl Pts',(12.2845193314483,-5.,73.8751704542434));
#39256=CARTESIAN_POINT('Ctrl Pts',(12.2845193314483,5.,73.8751704542434));
#39257=CARTESIAN_POINT('Ctrl Pts',(12.2803859972684,-5.,73.8814341502495));
#39258=CARTESIAN_POINT('Ctrl Pts',(12.2803859972684,5.,73.8814341502495));
#39259=CARTESIAN_POINT('Ctrl Pts',(12.2783393423437,-5.,73.8844332675354));
#39260=CARTESIAN_POINT('Ctrl Pts',(12.2783393423437,5.,73.8844332675354));
#39261=CARTESIAN_POINT('',(12.2783393423437,0.,73.8844332675354));
#39262=CARTESIAN_POINT('Ctrl Pts',(12.4804784574649,4.8,72.906075545245));
#39263=CARTESIAN_POINT('Ctrl Pts',(12.4804784574649,3.13333333333333,72.906075545245));
#39264=CARTESIAN_POINT('Ctrl Pts',(12.4804784574649,1.46666666666667,72.906075545245));
#39265=CARTESIAN_POINT('Ctrl Pts',(12.4804784574649,-1.73333333333333,72.906075545245));
#39266=CARTESIAN_POINT('Ctrl Pts',(12.4804784574649,-3.26666666666667,72.906075545245));
#39267=CARTESIAN_POINT('Ctrl Pts',(12.4804784574649,-4.8,72.906075545245));
#39268=CARTESIAN_POINT('Origin',(9.3099999999996,0.,78.0000000000005));
#39269=CARTESIAN_POINT('',(12.5915348397961,0.,74.7054546451438));
#39270=CARTESIAN_POINT('',(11.9846612632316,0.,74.1962272508773));
#39271=CARTESIAN_POINT('Origin',(12.2783393423437,0.,73.8844332675354));
#39272=CARTESIAN_POINT('Ctrl Pts',(12.8475953086752,-5.,74.3620957389297));
#39273=CARTESIAN_POINT('Ctrl Pts',(12.8475953086752,5.,74.3620957389297));
#39274=CARTESIAN_POINT('Ctrl Pts',(12.8501934647285,-5.,74.3595593860371));
#39275=CARTESIAN_POINT('Ctrl Pts',(12.8501934647285,5.,74.3595593860371));
#39276=CARTESIAN_POINT('Ctrl Pts',(12.8556442551632,-5.,74.3544011670879));
#39277=CARTESIAN_POINT('Ctrl Pts',(12.8556442551632,5.,74.3544011670879));
#39278=CARTESIAN_POINT('Ctrl Pts',(12.8645838536043,-5.,74.3464073156575));
#39279=CARTESIAN_POINT('Ctrl Pts',(12.8645838536043,5.,74.3464073156575));
#39280=CARTESIAN_POINT('Ctrl Pts',(12.8780331013787,-5.,74.3352347287054));
#39281=CARTESIAN_POINT('Ctrl Pts',(12.8780331013787,5.,74.3352347287054));
#39282=CARTESIAN_POINT('Ctrl Pts',(12.8973802923948,-5.,74.3204300963656));
#39283=CARTESIAN_POINT('Ctrl Pts',(12.8973802923948,5.,74.3204300963656));
#39284=CARTESIAN_POINT('Ctrl Pts',(12.9191964772087,-5.,74.3048473392293));
#39285=CARTESIAN_POINT('Ctrl Pts',(12.9191964772087,5.,74.3048473392293));
#39286=CARTESIAN_POINT('Ctrl Pts',(12.9433198980238,-5.,74.2886204812186));
#39287=CARTESIAN_POINT('Ctrl Pts',(12.9433198980238,5.,74.2886204812186));
#39288=CARTESIAN_POINT('Ctrl Pts',(12.9694812859721,-5.,74.2719645711802));
#39289=CARTESIAN_POINT('Ctrl Pts',(12.9694812859721,5.,74.2719645711802));
#39290=CARTESIAN_POINT('Ctrl Pts',(12.9973652192703,-5.,74.2551282242927));
#39291=CARTESIAN_POINT('Ctrl Pts',(12.9973652192703,5.,74.2551282242927));
#39292=CARTESIAN_POINT('Ctrl Pts',(13.0266581777359,-5.,74.2383558265071));
#39293=CARTESIAN_POINT('Ctrl Pts',(13.0266581777359,5.,74.2383558265071));
#39294=CARTESIAN_POINT('Ctrl Pts',(13.0570978945092,-5.,74.221848830972));
#39295=CARTESIAN_POINT('Ctrl Pts',(13.0570978945092,5.,74.221848830972));
#39296=CARTESIAN_POINT('Ctrl Pts',(13.0885311201451,-5.,74.2057199352152));
#39297=CARTESIAN_POINT('Ctrl Pts',(13.0885311201451,5.,74.2057199352152));
#39298=CARTESIAN_POINT('Ctrl Pts',(13.1208966700483,-5.,74.1900073614239));
#39299=CARTESIAN_POINT('Ctrl Pts',(13.1208966700483,5.,74.1900073614239));
#39300=CARTESIAN_POINT('Ctrl Pts',(13.1541912414913,-5.,74.1747028224464));
#39301=CARTESIAN_POINT('Ctrl Pts',(13.1541912414913,5.,74.1747028224464));
#39302=CARTESIAN_POINT('Ctrl Pts',(13.1884408770234,-5.,74.1597747542931));
#39303=CARTESIAN_POINT('Ctrl Pts',(13.1884408770234,5.,74.1597747542931));
#39304=CARTESIAN_POINT('Ctrl Pts',(13.2236714649144,-5.,74.145192175817));
#39305=CARTESIAN_POINT('Ctrl Pts',(13.2236714649144,5.,74.145192175817));
#39306=CARTESIAN_POINT('Ctrl Pts',(13.259876023226,-5.,74.1309508845651));
#39307=CARTESIAN_POINT('Ctrl Pts',(13.259876023226,5.,74.1309508845651));
#39308=CARTESIAN_POINT('Ctrl Pts',(13.2970200741795,-5.,74.1170695597709));
#39309=CARTESIAN_POINT('Ctrl Pts',(13.2970200741795,5.,74.1170695597709));
#39310=CARTESIAN_POINT('Ctrl Pts',(13.3350526082954,-5.,74.103581307568));
#39311=CARTESIAN_POINT('Ctrl Pts',(13.3350526082954,5.,74.103581307568));
#39312=CARTESIAN_POINT('Ctrl Pts',(13.3739150246539,-5.,74.0905266302112));
#39313=CARTESIAN_POINT('Ctrl Pts',(13.3739150246539,5.,74.0905266302112));
#39314=CARTESIAN_POINT('Ctrl Pts',(13.4135499722042,-5.,74.0779463262631));
#39315=CARTESIAN_POINT('Ctrl Pts',(13.4135499722042,5.,74.0779463262631));
#39316=CARTESIAN_POINT('Ctrl Pts',(13.4539117100106,-5.,74.065873000654));
#39317=CARTESIAN_POINT('Ctrl Pts',(13.4539117100106,5.,74.065873000654));
#39318=CARTESIAN_POINT('Ctrl Pts',(13.4949685665442,-5.,74.0543287622629));
#39319=CARTESIAN_POINT('Ctrl Pts',(13.4949685665442,5.,74.0543287622629));
#39320=CARTESIAN_POINT('Ctrl Pts',(13.5366989120298,-5.,74.0433279599792));
#39321=CARTESIAN_POINT('Ctrl Pts',(13.5366989120298,5.,74.0433279599792));
#39322=CARTESIAN_POINT('Ctrl Pts',(13.5790889547283,-5.,74.0328783019039));
#39323=CARTESIAN_POINT('Ctrl Pts',(13.5790889547283,5.,74.0328783019039));
#39324=CARTESIAN_POINT('Ctrl Pts',(13.6221296707664,-5.,74.0229824691757));
#39325=CARTESIAN_POINT('Ctrl Pts',(13.6221296707664,5.,74.0229824691757));
#39326=CARTESIAN_POINT('Ctrl Pts',(13.6658140788138,-5.,74.0136393542647));
#39327=CARTESIAN_POINT('Ctrl Pts',(13.6658140788138,5.,74.0136393542647));
#39328=CARTESIAN_POINT('Ctrl Pts',(13.7101340388369,-5.,74.0048453064413));
#39329=CARTESIAN_POINT('Ctrl Pts',(13.7101340388369,5.,74.0048453064413));
#39330=CARTESIAN_POINT('Ctrl Pts',(13.7550810514531,-5.,73.9965952330688));
#39331=CARTESIAN_POINT('Ctrl Pts',(13.7550810514531,5.,73.9965952330688));
#39332=CARTESIAN_POINT('Ctrl Pts',(13.8006472240049,-5.,73.9888836296951));
#39333=CARTESIAN_POINT('Ctrl Pts',(13.8006472240049,5.,73.9888836296951));
#39334=CARTESIAN_POINT('Ctrl Pts',(13.8375902833446,-5.,73.9831411376432));
#39335=CARTESIAN_POINT('Ctrl Pts',(13.8375902833446,5.,73.9831411376432));
#39336=CARTESIAN_POINT('Ctrl Pts',(13.8655712938679,-5.,73.9790727181811));
#39337=CARTESIAN_POINT('Ctrl Pts',(13.8655712938679,5.,73.9790727181811));
#39338=CARTESIAN_POINT('Ctrl Pts',(13.8843467322659,-5.,73.9764662244028));
#39339=CARTESIAN_POINT('Ctrl Pts',(13.8843467322659,5.,73.9764662244028));
#39340=CARTESIAN_POINT('Ctrl Pts',(13.8937648093287,-5.,73.9751894239903));
#39341=CARTESIAN_POINT('Ctrl Pts',(13.8937648093287,5.,73.9751894239903));
#39342=CARTESIAN_POINT('Ctrl Pts',(13.7759884897161,-4.8,73.993137535462));
#39343=CARTESIAN_POINT('Ctrl Pts',(13.7759884897161,-3.13333333333333,73.993137535462));
#39344=CARTESIAN_POINT('Ctrl Pts',(13.7759884897161,-1.46666666666667,73.993137535462));
#39345=CARTESIAN_POINT('Ctrl Pts',(13.7759884897161,1.73333333333333,73.993137535462));
#39346=CARTESIAN_POINT('Ctrl Pts',(13.7759884897161,3.26666666666667,73.993137535462));
#39347=CARTESIAN_POINT('Ctrl Pts',(13.7759884897161,4.8,73.993137535462));
#39348=CARTESIAN_POINT('',(12.8475953086752,0.,74.3620957389297));
#39349=CARTESIAN_POINT('Origin',(12.5915348397961,0.,74.7054546451438));
#39350=CARTESIAN_POINT('Ctrl Pts',(15.0874706089091,-5.,76.0427485181531));
#39351=CARTESIAN_POINT('Ctrl Pts',(15.0874706089091,5.,76.0427485181531));
#39352=CARTESIAN_POINT('Ctrl Pts',(15.0816558287596,-5.,76.0502664118982));
#39353=CARTESIAN_POINT('Ctrl Pts',(15.0816558287596,5.,76.0502664118982));
#39354=CARTESIAN_POINT('Ctrl Pts',(15.0700108196895,-5.,76.0652231715592));
#39355=CARTESIAN_POINT('Ctrl Pts',(15.0700108196895,5.,76.0652231715592));
#39356=CARTESIAN_POINT('Ctrl Pts',(15.0524969597726,-5.,76.0874212276898));
#39357=CARTESIAN_POINT('Ctrl Pts',(15.0524969597726,5.,76.0874212276898));
#39358=CARTESIAN_POINT('Ctrl Pts',(15.029052286077,-5.,76.1165436095022));
#39359=CARTESIAN_POINT('Ctrl Pts',(15.029052286077,5.,76.1165436095022));
#39360=CARTESIAN_POINT('Ctrl Pts',(14.999590755387,-5.,76.1521492708168));
#39361=CARTESIAN_POINT('Ctrl Pts',(14.999590755387,5.,76.1521492708168));
#39362=CARTESIAN_POINT('Ctrl Pts',(14.9699724759961,-5.,76.186949488945));
#39363=CARTESIAN_POINT('Ctrl Pts',(14.9699724759961,5.,76.186949488945));
#39364=CARTESIAN_POINT('Ctrl Pts',(14.9401966272196,-5.,76.22093467639));
#39365=CARTESIAN_POINT('Ctrl Pts',(14.9401966272196,5.,76.22093467639));
#39366=CARTESIAN_POINT('Ctrl Pts',(14.9102630483799,-5.,76.2540949261266));
#39367=CARTESIAN_POINT('Ctrl Pts',(14.9102630483799,5.,76.2540949261266));
#39368=CARTESIAN_POINT('Ctrl Pts',(14.8801726478579,-5.,76.2864213632965));
#39369=CARTESIAN_POINT('Ctrl Pts',(14.8801726478579,5.,76.2864213632965));
#39370=CARTESIAN_POINT('Ctrl Pts',(14.8499279571665,-5.,76.3179073881206));
#39371=CARTESIAN_POINT('Ctrl Pts',(14.8499279571665,5.,76.3179073881206));
#39372=CARTESIAN_POINT('Ctrl Pts',(14.8195358101786,-5.,76.3485465262688));
#39373=CARTESIAN_POINT('Ctrl Pts',(14.8195358101786,5.,76.3485465262688));
#39374=CARTESIAN_POINT('Ctrl Pts',(14.7890097781812,-5.,76.3783306878053));
#39375=CARTESIAN_POINT('Ctrl Pts',(14.7890097781812,5.,76.3783306878053));
#39376=CARTESIAN_POINT('Ctrl Pts',(14.7583731025724,-5.,76.4072483152522));
#39377=CARTESIAN_POINT('Ctrl Pts',(14.7583731025724,5.,76.4072483152522));
#39378=CARTESIAN_POINT('Ctrl Pts',(14.7276607659748,-5.,76.4352830347113));
#39379=CARTESIAN_POINT('Ctrl Pts',(14.7276607659748,5.,76.4352830347113));
#39380=CARTESIAN_POINT('Ctrl Pts',(14.6969238755583,-5.,76.4624115358413));
#39381=CARTESIAN_POINT('Ctrl Pts',(14.6969238755583,5.,76.4624115358413));
#39382=CARTESIAN_POINT('Ctrl Pts',(14.6662264394396,-5.,76.4886045504555));
#39383=CARTESIAN_POINT('Ctrl Pts',(14.6662264394396,5.,76.4886045504555));
#39384=CARTESIAN_POINT('Ctrl Pts',(14.6356328340581,-5.,76.5138315797917));
#39385=CARTESIAN_POINT('Ctrl Pts',(14.6356328340581,5.,76.5138315797917));
#39386=CARTESIAN_POINT('Ctrl Pts',(14.6051972349025,-5.,76.5380650014057));
#39387=CARTESIAN_POINT('Ctrl Pts',(14.6051972349025,5.,76.5380650014057));
#39388=CARTESIAN_POINT('Ctrl Pts',(14.5749530575496,-5.,76.5612842962772));
#39389=CARTESIAN_POINT('Ctrl Pts',(14.5749530575496,5.,76.5612842962772));
#39390=CARTESIAN_POINT('Ctrl Pts',(14.5449001535355,-5.,76.583481316641));
#39391=CARTESIAN_POINT('Ctrl Pts',(14.5449001535355,5.,76.583481316641));
#39392=CARTESIAN_POINT('Ctrl Pts',(14.5149987482656,-5.,76.6046629918255));
#39393=CARTESIAN_POINT('Ctrl Pts',(14.5149987482656,5.,76.6046629918255));
#39394=CARTESIAN_POINT('Ctrl Pts',(14.4852084852497,-5.,76.6248360933492));
#39395=CARTESIAN_POINT('Ctrl Pts',(14.4852084852497,5.,76.6248360933492));
#39396=CARTESIAN_POINT('Ctrl Pts',(14.4555238389698,-5.,76.6439936173949));
#39397=CARTESIAN_POINT('Ctrl Pts',(14.4555238389698,5.,76.6439936173949));
#39398=CARTESIAN_POINT('Ctrl Pts',(14.4260085031102,-5.,76.6621016876444));
#39399=CARTESIAN_POINT('Ctrl Pts',(14.4260085031102,5.,76.6621016876444));
#39400=CARTESIAN_POINT('Ctrl Pts',(14.3968367013156,-5.,76.6790839349479));
#39401=CARTESIAN_POINT('Ctrl Pts',(14.3968367013156,5.,76.6790839349479));
#39402=CARTESIAN_POINT('Ctrl Pts',(14.3683140305578,-5.,76.6948139561085));
#39403=CARTESIAN_POINT('Ctrl Pts',(14.3683140305578,5.,76.6948139561085));
#39404=CARTESIAN_POINT('Ctrl Pts',(14.3408088953677,-5.,76.709142427651));
#39405=CARTESIAN_POINT('Ctrl Pts',(14.3408088953677,5.,76.709142427651));
#39406=CARTESIAN_POINT('Ctrl Pts',(14.3146943136958,-5.,76.7219204938828));
#39407=CARTESIAN_POINT('Ctrl Pts',(14.3146943136958,5.,76.7219204938828));
#39408=CARTESIAN_POINT('Ctrl Pts',(14.2902911577409,-5.,76.7330224855497));
#39409=CARTESIAN_POINT('Ctrl Pts',(14.2902911577409,5.,76.7330224855497));
#39410=CARTESIAN_POINT('Ctrl Pts',(14.2677963745262,-5.,76.7423753282655));
#39411=CARTESIAN_POINT('Ctrl Pts',(14.2677963745262,5.,76.7423753282655));
#39412=CARTESIAN_POINT('Ctrl Pts',(14.2513960065121,-5.,76.7484364250213));
#39413=CARTESIAN_POINT('Ctrl Pts',(14.2513960065121,5.,76.7484364250213));
#39414=CARTESIAN_POINT('Ctrl Pts',(14.2400033288828,-5.,76.7521814186714));
#39415=CARTESIAN_POINT('Ctrl Pts',(14.2400033288828,5.,76.7521814186714));
#39416=CARTESIAN_POINT('Ctrl Pts',(14.2328107850219,-5.,76.7543228322031));
#39417=CARTESIAN_POINT('Ctrl Pts',(14.2328107850219,5.,76.7543228322031));
#39418=CARTESIAN_POINT('Ctrl Pts',(14.2293151609602,-5.,76.7553047249138));
#39419=CARTESIAN_POINT('Ctrl Pts',(14.2293151609602,5.,76.7553047249138));
#39420=CARTESIAN_POINT('',(14.2293151609602,0.,76.7553047249138));
#39421=CARTESIAN_POINT('Ctrl Pts',(15.0130389285309,4.8,76.1357717468986));
#39422=CARTESIAN_POINT('Ctrl Pts',(15.0130389285309,3.13333333333333,76.1357717468986));
#39423=CARTESIAN_POINT('Ctrl Pts',(15.0130389285309,1.46666666666667,76.1357717468986));
#39424=CARTESIAN_POINT('Ctrl Pts',(15.0130389285309,-1.73333333333333,76.1357717468986));
#39425=CARTESIAN_POINT('Ctrl Pts',(15.0130389285309,-3.26666666666667,76.1357717468986));
#39426=CARTESIAN_POINT('Ctrl Pts',(15.0130389285309,-4.8,76.1357717468986));
#39427=CARTESIAN_POINT('Origin',(9.30999999999972,0.,78.0000000000001));
#39428=CARTESIAN_POINT('',(13.941494462579,0.,77.5855617740846));
#39429=CARTESIAN_POINT('',(13.8039273911235,0.,76.805380142761));
#39430=CARTESIAN_POINT('Origin',(14.2293151609602,0.,76.7553047249138));
#39431=CARTESIAN_POINT('Ctrl Pts',(14.3583550124563,-5.,77.4871260887099));
#39432=CARTESIAN_POINT('Ctrl Pts',(14.3583550124563,5.,77.4871260887099));
#39433=CARTESIAN_POINT('Ctrl Pts',(14.3619756516734,-5.,77.4868531921847));
#39434=CARTESIAN_POINT('Ctrl Pts',(14.3619756516734,5.,77.4868531921847));
#39435=CARTESIAN_POINT('Ctrl Pts',(14.3694668386202,-5.,77.4864054677684));
#39436=CARTESIAN_POINT('Ctrl Pts',(14.3694668386202,5.,77.4864054677684));
#39437=CARTESIAN_POINT('Ctrl Pts',(14.3814533169788,-5.,77.486028085408));
#39438=CARTESIAN_POINT('Ctrl Pts',(14.3814533169788,5.,77.486028085408));
#39439=CARTESIAN_POINT('Ctrl Pts',(14.3989376389619,-5.,77.4861143970885));
#39440=CARTESIAN_POINT('Ctrl Pts',(14.3989376389619,5.,77.4861143970885));
#39441=CARTESIAN_POINT('Ctrl Pts',(14.4232746813706,-5.,77.4872095254305));
#39442=CARTESIAN_POINT('Ctrl Pts',(14.4232746813706,5.,77.4872095254305));
#39443=CARTESIAN_POINT('Ctrl Pts',(14.4500032517364,-5.,77.4892956142184));
#39444=CARTESIAN_POINT('Ctrl Pts',(14.4500032517364,5.,77.4892956142184));
#39445=CARTESIAN_POINT('Ctrl Pts',(14.478913287478,-5.,77.4923713558196));
#39446=CARTESIAN_POINT('Ctrl Pts',(14.478913287478,5.,77.4923713558196));
#39447=CARTESIAN_POINT('Ctrl Pts',(14.5096602859406,-5.,77.4964284045148));
#39448=CARTESIAN_POINT('Ctrl Pts',(14.5096602859406,5.,77.4964284045148));
#39449=CARTESIAN_POINT('Ctrl Pts',(14.5418428132648,-5.,77.5014544613684));
#39450=CARTESIAN_POINT('Ctrl Pts',(14.5418428132648,5.,77.5014544613684));
#39451=CARTESIAN_POINT('Ctrl Pts',(14.575063610798,-5.,77.5074352099942));
#39452=CARTESIAN_POINT('Ctrl Pts',(14.575063610798,5.,77.5074352099942));
#39453=CARTESIAN_POINT('Ctrl Pts',(14.6089922788841,-5.,77.5143563905722));
#39454=CARTESIAN_POINT('Ctrl Pts',(14.6089922788841,5.,77.5143563905722));
#39455=CARTESIAN_POINT('Ctrl Pts',(14.6434389810628,-5.,77.5222058275741));
#39456=CARTESIAN_POINT('Ctrl Pts',(14.6434389810628,5.,77.5222058275741));
#39457=CARTESIAN_POINT('Ctrl Pts',(14.6783322784657,-5.,77.5309734721938));
#39458=CARTESIAN_POINT('Ctrl Pts',(14.6783322784657,5.,77.5309734721938));
#39459=CARTESIAN_POINT('Ctrl Pts',(14.7136749679333,-5.,77.5406508531512));
#39460=CARTESIAN_POINT('Ctrl Pts',(14.7136749679333,5.,77.5406508531512));
#39461=CARTESIAN_POINT('Ctrl Pts',(14.7495072881561,-5.,77.5512305308537));
#39462=CARTESIAN_POINT('Ctrl Pts',(14.7495072881561,5.,77.5512305308537));
#39463=CARTESIAN_POINT('Ctrl Pts',(14.7858689849959,-5.,77.5627054130239));
#39464=CARTESIAN_POINT('Ctrl Pts',(14.7858689849959,5.,77.5627054130239));
#39465=CARTESIAN_POINT('Ctrl Pts',(14.8227574112639,-5.,77.575067792493));
#39466=CARTESIAN_POINT('Ctrl Pts',(14.8227574112639,5.,77.575067792493));
#39467=CARTESIAN_POINT('Ctrl Pts',(14.8601341486718,-5.,77.5883098164962));
#39468=CARTESIAN_POINT('Ctrl Pts',(14.8601341486718,5.,77.5883098164962));
#39469=CARTESIAN_POINT('Ctrl Pts',(14.8979388414815,-5.,77.6024240575431));
#39470=CARTESIAN_POINT('Ctrl Pts',(14.8979388414815,5.,77.6024240575431));
#39471=CARTESIAN_POINT('Ctrl Pts',(14.936100564438,-5.,77.6174038742163));
#39472=CARTESIAN_POINT('Ctrl Pts',(14.936100564438,5.,77.6174038742163));
#39473=CARTESIAN_POINT('Ctrl Pts',(14.9745491592773,-5.,77.6332436554837));
#39474=CARTESIAN_POINT('Ctrl Pts',(14.9745491592773,5.,77.6332436554837));
#39475=CARTESIAN_POINT('Ctrl Pts',(15.0132286283616,-5.,77.6499389764632));
#39476=CARTESIAN_POINT('Ctrl Pts',(15.0132286283616,5.,77.6499389764632));
#39477=CARTESIAN_POINT('Ctrl Pts',(15.0521004985737,-5.,77.6674864154704));
#39478=CARTESIAN_POINT('Ctrl Pts',(15.0521004985737,5.,77.6674864154704));
#39479=CARTESIAN_POINT('Ctrl Pts',(15.0911389772507,-5.,77.685883061039));
#39480=CARTESIAN_POINT('Ctrl Pts',(15.0911389772507,5.,77.685883061039));
#39481=CARTESIAN_POINT('Ctrl Pts',(15.1303285446315,-5.,77.705125952756));
#39482=CARTESIAN_POINT('Ctrl Pts',(15.1303285446315,5.,77.705125952756));
#39483=CARTESIAN_POINT('Ctrl Pts',(15.1696605646238,-5.,77.7252113440577));
#39484=CARTESIAN_POINT('Ctrl Pts',(15.1696605646238,5.,77.7252113440577));
#39485=CARTESIAN_POINT('Ctrl Pts',(15.2091304011272,-5.,77.7461338990148));
#39486=CARTESIAN_POINT('Ctrl Pts',(15.2091304011272,5.,77.7461338990148));
#39487=CARTESIAN_POINT('Ctrl Pts',(15.2487341651656,-5.,77.7678855886962));
#39488=CARTESIAN_POINT('Ctrl Pts',(15.2487341651656,5.,77.7678855886962));
#39489=CARTESIAN_POINT('Ctrl Pts',(15.2884686193296,-5.,77.7904570486235));
#39490=CARTESIAN_POINT('Ctrl Pts',(15.2884686193296,5.,77.7904570486235));
#39491=CARTESIAN_POINT('Ctrl Pts',(15.3283312556985,-5.,77.8138389888447));
#39492=CARTESIAN_POINT('Ctrl Pts',(15.3283312556985,5.,77.8138389888447));
#39493=CARTESIAN_POINT('Ctrl Pts',(15.3603224837765,-5.,77.8331865255343));
#39494=CARTESIAN_POINT('Ctrl Pts',(15.3603224837765,5.,77.8331865255343));
#39495=CARTESIAN_POINT('Ctrl Pts',(15.3843723110553,-5.,77.8480557822982));
#39496=CARTESIAN_POINT('Ctrl Pts',(15.3843723110553,5.,77.8480557822982));
#39497=CARTESIAN_POINT('Ctrl Pts',(15.4004305532434,-5.,77.8581277114053));
#39498=CARTESIAN_POINT('Ctrl Pts',(15.4004305532434,5.,77.8581277114053));
#39499=CARTESIAN_POINT('Ctrl Pts',(15.408465930345,-5.,77.8632034487949));
#39500=CARTESIAN_POINT('Ctrl Pts',(15.408465930345,5.,77.8632034487949));
#39501=CARTESIAN_POINT('Ctrl Pts',(15.3067072115039,-4.8,77.8012473409061));
#39502=CARTESIAN_POINT('Ctrl Pts',(15.3067072115039,-3.13333333333333,77.8012473409061));
#39503=CARTESIAN_POINT('Ctrl Pts',(15.3067072115039,-1.46666666666667,77.8012473409061));
#39504=CARTESIAN_POINT('Ctrl Pts',(15.3067072115039,1.73333333333333,77.8012473409061));
#39505=CARTESIAN_POINT('Ctrl Pts',(15.3067072115039,3.26666666666667,77.8012473409061));
#39506=CARTESIAN_POINT('Ctrl Pts',(15.3067072115039,4.8,77.8012473409061));
#39507=CARTESIAN_POINT('',(14.3583550124563,0.,77.4871260887099));
#39508=CARTESIAN_POINT('Origin',(13.941494462579,0.,77.5855617740846));
#39509=CARTESIAN_POINT('Ctrl Pts',(15.408465930345,-5.,78.1367965512051));
#39510=CARTESIAN_POINT('Ctrl Pts',(15.408465930345,5.,78.1367965512051));
#39511=CARTESIAN_POINT('Ctrl Pts',(15.4004305532433,-5.,78.1418722885381));
#39512=CARTESIAN_POINT('Ctrl Pts',(15.4004305532433,5.,78.1418722885381));
#39513=CARTESIAN_POINT('Ctrl Pts',(15.3843723110551,-5.,78.1519442175461));
#39514=CARTESIAN_POINT('Ctrl Pts',(15.3843723110551,5.,78.1519442175461));
#39515=CARTESIAN_POINT('Ctrl Pts',(15.3603224837762,-5.,78.1668134742034));
#39516=CARTESIAN_POINT('Ctrl Pts',(15.3603224837762,5.,78.1668134742034));
#39517=CARTESIAN_POINT('Ctrl Pts',(15.3283312556981,-5.,78.1861610108314));
#39518=CARTESIAN_POINT('Ctrl Pts',(15.3283312556981,5.,78.1861610108314));
#39519=CARTESIAN_POINT('Ctrl Pts',(15.2884686193292,-5.,78.2095429510792));
#39520=CARTESIAN_POINT('Ctrl Pts',(15.2884686193292,5.,78.2095429510792));
#39521=CARTESIAN_POINT('Ctrl Pts',(15.2487341651653,-5.,78.2321144110984));
#39522=CARTESIAN_POINT('Ctrl Pts',(15.2487341651653,5.,78.2321144110984));
#39523=CARTESIAN_POINT('Ctrl Pts',(15.2091304011271,-5.,78.2538661008963));
#39524=CARTESIAN_POINT('Ctrl Pts',(15.2091304011271,5.,78.2538661008963));
#39525=CARTESIAN_POINT('Ctrl Pts',(15.1696605646239,-5.,78.2747886559577));
#39526=CARTESIAN_POINT('Ctrl Pts',(15.1696605646239,5.,78.2747886559577));
#39527=CARTESIAN_POINT('Ctrl Pts',(15.1303285446317,-5.,78.2948740473268));
#39528=CARTESIAN_POINT('Ctrl Pts',(15.1303285446317,5.,78.2948740473268));
#39529=CARTESIAN_POINT('Ctrl Pts',(15.0911389772509,-5.,78.3141169390679));
#39530=CARTESIAN_POINT('Ctrl Pts',(15.0911389772509,5.,78.3141169390679));
#39531=CARTESIAN_POINT('Ctrl Pts',(15.0521004985739,-5.,78.3325135846235));
#39532=CARTESIAN_POINT('Ctrl Pts',(15.0521004985739,5.,78.3325135846235));
#39533=CARTESIAN_POINT('Ctrl Pts',(15.0132286283617,-5.,78.3500610235947));
#39534=CARTESIAN_POINT('Ctrl Pts',(15.0132286283617,5.,78.3500610235947));
#39535=CARTESIAN_POINT('Ctrl Pts',(14.9745491592773,-5.,78.3667563445323));
#39536=CARTESIAN_POINT('Ctrl Pts',(14.9745491592773,5.,78.3667563445323));
#39537=CARTESIAN_POINT('Ctrl Pts',(14.936100564438,-5.,78.3825961257675));
#39538=CARTESIAN_POINT('Ctrl Pts',(14.936100564438,5.,78.3825961257675));
#39539=CARTESIAN_POINT('Ctrl Pts',(14.8979388414814,-5.,78.3975759424268));
#39540=CARTESIAN_POINT('Ctrl Pts',(14.8979388414814,5.,78.3975759424268));
#39541=CARTESIAN_POINT('Ctrl Pts',(14.8601341486718,-5.,78.4116901834755));
#39542=CARTESIAN_POINT('Ctrl Pts',(14.8601341486718,5.,78.4116901834755));
#39543=CARTESIAN_POINT('Ctrl Pts',(14.8227574112638,-5.,78.4249322074904));
#39544=CARTESIAN_POINT('Ctrl Pts',(14.8227574112638,5.,78.4249322074904));
#39545=CARTESIAN_POINT('Ctrl Pts',(14.7858689849959,-5.,78.4372945869721));
#39546=CARTESIAN_POINT('Ctrl Pts',(14.7858689849959,5.,78.4372945869721));
#39547=CARTESIAN_POINT('Ctrl Pts',(14.7495072881561,-5.,78.4487694691489));
#39548=CARTESIAN_POINT('Ctrl Pts',(14.7495072881561,5.,78.4487694691489));
#39549=CARTESIAN_POINT('Ctrl Pts',(14.7136749679335,-5.,78.4593491468485));
#39550=CARTESIAN_POINT('Ctrl Pts',(14.7136749679335,5.,78.4593491468485));
#39551=CARTESIAN_POINT('Ctrl Pts',(14.678332278466,-5.,78.4690265277979));
#39552=CARTESIAN_POINT('Ctrl Pts',(14.678332278466,5.,78.4690265277979));
#39553=CARTESIAN_POINT('Ctrl Pts',(14.6434389810631,-5.,78.4777941724113));
#39554=CARTESIAN_POINT('Ctrl Pts',(14.6434389810631,5.,78.4777941724113));
#39555=CARTESIAN_POINT('Ctrl Pts',(14.6089922788842,-5.,78.4856436094153));
#39556=CARTESIAN_POINT('Ctrl Pts',(14.6089922788842,5.,78.4856436094153));
#39557=CARTESIAN_POINT('Ctrl Pts',(14.575063610798,-5.,78.492564790007));
#39558=CARTESIAN_POINT('Ctrl Pts',(14.575063610798,5.,78.492564790007));
#39559=CARTESIAN_POINT('Ctrl Pts',(14.5418428132646,-5.,78.498545538655));
#39560=CARTESIAN_POINT('Ctrl Pts',(14.5418428132646,5.,78.498545538655));
#39561=CARTESIAN_POINT('Ctrl Pts',(14.5096602859403,-5.,78.5035715955264));
#39562=CARTESIAN_POINT('Ctrl Pts',(14.5096602859403,5.,78.5035715955264));
#39563=CARTESIAN_POINT('Ctrl Pts',(14.4789132874778,-5.,78.5076286442221));
#39564=CARTESIAN_POINT('Ctrl Pts',(14.4789132874778,5.,78.5076286442221));
#39565=CARTESIAN_POINT('Ctrl Pts',(14.4500032517364,-5.,78.5107043857979));
#39566=CARTESIAN_POINT('Ctrl Pts',(14.4500032517364,5.,78.5107043857979));
#39567=CARTESIAN_POINT('Ctrl Pts',(14.4232746813707,-5.,78.5127904745387));
#39568=CARTESIAN_POINT('Ctrl Pts',(14.4232746813707,5.,78.5127904745387));
#39569=CARTESIAN_POINT('Ctrl Pts',(14.3989376389621,-5.,78.513885602836));
#39570=CARTESIAN_POINT('Ctrl Pts',(14.3989376389621,5.,78.513885602836));
#39571=CARTESIAN_POINT('Ctrl Pts',(14.3814533169789,-5.,78.5139719145117));
#39572=CARTESIAN_POINT('Ctrl Pts',(14.3814533169789,5.,78.5139719145117));
#39573=CARTESIAN_POINT('Ctrl Pts',(14.3694668386203,-5.,78.5135945321781));
#39574=CARTESIAN_POINT('Ctrl Pts',(14.3694668386203,5.,78.5135945321781));
#39575=CARTESIAN_POINT('Ctrl Pts',(14.3619756516734,-5.,78.5131468077949));
#39576=CARTESIAN_POINT('Ctrl Pts',(14.3619756516734,5.,78.5131468077949));
#39577=CARTESIAN_POINT('Ctrl Pts',(14.3583550124563,-5.,78.5128739112901));
#39578=CARTESIAN_POINT('Ctrl Pts',(14.3583550124563,5.,78.5128739112901));
#39579=CARTESIAN_POINT('',(14.3583550124563,0.,78.5128739112901));
#39580=CARTESIAN_POINT('Ctrl Pts',(15.306707211514,4.8,78.1987526587886));
#39581=CARTESIAN_POINT('Ctrl Pts',(15.306707211514,3.13333333333333,78.1987526587886));
#39582=CARTESIAN_POINT('Ctrl Pts',(15.306707211514,1.46666666666667,78.1987526587886));
#39583=CARTESIAN_POINT('Ctrl Pts',(15.306707211514,-1.73333333333333,78.1987526587886));
#39584=CARTESIAN_POINT('Ctrl Pts',(15.306707211514,-3.26666666666667,78.1987526587886));
#39585=CARTESIAN_POINT('Ctrl Pts',(15.306707211514,-4.8,78.1987526587886));
#39586=CARTESIAN_POINT('Origin',(9.30999999999925,0.,77.9999999999999));
#39587=CARTESIAN_POINT('',(13.8039273911235,0.,79.194619857239));
#39588=CARTESIAN_POINT('',(13.941494462579,0.,78.4144382259154));
#39589=CARTESIAN_POINT('Origin',(14.3583550124563,0.,78.5128739112901));
#39590=CARTESIAN_POINT('Ctrl Pts',(14.2293151609602,-5.,79.2446952750862));
#39591=CARTESIAN_POINT('Ctrl Pts',(14.2293151609602,5.,79.2446952750862));
#39592=CARTESIAN_POINT('Ctrl Pts',(14.2328107850219,-5.,79.2456771677792));
#39593=CARTESIAN_POINT('Ctrl Pts',(14.2328107850219,5.,79.2456771677792));
#39594=CARTESIAN_POINT('Ctrl Pts',(14.2400033288829,-5.,79.247818581282));
#39595=CARTESIAN_POINT('Ctrl Pts',(14.2400033288829,5.,79.247818581282));
#39596=CARTESIAN_POINT('Ctrl Pts',(14.2513960065123,-5.,79.2515635749088));
#39597=CARTESIAN_POINT('Ctrl Pts',(14.2513960065123,5.,79.2515635749088));
#39598=CARTESIAN_POINT('Ctrl Pts',(14.2677963745263,-5.,79.2576246716687));
#39599=CARTESIAN_POINT('Ctrl Pts',(14.2677963745263,5.,79.2576246716687));
#39600=CARTESIAN_POINT('Ctrl Pts',(14.290291157741,-5.,79.2669775144234));
#39601=CARTESIAN_POINT('Ctrl Pts',(14.290291157741,5.,79.2669775144234));
#39602=CARTESIAN_POINT('Ctrl Pts',(14.3146943136958,-5.,79.2780795061314));
#39603=CARTESIAN_POINT('Ctrl Pts',(14.3146943136958,5.,79.2780795061314));
#39604=CARTESIAN_POINT('Ctrl Pts',(14.3408088953677,-5.,79.2908575723857));
#39605=CARTESIAN_POINT('Ctrl Pts',(14.3408088953677,5.,79.2908575723857));
#39606=CARTESIAN_POINT('Ctrl Pts',(14.3683140305578,-5.,79.305186043928));
#39607=CARTESIAN_POINT('Ctrl Pts',(14.3683140305578,5.,79.305186043928));
#39608=CARTESIAN_POINT('Ctrl Pts',(14.3968367013155,-5.,79.3209160650726));
#39609=CARTESIAN_POINT('Ctrl Pts',(14.3968367013155,5.,79.3209160650726));
#39610=CARTESIAN_POINT('Ctrl Pts',(14.4260085031102,-5.,79.3378983123566));
#39611=CARTESIAN_POINT('Ctrl Pts',(14.4260085031102,5.,79.3378983123566));
#39612=CARTESIAN_POINT('Ctrl Pts',(14.4555238389699,-5.,79.3560063825941));
#39613=CARTESIAN_POINT('Ctrl Pts',(14.4555238389699,5.,79.3560063825941));
#39614=CARTESIAN_POINT('Ctrl Pts',(14.4852084852499,-5.,79.3751639066383));
#39615=CARTESIAN_POINT('Ctrl Pts',(14.4852084852499,5.,79.3751639066383));
#39616=CARTESIAN_POINT('Ctrl Pts',(14.514998748266,-5.,79.395337008168));
#39617=CARTESIAN_POINT('Ctrl Pts',(14.514998748266,5.,79.395337008168));
#39618=CARTESIAN_POINT('Ctrl Pts',(14.5449001535359,-5.,79.4165186833593));
#39619=CARTESIAN_POINT('Ctrl Pts',(14.5449001535359,5.,79.4165186833593));
#39620=CARTESIAN_POINT('Ctrl Pts',(14.5749530575497,-5.,79.4387157037252));
#39621=CARTESIAN_POINT('Ctrl Pts',(14.5749530575497,5.,79.4387157037252));
#39622=CARTESIAN_POINT('Ctrl Pts',(14.6051972349022,-5.,79.4619349985905));
#39623=CARTESIAN_POINT('Ctrl Pts',(14.6051972349022,5.,79.4619349985905));
#39624=CARTESIAN_POINT('Ctrl Pts',(14.6356328340575,-5.,79.4861684201933));
#39625=CARTESIAN_POINT('Ctrl Pts',(14.6356328340575,5.,79.4861684201933));
#39626=CARTESIAN_POINT('Ctrl Pts',(14.6662264394389,-5.,79.5113954495195));
#39627=CARTESIAN_POINT('Ctrl Pts',(14.6662264394389,5.,79.5113954495195));
#39628=CARTESIAN_POINT('Ctrl Pts',(14.6969238755576,-5.,79.5375884641322));
#39629=CARTESIAN_POINT('Ctrl Pts',(14.6969238755576,5.,79.5375884641322));
#39630=CARTESIAN_POINT('Ctrl Pts',(14.7276607659746,-5.,79.5647169652746));
#39631=CARTESIAN_POINT('Ctrl Pts',(14.7276607659746,5.,79.5647169652746));
#39632=CARTESIAN_POINT('Ctrl Pts',(14.7583731025727,-5.,79.5927516847618));
#39633=CARTESIAN_POINT('Ctrl Pts',(14.7583731025727,5.,79.5927516847618));
#39634=CARTESIAN_POINT('Ctrl Pts',(14.789009778182,-5.,79.6216693122451));
#39635=CARTESIAN_POINT('Ctrl Pts',(14.789009778182,5.,79.6216693122451));
#39636=CARTESIAN_POINT('Ctrl Pts',(14.8195358101796,-5.,79.6514534738131));
#39637=CARTESIAN_POINT('Ctrl Pts',(14.8195358101796,5.,79.6514534738131));
#39638=CARTESIAN_POINT('Ctrl Pts',(14.8499279571675,-5.,79.6820926119728));
#39639=CARTESIAN_POINT('Ctrl Pts',(14.8499279571675,5.,79.6820926119728));
#39640=CARTESIAN_POINT('Ctrl Pts',(14.8801726478586,-5.,79.7135786367758));
#39641=CARTESIAN_POINT('Ctrl Pts',(14.8801726478586,5.,79.7135786367758));
#39642=CARTESIAN_POINT('Ctrl Pts',(14.91026304838,-5.,79.7459050738868));
#39643=CARTESIAN_POINT('Ctrl Pts',(14.91026304838,5.,79.7459050738868));
#39644=CARTESIAN_POINT('Ctrl Pts',(14.9401966272191,-5.,79.7790653235324));
#39645=CARTESIAN_POINT('Ctrl Pts',(14.9401966272191,5.,79.7790653235324));
#39646=CARTESIAN_POINT('Ctrl Pts',(14.969972475995,-5.,79.8130505108762));
#39647=CARTESIAN_POINT('Ctrl Pts',(14.969972475995,5.,79.8130505108762));
#39648=CARTESIAN_POINT('Ctrl Pts',(14.9995907553857,-5.,79.8478507289248));
#39649=CARTESIAN_POINT('Ctrl Pts',(14.9995907553857,5.,79.8478507289248));
#39650=CARTESIAN_POINT('Ctrl Pts',(15.0290522860757,-5.,79.8834563902168));
#39651=CARTESIAN_POINT('Ctrl Pts',(15.0290522860757,5.,79.8834563902168));
#39652=CARTESIAN_POINT('Ctrl Pts',(15.0524969597716,-5.,79.9125787720828));
#39653=CARTESIAN_POINT('Ctrl Pts',(15.0524969597716,5.,79.9125787720828));
#39654=CARTESIAN_POINT('Ctrl Pts',(15.0700108196889,-5.,79.934776828306));
#39655=CARTESIAN_POINT('Ctrl Pts',(15.0700108196889,5.,79.934776828306));
#39656=CARTESIAN_POINT('Ctrl Pts',(15.0816558287594,-5.,79.9497335880528));
#39657=CARTESIAN_POINT('Ctrl Pts',(15.0816558287594,5.,79.9497335880528));
#39658=CARTESIAN_POINT('Ctrl Pts',(15.0874706089091,-5.,79.9572514818469));
#39659=CARTESIAN_POINT('Ctrl Pts',(15.0874706089091,5.,79.9572514818469));
#39660=CARTESIAN_POINT('Ctrl Pts',(15.0130389285914,-4.8,79.8642282529162));
#39661=CARTESIAN_POINT('Ctrl Pts',(15.0130389285914,-3.13333333333333,79.8642282529162));
#39662=CARTESIAN_POINT('Ctrl Pts',(15.0130389285914,-1.46666666666667,79.8642282529162));
#39663=CARTESIAN_POINT('Ctrl Pts',(15.0130389285914,1.73333333333333,79.8642282529162));
#39664=CARTESIAN_POINT('Ctrl Pts',(15.0130389285914,3.26666666666667,79.8642282529162));
#39665=CARTESIAN_POINT('Ctrl Pts',(15.0130389285914,4.8,79.8642282529162));
#39666=CARTESIAN_POINT('',(14.2293151609602,0.,79.2446952750862));
#39667=CARTESIAN_POINT('Origin',(13.8039273911235,0.,79.194619857239));
#39668=CARTESIAN_POINT('Ctrl Pts',(13.8937648093287,-5.,82.0248105760097));
#39669=CARTESIAN_POINT('Ctrl Pts',(13.8937648093287,5.,82.0248105760097));
#39670=CARTESIAN_POINT('Ctrl Pts',(13.8843467322662,-5.,82.0235337755467));
#39671=CARTESIAN_POINT('Ctrl Pts',(13.8843467322662,5.,82.0235337755467));
#39672=CARTESIAN_POINT('Ctrl Pts',(13.8655712938686,-5.,82.02092728168));
#39673=CARTESIAN_POINT('Ctrl Pts',(13.8655712938686,5.,82.02092728168));
#39674=CARTESIAN_POINT('Ctrl Pts',(13.8375902833457,-5.,82.0168588621226));
#39675=CARTESIAN_POINT('Ctrl Pts',(13.8375902833457,5.,82.0168588621226));
#39676=CARTESIAN_POINT('Ctrl Pts',(13.8006472240062,-5.,82.0111163700153));
#39677=CARTESIAN_POINT('Ctrl Pts',(13.8006472240062,5.,82.0111163700153));
#39678=CARTESIAN_POINT('Ctrl Pts',(13.7550810514543,-5.,82.0034047666646));
#39679=CARTESIAN_POINT('Ctrl Pts',(13.7550810514543,5.,82.0034047666646));
#39680=CARTESIAN_POINT('Ctrl Pts',(13.7101340388377,-5.,81.9951546933737));
#39681=CARTESIAN_POINT('Ctrl Pts',(13.7101340388377,5.,81.9951546933737));
#39682=CARTESIAN_POINT('Ctrl Pts',(13.6658140788142,-5.,81.9863606456546));
#39683=CARTESIAN_POINT('Ctrl Pts',(13.6658140788142,5.,81.9863606456546));
#39684=CARTESIAN_POINT('Ctrl Pts',(13.6221296707664,-5.,81.9770175308379));
#39685=CARTESIAN_POINT('Ctrl Pts',(13.6221296707664,5.,81.9770175308379));
#39686=CARTESIAN_POINT('Ctrl Pts',(13.579088954728,-5.,81.9671216981718));
#39687=CARTESIAN_POINT('Ctrl Pts',(13.579088954728,5.,81.9671216981718));
#39688=CARTESIAN_POINT('Ctrl Pts',(13.5366989120296,-5.,81.9566720401197));
#39689=CARTESIAN_POINT('Ctrl Pts',(13.5366989120296,5.,81.9566720401197));
#39690=CARTESIAN_POINT('Ctrl Pts',(13.4949685665442,-5.,81.9456712378251));
#39691=CARTESIAN_POINT('Ctrl Pts',(13.4949685665442,5.,81.9456712378251));
#39692=CARTESIAN_POINT('Ctrl Pts',(13.4539117100108,-5.,81.9341269994011));
#39693=CARTESIAN_POINT('Ctrl Pts',(13.4539117100108,5.,81.9341269994011));
#39694=CARTESIAN_POINT('Ctrl Pts',(13.4135499722044,-5.,81.9220536737527));
#39695=CARTESIAN_POINT('Ctrl Pts',(13.4135499722044,5.,81.9220536737527));
#39696=CARTESIAN_POINT('Ctrl Pts',(13.3739150246538,-5.,81.9094733697732));
#39697=CARTESIAN_POINT('Ctrl Pts',(13.3739150246538,5.,81.9094733697732));
#39698=CARTESIAN_POINT('Ctrl Pts',(13.3350526082949,-5.,81.8964186924009));
#39699=CARTESIAN_POINT('Ctrl Pts',(13.3350526082949,5.,81.8964186924009));
#39700=CARTESIAN_POINT('Ctrl Pts',(13.2970200741786,-5.,81.8829304401978));
#39701=CARTESIAN_POINT('Ctrl Pts',(13.2970200741786,5.,81.8829304401978));
#39702=CARTESIAN_POINT('Ctrl Pts',(13.2598760232249,-5.,81.8690491154141));
#39703=CARTESIAN_POINT('Ctrl Pts',(13.2598760232249,5.,81.8690491154141));
#39704=CARTESIAN_POINT('Ctrl Pts',(13.2236714649137,-5.,81.8548078241759));
#39705=CARTESIAN_POINT('Ctrl Pts',(13.2236714649137,5.,81.8548078241759));
#39706=CARTESIAN_POINT('Ctrl Pts',(13.1884408770234,-5.,81.8402252457097));
#39707=CARTESIAN_POINT('Ctrl Pts',(13.1884408770234,5.,81.8402252457097));
#39708=CARTESIAN_POINT('Ctrl Pts',(13.1541912414923,-5.,81.8252971775583));
#39709=CARTESIAN_POINT('Ctrl Pts',(13.1541912414923,5.,81.8252971775583));
#39710=CARTESIAN_POINT('Ctrl Pts',(13.1208966700501,-5.,81.8099926385766));
#39711=CARTESIAN_POINT('Ctrl Pts',(13.1208966700501,5.,81.8099926385766));
#39712=CARTESIAN_POINT('Ctrl Pts',(13.0885311201469,-5.,81.7942800647796));
#39713=CARTESIAN_POINT('Ctrl Pts',(13.0885311201469,5.,81.7942800647796));
#39714=CARTESIAN_POINT('Ctrl Pts',(13.0570978945104,-5.,81.7781511690216));
#39715=CARTESIAN_POINT('Ctrl Pts',(13.0570978945104,5.,81.7781511690216));
#39716=CARTESIAN_POINT('Ctrl Pts',(13.0266581777357,-5.,81.7616441734931));
#39717=CARTESIAN_POINT('Ctrl Pts',(13.0266581777357,5.,81.7616441734931));
#39718=CARTESIAN_POINT('Ctrl Pts',(12.9973652192683,-5.,81.7448717757205));
#39719=CARTESIAN_POINT('Ctrl Pts',(12.9973652192683,5.,81.7448717757205));
#39720=CARTESIAN_POINT('Ctrl Pts',(12.9694812859689,-5.,81.7280354288443));
#39721=CARTESIAN_POINT('Ctrl Pts',(12.9694812859689,5.,81.7280354288443));
#39722=CARTESIAN_POINT('Ctrl Pts',(12.9433198980207,-5.,81.7113795188064));
#39723=CARTESIAN_POINT('Ctrl Pts',(12.9433198980207,5.,81.7113795188064));
#39724=CARTESIAN_POINT('Ctrl Pts',(12.9191964772076,-5.,81.6951526607806));
#39725=CARTESIAN_POINT('Ctrl Pts',(12.9191964772076,5.,81.6951526607806));
#39726=CARTESIAN_POINT('Ctrl Pts',(12.897380292397,-5.,81.6795699036158));
#39727=CARTESIAN_POINT('Ctrl Pts',(12.897380292397,5.,81.6795699036158));
#39728=CARTESIAN_POINT('Ctrl Pts',(12.8780331013841,-5.,81.6647652712487));
#39729=CARTESIAN_POINT('Ctrl Pts',(12.8780331013841,5.,81.6647652712487));
#39730=CARTESIAN_POINT('Ctrl Pts',(12.8645838536101,-5.,81.653592684294));
#39731=CARTESIAN_POINT('Ctrl Pts',(12.8645838536101,5.,81.653592684294));
#39732=CARTESIAN_POINT('Ctrl Pts',(12.8556442551671,-5.,81.6455988328799));
#39733=CARTESIAN_POINT('Ctrl Pts',(12.8556442551671,5.,81.6455988328799));
#39734=CARTESIAN_POINT('Ctrl Pts',(12.85019346473,-5.,81.6404406139507));
#39735=CARTESIAN_POINT('Ctrl Pts',(12.85019346473,5.,81.6404406139507));
#39736=CARTESIAN_POINT('Ctrl Pts',(12.8475953086752,-5.,81.6379042610703));
#39737=CARTESIAN_POINT('Ctrl Pts',(12.8475953086752,5.,81.6379042610703));
#39738=CARTESIAN_POINT('',(12.8475953086752,0.,81.6379042610703));
#39739=CARTESIAN_POINT('Ctrl Pts',(13.7759884899248,4.8,82.0068624643054));
#39740=CARTESIAN_POINT('Ctrl Pts',(13.7759884899248,3.13333333333333,82.0068624643054));
#39741=CARTESIAN_POINT('Ctrl Pts',(13.7759884899248,1.46666666666667,82.0068624643054));
#39742=CARTESIAN_POINT('Ctrl Pts',(13.7759884899248,-1.73333333333333,82.0068624643054));
#39743=CARTESIAN_POINT('Ctrl Pts',(13.7759884899248,-3.26666666666667,82.0068624643054));
#39744=CARTESIAN_POINT('Ctrl Pts',(13.7759884899248,-4.8,82.0068624643054));
#39745=CARTESIAN_POINT('Origin',(9.31000000000031,0.,78.0000000000004));
#39746=CARTESIAN_POINT('',(11.9846612632316,0.,81.8037727491227));
#39747=CARTESIAN_POINT('',(12.5915348397961,0.,81.2945453548562));
#39748=CARTESIAN_POINT('Origin',(12.8475953086752,0.,81.6379042610703));
#39749=CARTESIAN_POINT('Ctrl Pts',(12.2783393423437,-5.,82.1155667324646));
#39750=CARTESIAN_POINT('Ctrl Pts',(12.2783393423437,5.,82.1155667324646));
#39751=CARTESIAN_POINT('Ctrl Pts',(12.2803859972687,-5.,82.1185658497385));
#39752=CARTESIAN_POINT('Ctrl Pts',(12.2803859972687,5.,82.1185658497385));
#39753=CARTESIAN_POINT('Ctrl Pts',(12.2845193314492,-5.,82.124829545725));
#39754=CARTESIAN_POINT('Ctrl Pts',(12.2845193314492,5.,82.124829545725));
#39755=CARTESIAN_POINT('Ctrl Pts',(12.2908393933303,-5.,82.1350214493006));
#39756=CARTESIAN_POINT('Ctrl Pts',(12.2908393933303,5.,82.1350214493006));
#39757=CARTESIAN_POINT('Ctrl Pts',(12.2995068062155,-5.,82.1502064721471));
#39758=CARTESIAN_POINT('Ctrl Pts',(12.2995068062155,5.,82.1502064721471));
#39759=CARTESIAN_POINT('Ctrl Pts',(12.3107269184707,-5.,82.1718305333045));
#39760=CARTESIAN_POINT('Ctrl Pts',(12.3107269184707,5.,82.1718305333045));
#39761=CARTESIAN_POINT('Ctrl Pts',(12.3222845977848,-5.,82.1960211986505));
#39762=CARTESIAN_POINT('Ctrl Pts',(12.3222845977848,5.,82.1960211986505));
#39763=CARTESIAN_POINT('Ctrl Pts',(12.334075945302,-5.,82.2225958948322));
#39764=CARTESIAN_POINT('Ctrl Pts',(12.334075945302,5.,82.2225958948322));
#39765=CARTESIAN_POINT('Ctrl Pts',(12.3459359372985,-5.,82.2512521009388));
#39766=CARTESIAN_POINT('Ctrl Pts',(12.3459359372985,5.,82.2512521009388));
#39767=CARTESIAN_POINT('Ctrl Pts',(12.3576745080383,-5.,82.2816360155831));
#39768=CARTESIAN_POINT('Ctrl Pts',(12.3576745080383,5.,82.2816360155831));
#39769=CARTESIAN_POINT('Ctrl Pts',(12.369105426554,-5.,82.3133964444896));
#39770=CARTESIAN_POINT('Ctrl Pts',(12.369105426554,5.,82.3133964444896));
#39771=CARTESIAN_POINT('Ctrl Pts',(12.3800758423883,-5.,82.3462401232546));
#39772=CARTESIAN_POINT('Ctrl Pts',(12.3800758423883,5.,82.3462401232546));
#39773=CARTESIAN_POINT('Ctrl Pts',(12.3905013816289,-5.,82.3799965609175));
#39774=CARTESIAN_POINT('Ctrl Pts',(12.3905013816289,5.,82.3799965609175));
#39775=CARTESIAN_POINT('Ctrl Pts',(12.4003550273611,-5.,82.4145988652004));
#39776=CARTESIAN_POINT('Ctrl Pts',(12.4003550273611,5.,82.4145988652004));
#39777=CARTESIAN_POINT('Ctrl Pts',(12.4096455143463,-5.,82.4500452225975));
#39778=CARTESIAN_POINT('Ctrl Pts',(12.4096455143463,5.,82.4500452225975));
#39779=CARTESIAN_POINT('Ctrl Pts',(12.418399404803,-5.,82.4863667610403));
#39780=CARTESIAN_POINT('Ctrl Pts',(12.418399404803,5.,82.4863667610403));
#39781=CARTESIAN_POINT('Ctrl Pts',(12.4266427137534,-5.,82.5235943553157));
#39782=CARTESIAN_POINT('Ctrl Pts',(12.4266427137534,5.,82.5235943553157));
#39783=CARTESIAN_POINT('Ctrl Pts',(12.4343807922091,-5.,82.5617218593056));
#39784=CARTESIAN_POINT('Ctrl Pts',(12.4343807922091,5.,82.5617218593056));
#39785=CARTESIAN_POINT('Ctrl Pts',(12.4416012317233,-5.,82.6007120754133));
#39786=CARTESIAN_POINT('Ctrl Pts',(12.4416012317233,5.,82.6007120754133));
#39787=CARTESIAN_POINT('Ctrl Pts',(12.4482802868263,-5.,82.6405090202912));
#39788=CARTESIAN_POINT('Ctrl Pts',(12.4482802868263,5.,82.6405090202912));
#39789=CARTESIAN_POINT('Ctrl Pts',(12.4543882465293,-5.,82.6810479501583));
#39790=CARTESIAN_POINT('Ctrl Pts',(12.4543882465293,5.,82.6810479501583));
#39791=CARTESIAN_POINT('Ctrl Pts',(12.4598948909969,-5.,82.7222653006607));
#39792=CARTESIAN_POINT('Ctrl Pts',(12.4598948909969,5.,82.7222653006607));
#39793=CARTESIAN_POINT('Ctrl Pts',(12.4647760534665,-5.,82.7641103639807));
#39794=CARTESIAN_POINT('Ctrl Pts',(12.4647760534665,5.,82.7641103639807));
#39795=CARTESIAN_POINT('Ctrl Pts',(12.4690154606377,-5.,82.8065481105801));
#39796=CARTESIAN_POINT('Ctrl Pts',(12.4690154606377,5.,82.8065481105801));
#39797=CARTESIAN_POINT('Ctrl Pts',(12.4726027375752,-5.,82.8495547476242));
#39798=CARTESIAN_POINT('Ctrl Pts',(12.4726027375752,5.,82.8495547476242));
#39799=CARTESIAN_POINT('Ctrl Pts',(12.4755326881847,-5.,82.8931153543989));
#39800=CARTESIAN_POINT('Ctrl Pts',(12.4755326881847,5.,82.8931153543989));
#39801=CARTESIAN_POINT('Ctrl Pts',(12.4778042390369,-5.,82.9372205785469));
#39802=CARTESIAN_POINT('Ctrl Pts',(12.4778042390369,5.,82.9372205785469));
#39803=CARTESIAN_POINT('Ctrl Pts',(12.4794196931349,-5.,82.9818637371221));
#39804=CARTESIAN_POINT('Ctrl Pts',(12.4794196931349,5.,82.9818637371221));
#39805=CARTESIAN_POINT('Ctrl Pts',(12.4803840592604,-5.,83.0270374477065));
#39806=CARTESIAN_POINT('Ctrl Pts',(12.4803840592604,5.,83.0270374477065));
#39807=CARTESIAN_POINT('Ctrl Pts',(12.4807038286021,-5.,83.072734224382));
#39808=CARTESIAN_POINT('Ctrl Pts',(12.4807038286021,5.,83.072734224382));
#39809=CARTESIAN_POINT('Ctrl Pts',(12.480385792553,-5.,83.1189472502496));
#39810=CARTESIAN_POINT('Ctrl Pts',(12.480385792553,5.,83.1189472502496));
#39811=CARTESIAN_POINT('Ctrl Pts',(12.4796259483469,-5.,83.1563262348074));
#39812=CARTESIAN_POINT('Ctrl Pts',(12.4796259483469,5.,83.1563262348074));
#39813=CARTESIAN_POINT('Ctrl Pts',(12.478773707943,-5.,83.1845886245686));
#39814=CARTESIAN_POINT('Ctrl Pts',(12.478773707943,5.,83.1845886245686));
#39815=CARTESIAN_POINT('Ctrl Pts',(12.4780802826114,-5.,83.2035314347966));
#39816=CARTESIAN_POINT('Ctrl Pts',(12.4780802826114,5.,83.2035314347966));
#39817=CARTESIAN_POINT('Ctrl Pts',(12.4777022536662,-5.,83.2130281441901));
#39818=CARTESIAN_POINT('Ctrl Pts',(12.4777022536662,5.,83.2130281441901));
#39819=CARTESIAN_POINT('Ctrl Pts',(12.4804784574569,-4.8,83.0939244547599));
#39820=CARTESIAN_POINT('Ctrl Pts',(12.4804784574569,-3.13333333333333,83.0939244547599));
#39821=CARTESIAN_POINT('Ctrl Pts',(12.4804784574569,-1.46666666666667,83.0939244547599));
#39822=CARTESIAN_POINT('Ctrl Pts',(12.4804784574569,1.73333333333333,83.0939244547599));
#39823=CARTESIAN_POINT('Ctrl Pts',(12.4804784574569,3.26666666666667,83.09392445476));
#39824=CARTESIAN_POINT('Ctrl Pts',(12.4804784574569,4.8,83.09392445476));
#39825=CARTESIAN_POINT('',(12.2783393423437,0.,82.1155667324646));
#39826=CARTESIAN_POINT('Origin',(11.9846612632316,0.,81.8037727491227));
#39827=CARTESIAN_POINT('Ctrl Pts',(10.2342691911562,-5.,84.0295710015124));
#39828=CARTESIAN_POINT('Ctrl Pts',(10.2342691911562,5.,84.0295710015124));
#39829=CARTESIAN_POINT('Ctrl Pts',(10.2278752370576,-5.,84.0225390923711));
#39830=CARTESIAN_POINT('Ctrl Pts',(10.2278752370576,5.,84.0225390923711));
#39831=CARTESIAN_POINT('Ctrl Pts',(10.2151678387374,-5.,84.0084737830622));
#39832=CARTESIAN_POINT('Ctrl Pts',(10.2151678387374,5.,84.0084737830622));
#39833=CARTESIAN_POINT('Ctrl Pts',(10.1963482707627,-5.,83.9873713459997));
#39834=CARTESIAN_POINT('Ctrl Pts',(10.1963482707627,5.,83.9873713459997));
#39835=CARTESIAN_POINT('Ctrl Pts',(10.1717394481999,-5.,83.9592258010255));
#39836=CARTESIAN_POINT('Ctrl Pts',(10.1717394481999,5.,83.9592258010255));
#39837=CARTESIAN_POINT('Ctrl Pts',(10.1417906580151,-5.,83.9240289989938));
#39838=CARTESIAN_POINT('Ctrl Pts',(10.1417906580151,5.,83.9240289989938));
#39839=CARTESIAN_POINT('Ctrl Pts',(10.1126622936843,-5.,83.8888176933897));
#39840=CARTESIAN_POINT('Ctrl Pts',(10.1126622936843,5.,83.8888176933897));
#39841=CARTESIAN_POINT('Ctrl Pts',(10.0843639395383,-5.,83.8535927408343));
#39842=CARTESIAN_POINT('Ctrl Pts',(10.0843639395383,5.,83.8535927408343));
#39843=CARTESIAN_POINT('Ctrl Pts',(10.056905379975,-5.,83.8183557034152));
#39844=CARTESIAN_POINT('Ctrl Pts',(10.056905379975,5.,83.8183557034152));
#39845=CARTESIAN_POINT('Ctrl Pts',(10.0302951972726,-5.,83.7831090168075));
#39846=CARTESIAN_POINT('Ctrl Pts',(10.0302951972726,5.,83.7831090168075));
#39847=CARTESIAN_POINT('Ctrl Pts',(10.004539451349,-5.,83.7478563201022));
#39848=CARTESIAN_POINT('Ctrl Pts',(10.004539451349,5.,83.7478563201022));
#39849=CARTESIAN_POINT('Ctrl Pts',(9.97964333148819,-5.,83.7126054676082));
#39850=CARTESIAN_POINT('Ctrl Pts',(9.97964333148819,5.,83.7126054676082));
#39851=CARTESIAN_POINT('Ctrl Pts',(9.95561244809968,-5.,83.6773712292418));
#39852=CARTESIAN_POINT('Ctrl Pts',(9.95561244809968,5.,83.6773712292418));
#39853=CARTESIAN_POINT('Ctrl Pts',(9.93245414725961,-5.,83.6421785002535));
#39854=CARTESIAN_POINT('Ctrl Pts',(9.93245414725961,5.,83.6421785002535));
#39855=CARTESIAN_POINT('Ctrl Pts',(9.91017847944887,-5.,83.607064575104));
#39856=CARTESIAN_POINT('Ctrl Pts',(9.91017847944887,5.,83.607064575104));
#39857=CARTESIAN_POINT('Ctrl Pts',(9.88879952620944,-5.,83.5720838323314));
#39858=CARTESIAN_POINT('Ctrl Pts',(9.88879952620944,5.,83.5720838323314));
#39859=CARTESIAN_POINT('Ctrl Pts',(9.86833499618459,-5.,83.537304389991));
#39860=CARTESIAN_POINT('Ctrl Pts',(9.86833499618459,5.,83.537304389991));
#39861=CARTESIAN_POINT('Ctrl Pts',(9.84880374593727,-5.,83.5027949425508));
#39862=CARTESIAN_POINT('Ctrl Pts',(9.84880374593727,5.,83.5027949425508));
#39863=CARTESIAN_POINT('Ctrl Pts',(9.83022357078563,-5.,83.4686136390358));
#39864=CARTESIAN_POINT('Ctrl Pts',(9.83022357078563,5.,83.4686136390358));
#39865=CARTESIAN_POINT('Ctrl Pts',(9.81260887546256,-5.,83.4347969504531));
#39866=CARTESIAN_POINT('Ctrl Pts',(9.81260887546256,5.,83.4347969504531));
#39867=CARTESIAN_POINT('Ctrl Pts',(9.79596770972913,-5.,83.4013461454384));
#39868=CARTESIAN_POINT('Ctrl Pts',(9.79596770972913,5.,83.4013461454384));
#39869=CARTESIAN_POINT('Ctrl Pts',(9.78030015631686,-5.,83.3682208504004));
#39870=CARTESIAN_POINT('Ctrl Pts',(9.78030015631686,5.,83.3682208504004));
#39871=CARTESIAN_POINT('Ctrl Pts',(9.76560655441585,-5.,83.3353801460973));
#39872=CARTESIAN_POINT('Ctrl Pts',(9.76560655441585,5.,83.3353801460973));
#39873=CARTESIAN_POINT('Ctrl Pts',(9.75189476093909,-5.,83.30281980716));
#39874=CARTESIAN_POINT('Ctrl Pts',(9.75189476093909,5.,83.30281980716));
#39875=CARTESIAN_POINT('Ctrl Pts',(9.73918707725655,-5.,83.270608442185));
#39876=CARTESIAN_POINT('Ctrl Pts',(9.73918707725655,5.,83.270608442185));
#39877=CARTESIAN_POINT('Ctrl Pts',(9.72752845867955,-5.,83.2389308893288));
#39878=CARTESIAN_POINT('Ctrl Pts',(9.72752845867955,5.,83.2389308893288));
#39879=CARTESIAN_POINT('Ctrl Pts',(9.71699032169307,-5.,83.2081100525341));
#39880=CARTESIAN_POINT('Ctrl Pts',(9.71699032169307,5.,83.2081100525341));
#39881=CARTESIAN_POINT('Ctrl Pts',(9.70765574843163,-5.,83.1785346691788));
#39882=CARTESIAN_POINT('Ctrl Pts',(9.70765574843163,5.,83.1785346691788));
#39883=CARTESIAN_POINT('Ctrl Pts',(9.69960655924427,-5.,83.1505979387468));
#39884=CARTESIAN_POINT('Ctrl Pts',(9.69960655924427,5.,83.1505979387468));
#39885=CARTESIAN_POINT('Ctrl Pts',(9.69291079531643,-5.,83.1246376809074));
#39886=CARTESIAN_POINT('Ctrl Pts',(9.69291079531643,5.,83.1246376809074));
#39887=CARTESIAN_POINT('Ctrl Pts',(9.6876062213894,-5.,83.1008605398683));
#39888=CARTESIAN_POINT('Ctrl Pts',(9.6876062213894,5.,83.1008605398683));
#39889=CARTESIAN_POINT('Ctrl Pts',(9.68448510032915,-5.,83.0836568318856));
#39890=CARTESIAN_POINT('Ctrl Pts',(9.68448510032915,5.,83.0836568318856));
#39891=CARTESIAN_POINT('Ctrl Pts',(9.68277531926867,-5.,83.0717869233261));
#39892=CARTESIAN_POINT('Ctrl Pts',(9.68277531926867,5.,83.0717869233261));
#39893=CARTESIAN_POINT('Ctrl Pts',(9.68191541076936,-5.,83.0643317978355));
#39894=CARTESIAN_POINT('Ctrl Pts',(9.68191541076936,5.,83.0643317978355));
#39895=CARTESIAN_POINT('Ctrl Pts',(9.68155544397255,-5.,83.0607187762934));
#39896=CARTESIAN_POINT('Ctrl Pts',(9.68155544397255,5.,83.0607187762934));
#39897=CARTESIAN_POINT('',(9.68155544397255,0.,83.0607187762934));
#39898=CARTESIAN_POINT('Ctrl Pts',(10.1555841198781,4.8,83.9401167914621));
#39899=CARTESIAN_POINT('Ctrl Pts',(10.1555841198781,3.13333333333333,83.9401167914621));
#39900=CARTESIAN_POINT('Ctrl Pts',(10.1555841198781,1.46666666666667,83.9401167914621));
#39901=CARTESIAN_POINT('Ctrl Pts',(10.1555841198781,-1.73333333333333,83.9401167914621));
#39902=CARTESIAN_POINT('Ctrl Pts',(10.1555841198781,-3.26666666666667,83.9401167914621));
#39903=CARTESIAN_POINT('Ctrl Pts',(10.1555841198781,-4.8,83.9401167914621));
#39904=CARTESIAN_POINT('Origin',(9.31,0.,78.0000000000002));
#39905=CARTESIAN_POINT('',(8.91389140472481,0.,82.6330980974667));
#39906=CARTESIAN_POINT('',(9.70610859527519,0.,82.6330980974667));
#39907=CARTESIAN_POINT('Origin',(9.68155544397255,0.,83.0607187762934));
#39908=CARTESIAN_POINT('Ctrl Pts',(8.93844455602746,-5.,83.0607187762934));
#39909=CARTESIAN_POINT('Ctrl Pts',(8.93844455602746,5.,83.0607187762934));
#39910=CARTESIAN_POINT('Ctrl Pts',(8.93808458922896,-5.,83.0643317978355));
#39911=CARTESIAN_POINT('Ctrl Pts',(8.93808458922896,5.,83.0643317978355));
#39912=CARTESIAN_POINT('Ctrl Pts',(8.93722468072689,-5.,83.0717869233258));
#39913=CARTESIAN_POINT('Ctrl Pts',(8.93722468072689,5.,83.0717869233258));
#39914=CARTESIAN_POINT('Ctrl Pts',(8.93551489966416,-5.,83.0836568318852));
#39915=CARTESIAN_POINT('Ctrl Pts',(8.93551489966416,5.,83.0836568318852));
#39916=CARTESIAN_POINT('Ctrl Pts',(8.93239377860429,-5.,83.1008605398679));
#39917=CARTESIAN_POINT('Ctrl Pts',(8.93239377860429,5.,83.1008605398679));
#39918=CARTESIAN_POINT('Ctrl Pts',(8.92708920468098,-5.,83.1246376809072));
#39919=CARTESIAN_POINT('Ctrl Pts',(8.92708920468098,5.,83.1246376809072));
#39920=CARTESIAN_POINT('Ctrl Pts',(8.92039344075711,-5.,83.1505979387469));
#39921=CARTESIAN_POINT('Ctrl Pts',(8.92039344075711,5.,83.1505979387469));
#39922=CARTESIAN_POINT('Ctrl Pts',(8.91234425157185,-5.,83.178534669179));
#39923=CARTESIAN_POINT('Ctrl Pts',(8.91234425157185,5.,83.178534669179));
#39924=CARTESIAN_POINT('Ctrl Pts',(8.90300967831031,-5.,83.2081100525344));
#39925=CARTESIAN_POINT('Ctrl Pts',(8.90300967831031,5.,83.2081100525344));
#39926=CARTESIAN_POINT('Ctrl Pts',(8.89247154132227,-5.,83.2389308893288));
#39927=CARTESIAN_POINT('Ctrl Pts',(8.89247154132227,5.,83.2389308893288));
#39928=CARTESIAN_POINT('Ctrl Pts',(8.88081292274349,-5.,83.270608442185));
#39929=CARTESIAN_POINT('Ctrl Pts',(8.88081292274349,5.,83.270608442185));
#39930=CARTESIAN_POINT('Ctrl Pts',(8.86810523906001,-5.,83.30281980716));
#39931=CARTESIAN_POINT('Ctrl Pts',(8.86810523906001,5.,83.30281980716));
#39932=CARTESIAN_POINT('Ctrl Pts',(8.85439344558332,-5.,83.3353801460974));
#39933=CARTESIAN_POINT('Ctrl Pts',(8.85439344558332,5.,83.3353801460974));
#39934=CARTESIAN_POINT('Ctrl Pts',(8.839699843683,-5.,83.3682208504006));
#39935=CARTESIAN_POINT('Ctrl Pts',(8.839699843683,5.,83.3682208504006));
#39936=CARTESIAN_POINT('Ctrl Pts',(8.82403229027133,-5.,83.4013461454385));
#39937=CARTESIAN_POINT('Ctrl Pts',(8.82403229027133,5.,83.4013461454385));
#39938=CARTESIAN_POINT('Ctrl Pts',(8.80739112453778,-5.,83.4347969504531));
#39939=CARTESIAN_POINT('Ctrl Pts',(8.80739112453778,5.,83.4347969504531));
#39940=CARTESIAN_POINT('Ctrl Pts',(8.78977642921359,-5.,83.4686136390359));
#39941=CARTESIAN_POINT('Ctrl Pts',(8.78977642921359,5.,83.4686136390359));
#39942=CARTESIAN_POINT('Ctrl Pts',(8.77119625406031,-5.,83.5027949425511));
#39943=CARTESIAN_POINT('Ctrl Pts',(8.77119625406031,5.,83.5027949425511));
#39944=CARTESIAN_POINT('Ctrl Pts',(8.75166500381164,-5.,83.5373043899916));
#39945=CARTESIAN_POINT('Ctrl Pts',(8.75166500381164,5.,83.5373043899916));
#39946=CARTESIAN_POINT('Ctrl Pts',(8.7312004737867,-5.,83.5720838323321));
#39947=CARTESIAN_POINT('Ctrl Pts',(8.7312004737867,5.,83.5720838323321));
#39948=CARTESIAN_POINT('Ctrl Pts',(8.70982152054912,-5.,83.6070645751044));
#39949=CARTESIAN_POINT('Ctrl Pts',(8.70982152054912,5.,83.6070645751044));
#39950=CARTESIAN_POINT('Ctrl Pts',(8.68754585274241,-5.,83.6421785002532));
#39951=CARTESIAN_POINT('Ctrl Pts',(8.68754585274241,5.,83.6421785002532));
#39952=CARTESIAN_POINT('Ctrl Pts',(8.66438755190743,-5.,83.6773712292402));
#39953=CARTESIAN_POINT('Ctrl Pts',(8.66438755190743,5.,83.6773712292402));
#39954=CARTESIAN_POINT('Ctrl Pts',(8.64035666852326,-5.,83.7126054676056));
#39955=CARTESIAN_POINT('Ctrl Pts',(8.64035666852326,5.,83.7126054676056));
#39956=CARTESIAN_POINT('Ctrl Pts',(8.61546054866391,-5.,83.7478563200994));
#39957=CARTESIAN_POINT('Ctrl Pts',(8.61546054866391,5.,83.7478563200994));
#39958=CARTESIAN_POINT('Ctrl Pts',(8.58970480273733,-5.,83.7831090168055));
#39959=CARTESIAN_POINT('Ctrl Pts',(8.58970480273733,5.,83.7831090168055));
#39960=CARTESIAN_POINT('Ctrl Pts',(8.5630946200268,-5.,83.8183557034149));
#39961=CARTESIAN_POINT('Ctrl Pts',(8.5630946200268,5.,83.8183557034149));
#39962=CARTESIAN_POINT('Ctrl Pts',(8.53563606045106,-5.,83.8535927408361));
#39963=CARTESIAN_POINT('Ctrl Pts',(8.53563606045106,5.,83.8535927408361));
#39964=CARTESIAN_POINT('Ctrl Pts',(8.50733770629117,-5.,83.8888176933934));
#39965=CARTESIAN_POINT('Ctrl Pts',(8.50733770629117,5.,83.8888176933934));
#39966=CARTESIAN_POINT('Ctrl Pts',(8.47820934194942,-5.,83.9240289989987));
#39967=CARTESIAN_POINT('Ctrl Pts',(8.47820934194942,5.,83.9240289989987));
#39968=CARTESIAN_POINT('Ctrl Pts',(8.44826055176156,-5.,83.9592258010304));
#39969=CARTESIAN_POINT('Ctrl Pts',(8.44826055176156,5.,83.9592258010304));
#39970=CARTESIAN_POINT('Ctrl Pts',(8.42365172920609,-5.,83.9873713460034));
#39971=CARTESIAN_POINT('Ctrl Pts',(8.42365172920609,5.,83.9873713460034));
#39972=CARTESIAN_POINT('Ctrl Pts',(8.40483216124414,-5.,84.0084737830643));
#39973=CARTESIAN_POINT('Ctrl Pts',(8.40483216124414,5.,84.0084737830643));
#39974=CARTESIAN_POINT('Ctrl Pts',(8.3921247629357,-5.,84.0225390923718));
#39975=CARTESIAN_POINT('Ctrl Pts',(8.3921247629357,5.,84.0225390923718));
#39976=CARTESIAN_POINT('Ctrl Pts',(8.38573080884383,-5.,84.0295710015124));
#39977=CARTESIAN_POINT('Ctrl Pts',(8.38573080884383,5.,84.0295710015124));
#39978=CARTESIAN_POINT('Ctrl Pts',(8.46441588009367,-4.8,83.9401167914581));
#39979=CARTESIAN_POINT('Ctrl Pts',(8.46441588009367,-3.13333333333333,83.9401167914581));
#39980=CARTESIAN_POINT('Ctrl Pts',(8.46441588009367,-1.46666666666667,83.9401167914581));
#39981=CARTESIAN_POINT('Ctrl Pts',(8.46441588009367,1.73333333333333,83.9401167914581));
#39982=CARTESIAN_POINT('Ctrl Pts',(8.46441588009368,3.26666666666667,83.9401167914581));
#39983=CARTESIAN_POINT('Ctrl Pts',(8.46441588009368,4.8,83.9401167914581));
#39984=CARTESIAN_POINT('',(8.93844455602746,0.,83.0607187762934));
#39985=CARTESIAN_POINT('Origin',(8.91389140472481,0.,82.6330980974667));
#39986=CARTESIAN_POINT('Ctrl Pts',(6.14229774633382,-5.,83.2130281441901));
#39987=CARTESIAN_POINT('Ctrl Pts',(6.14229774633382,5.,83.2130281441901));
#39988=CARTESIAN_POINT('Ctrl Pts',(6.14191971738338,-5.,83.2035314347958));
#39989=CARTESIAN_POINT('Ctrl Pts',(6.14191971738338,5.,83.2035314347958));
#39990=CARTESIAN_POINT('Ctrl Pts',(6.14122629204258,-5.,83.1845886245663));
#39991=CARTESIAN_POINT('Ctrl Pts',(6.14122629204258,5.,83.1845886245663));
#39992=CARTESIAN_POINT('Ctrl Pts',(6.14037405162884,-5.,83.1563262348033));
#39993=CARTESIAN_POINT('Ctrl Pts',(6.14037405162884,5.,83.1563262348033));
#39994=CARTESIAN_POINT('Ctrl Pts',(6.13961420741709,-5.,83.1189472502444));
#39995=CARTESIAN_POINT('Ctrl Pts',(6.13961420741709,5.,83.1189472502444));
#39996=CARTESIAN_POINT('Ctrl Pts',(6.13929617137036,-5.,83.072734224377));
#39997=CARTESIAN_POINT('Ctrl Pts',(6.13929617137036,5.,83.072734224377));
#39998=CARTESIAN_POINT('Ctrl Pts',(6.13961594072051,-5.,83.0270374477027));
#39999=CARTESIAN_POINT('Ctrl Pts',(6.13961594072051,5.,83.0270374477027));
#40000=CARTESIAN_POINT('Ctrl Pts',(6.14058030685684,-5.,82.9818637371201));
#40001=CARTESIAN_POINT('Ctrl Pts',(6.14058030685684,5.,82.9818637371201));
#40002=CARTESIAN_POINT('Ctrl Pts',(6.14219576096457,-5.,82.9372205785471));
#40003=CARTESIAN_POINT('Ctrl Pts',(6.14219576096457,5.,82.9372205785471));
#40004=CARTESIAN_POINT('Ctrl Pts',(6.14446731182308,-5.,82.893115354401));
#40005=CARTESIAN_POINT('Ctrl Pts',(6.14446731182308,5.,82.893115354401));
#40006=CARTESIAN_POINT('Ctrl Pts',(6.14739726243497,-5.,82.8495547476274));
#40007=CARTESIAN_POINT('Ctrl Pts',(6.14739726243497,5.,82.8495547476274));
#40008=CARTESIAN_POINT('Ctrl Pts',(6.15098453937128,-5.,82.8065481105834));
#40009=CARTESIAN_POINT('Ctrl Pts',(6.15098453937128,5.,82.8065481105834));
#40010=CARTESIAN_POINT('Ctrl Pts',(6.15522394653913,-5.,82.7641103639832));
#40011=CARTESIAN_POINT('Ctrl Pts',(6.15522394653913,5.,82.7641103639832));
#40012=CARTESIAN_POINT('Ctrl Pts',(6.16010510900473,-5.,82.7222653006616));
#40013=CARTESIAN_POINT('Ctrl Pts',(6.16010510900473,5.,82.7222653006616));
#40014=CARTESIAN_POINT('Ctrl Pts',(6.16561175346913,-5.,82.6810479501576));
#40015=CARTESIAN_POINT('Ctrl Pts',(6.16561175346913,5.,82.6810479501576));
#40016=CARTESIAN_POINT('Ctrl Pts',(6.17171971317045,-5.,82.6405090202891));
#40017=CARTESIAN_POINT('Ctrl Pts',(6.17171971317045,5.,82.6405090202891));
#40018=CARTESIAN_POINT('Ctrl Pts',(6.17839876827339,-5.,82.6007120754106));
#40019=CARTESIAN_POINT('Ctrl Pts',(6.17839876827339,5.,82.6007120754106));
#40020=CARTESIAN_POINT('Ctrl Pts',(6.18561920778864,-5.,82.5617218593032));
#40021=CARTESIAN_POINT('Ctrl Pts',(6.18561920778864,5.,82.5617218593032));
#40022=CARTESIAN_POINT('Ctrl Pts',(6.19335728624576,-5.,82.5235943553145));
#40023=CARTESIAN_POINT('Ctrl Pts',(6.19335728624576,5.,82.5235943553145));
#40024=CARTESIAN_POINT('Ctrl Pts',(6.20160059519734,-5.,82.4863667610406));
#40025=CARTESIAN_POINT('Ctrl Pts',(6.20160059519734,5.,82.4863667610406));
#40026=CARTESIAN_POINT('Ctrl Pts',(6.21035448565451,-5.,82.4500452225988));
#40027=CARTESIAN_POINT('Ctrl Pts',(6.21035448565451,5.,82.4500452225988));
#40028=CARTESIAN_POINT('Ctrl Pts',(6.21964497263948,-5.,82.4145988652022));
#40029=CARTESIAN_POINT('Ctrl Pts',(6.21964497263948,5.,82.4145988652022));
#40030=CARTESIAN_POINT('Ctrl Pts',(6.22949861837122,-5.,82.3799965609194));
#40031=CARTESIAN_POINT('Ctrl Pts',(6.22949861837122,5.,82.3799965609194));
#40032=CARTESIAN_POINT('Ctrl Pts',(6.23992415761144,-5.,82.3462401232558));
#40033=CARTESIAN_POINT('Ctrl Pts',(6.23992415761144,5.,82.3462401232558));
#40034=CARTESIAN_POINT('Ctrl Pts',(6.25089457344595,-5.,82.3133964444894));
#40035=CARTESIAN_POINT('Ctrl Pts',(6.25089457344595,5.,82.3133964444894));
#40036=CARTESIAN_POINT('Ctrl Pts',(6.26232549196237,-5.,82.2816360155812));
#40037=CARTESIAN_POINT('Ctrl Pts',(6.26232549196237,5.,82.2816360155812));
#40038=CARTESIAN_POINT('Ctrl Pts',(6.27406406270293,-5.,82.2512521009353));
#40039=CARTESIAN_POINT('Ctrl Pts',(6.27406406270293,5.,82.2512521009353));
#40040=CARTESIAN_POINT('Ctrl Pts',(6.28592405469946,-5.,82.2225958948289));
#40041=CARTESIAN_POINT('Ctrl Pts',(6.28592405469946,5.,82.2225958948289));
#40042=CARTESIAN_POINT('Ctrl Pts',(6.29771540221578,-5.,82.1960211986491));
#40043=CARTESIAN_POINT('Ctrl Pts',(6.29771540221578,5.,82.1960211986491));
#40044=CARTESIAN_POINT('Ctrl Pts',(6.30927308152824,-5.,82.1718305333071));
#40045=CARTESIAN_POINT('Ctrl Pts',(6.30927308152824,5.,82.1718305333071));
#40046=CARTESIAN_POINT('Ctrl Pts',(6.32049319378186,-5.,82.1502064721534));
#40047=CARTESIAN_POINT('Ctrl Pts',(6.32049319378186,5.,82.1502064721534));
#40048=CARTESIAN_POINT('Ctrl Pts',(6.32916060666696,-5.,82.1350214493075));
#40049=CARTESIAN_POINT('Ctrl Pts',(6.32916060666696,5.,82.1350214493075));
#40050=CARTESIAN_POINT('Ctrl Pts',(6.33548066854901,-5.,82.1248295457296));
#40051=CARTESIAN_POINT('Ctrl Pts',(6.33548066854901,5.,82.1248295457296));
#40052=CARTESIAN_POINT('Ctrl Pts',(6.33961400273064,-5.,82.1185658497402));
#40053=CARTESIAN_POINT('Ctrl Pts',(6.33961400273064,5.,82.1185658497402));
#40054=CARTESIAN_POINT('Ctrl Pts',(6.34166065765632,-5.,82.1155667324646));
#40055=CARTESIAN_POINT('Ctrl Pts',(6.34166065765632,5.,82.1155667324646));
#40056=CARTESIAN_POINT('',(6.34166065765632,0.,82.1155667324646));
#40057=CARTESIAN_POINT('Ctrl Pts',(6.13952154251532,4.8,83.0939244547427));
#40058=CARTESIAN_POINT('Ctrl Pts',(6.13952154251532,3.13333333333333,83.0939244547427));
#40059=CARTESIAN_POINT('Ctrl Pts',(6.13952154251532,1.46666666666667,83.0939244547427));
#40060=CARTESIAN_POINT('Ctrl Pts',(6.13952154251532,-1.73333333333333,83.0939244547427));
#40061=CARTESIAN_POINT('Ctrl Pts',(6.13952154251532,-3.26666666666667,83.0939244547427));
#40062=CARTESIAN_POINT('Ctrl Pts',(6.13952154251532,-4.8,83.0939244547427));
#40063=CARTESIAN_POINT('Origin',(9.3100000000004,0.,77.9999999999995));
#40064=CARTESIAN_POINT('',(6.02846516020393,0.,81.2945453548562));
#40065=CARTESIAN_POINT('',(6.63533873676839,0.,81.8037727491227));
#40066=CARTESIAN_POINT('Origin',(6.34166065765632,0.,82.1155667324646));
#40067=CARTESIAN_POINT('Ctrl Pts',(5.77240469132478,-5.,81.6379042610703));
#40068=CARTESIAN_POINT('Ctrl Pts',(5.77240469132478,5.,81.6379042610703));
#40069=CARTESIAN_POINT('Ctrl Pts',(5.76980653526848,-5.,81.640440613956));
#40070=CARTESIAN_POINT('Ctrl Pts',(5.76980653526848,5.,81.640440613956));
#40071=CARTESIAN_POINT('Ctrl Pts',(5.76435574482894,-5.,81.6455988328939));
#40072=CARTESIAN_POINT('Ctrl Pts',(5.76435574482894,5.,81.6455988328939));
#40073=CARTESIAN_POINT('Ctrl Pts',(5.75541614638387,-5.,81.6535926843148));
#40074=CARTESIAN_POINT('Ctrl Pts',(5.75541614638387,5.,81.6535926843148));
#40075=CARTESIAN_POINT('Ctrl Pts',(5.74196689861022,-5.,81.664765271268));
#40076=CARTESIAN_POINT('Ctrl Pts',(5.74196689861022,5.,81.664765271268));
#40077=CARTESIAN_POINT('Ctrl Pts',(5.7226197076007,-5.,81.6795699036238));
#40078=CARTESIAN_POINT('Ctrl Pts',(5.7226197076007,5.,81.6795699036238));
#40079=CARTESIAN_POINT('Ctrl Pts',(5.70080352279367,-5.,81.6951526607764));
#40080=CARTESIAN_POINT('Ctrl Pts',(5.70080352279367,5.,81.6951526607764));
#40081=CARTESIAN_POINT('Ctrl Pts',(5.67668010198233,-5.,81.7113795187953));
#40082=CARTESIAN_POINT('Ctrl Pts',(5.67668010198233,5.,81.7113795187953));
#40083=CARTESIAN_POINT('Ctrl Pts',(5.65051871403411,-5.,81.7280354288328));
#40084=CARTESIAN_POINT('Ctrl Pts',(5.65051871403411,5.,81.7280354288328));
#40085=CARTESIAN_POINT('Ctrl Pts',(5.6226347807333,-5.,81.7448717757137));
#40086=CARTESIAN_POINT('Ctrl Pts',(5.6226347807333,5.,81.7448717757137));
#40087=CARTESIAN_POINT('Ctrl Pts',(5.59334182226431,-5.,81.7616441734925));
#40088=CARTESIAN_POINT('Ctrl Pts',(5.59334182226431,5.,81.7616441734925));
#40089=CARTESIAN_POINT('Ctrl Pts',(5.56290210548887,-5.,81.7781511690255));
#40090=CARTESIAN_POINT('Ctrl Pts',(5.56290210548887,5.,81.7781511690255));
#40091=CARTESIAN_POINT('Ctrl Pts',(5.53146887985245,-5.,81.7942800647846));
#40092=CARTESIAN_POINT('Ctrl Pts',(5.53146887985245,5.,81.7942800647846));
#40093=CARTESIAN_POINT('Ctrl Pts',(5.49910332995,-5.,81.8099926385801));
#40094=CARTESIAN_POINT('Ctrl Pts',(5.49910332995,5.,81.8099926385801));
#40095=CARTESIAN_POINT('Ctrl Pts',(5.46580875850822,-5.,81.8252971775594));
#40096=CARTESIAN_POINT('Ctrl Pts',(5.46580875850822,5.,81.8252971775594));
#40097=CARTESIAN_POINT('Ctrl Pts',(5.43155912297688,-5.,81.8402252457094));
#40098=CARTESIAN_POINT('Ctrl Pts',(5.43155912297688,5.,81.8402252457094));
#40099=CARTESIAN_POINT('Ctrl Pts',(5.39632853508549,-5.,81.8548078241758));
#40100=CARTESIAN_POINT('Ctrl Pts',(5.39632853508549,5.,81.8548078241758));
#40101=CARTESIAN_POINT('Ctrl Pts',(5.36012397677274,-5.,81.8690491154153));
#40102=CARTESIAN_POINT('Ctrl Pts',(5.36012397677274,5.,81.8690491154153));
#40103=CARTESIAN_POINT('Ctrl Pts',(5.32297992581797,-5.,81.8829304401999));
#40104=CARTESIAN_POINT('Ctrl Pts',(5.32297992581797,5.,81.8829304401999));
#40105=CARTESIAN_POINT('Ctrl Pts',(5.28494739170169,-5.,81.896418692403));
#40106=CARTESIAN_POINT('Ctrl Pts',(5.28494739170169,5.,81.896418692403));
#40107=CARTESIAN_POINT('Ctrl Pts',(5.24608497534447,-5.,81.9094733697741));
#40108=CARTESIAN_POINT('Ctrl Pts',(5.24608497534447,5.,81.9094733697741));
#40109=CARTESIAN_POINT('Ctrl Pts',(5.20645002779738,-5.,81.9220536737517));
#40110=CARTESIAN_POINT('Ctrl Pts',(5.20645002779738,5.,81.9220536737517));
#40111=CARTESIAN_POINT('Ctrl Pts',(5.16608828999526,-5.,81.934126999398));
#40112=CARTESIAN_POINT('Ctrl Pts',(5.16608828999526,5.,81.934126999398));
#40113=CARTESIAN_POINT('Ctrl Pts',(5.12503143346544,-5.,81.9456712378206));
#40114=CARTESIAN_POINT('Ctrl Pts',(5.12503143346544,5.,81.9456712378206));
#40115=CARTESIAN_POINT('Ctrl Pts',(5.08330108798129,-5.,81.956672040115));
#40116=CARTESIAN_POINT('Ctrl Pts',(5.08330108798129,5.,81.956672040115));
#40117=CARTESIAN_POINT('Ctrl Pts',(5.04091104528035,-5.,81.9671216981684));
#40118=CARTESIAN_POINT('Ctrl Pts',(5.04091104528035,5.,81.9671216981684));
#40119=CARTESIAN_POINT('Ctrl Pts',(4.99787032923518,-5.,81.9770175308375));
#40120=CARTESIAN_POINT('Ctrl Pts',(4.99787032923518,5.,81.9770175308375));
#40121=CARTESIAN_POINT('Ctrl Pts',(4.9541859211769,-5.,81.986360645658));
#40122=CARTESIAN_POINT('Ctrl Pts',(4.9541859211769,5.,81.986360645658));
#40123=CARTESIAN_POINT('Ctrl Pts',(4.90986596114179,-5.,81.9951546933809));
#40124=CARTESIAN_POINT('Ctrl Pts',(4.90986596114179,5.,81.9951546933809));
#40125=CARTESIAN_POINT('Ctrl Pts',(4.86491894851597,-5.,82.0034047666743));
#40126=CARTESIAN_POINT('Ctrl Pts',(4.86491894851597,5.,82.0034047666743));
#40127=CARTESIAN_POINT('Ctrl Pts',(4.81935277596149,-5.,82.0111163700251));
#40128=CARTESIAN_POINT('Ctrl Pts',(4.81935277596149,5.,82.0111163700251));
#40129=CARTESIAN_POINT('Ctrl Pts',(4.78240971662817,-5.,82.01685886213));
#40130=CARTESIAN_POINT('Ctrl Pts',(4.78240971662817,5.,82.01685886213));
#40131=CARTESIAN_POINT('Ctrl Pts',(4.75442870611591,-5.,82.0209272816843));
#40132=CARTESIAN_POINT('Ctrl Pts',(4.75442870611591,5.,82.0209272816843));
#40133=CARTESIAN_POINT('Ctrl Pts',(4.7356532677282,-5.,82.0235337755483));
#40134=CARTESIAN_POINT('Ctrl Pts',(4.7356532677282,5.,82.0235337755483));
#40135=CARTESIAN_POINT('Ctrl Pts',(4.72623519067131,-5.,82.0248105760097));
#40136=CARTESIAN_POINT('Ctrl Pts',(4.72623519067131,5.,82.0248105760097));
#40137=CARTESIAN_POINT('Ctrl Pts',(4.84401151007851,-4.8,82.006862464309));
#40138=CARTESIAN_POINT('Ctrl Pts',(4.84401151007851,-3.13333333333333,82.006862464309));
#40139=CARTESIAN_POINT('Ctrl Pts',(4.84401151007851,-1.46666666666667,82.006862464309));
#40140=CARTESIAN_POINT('Ctrl Pts',(4.84401151007851,1.73333333333333,82.006862464309));
#40141=CARTESIAN_POINT('Ctrl Pts',(4.84401151007851,3.26666666666667,82.0068624643091));
#40142=CARTESIAN_POINT('Ctrl Pts',(4.84401151007851,4.8,82.0068624643091));
#40143=CARTESIAN_POINT('',(5.77240469132478,0.,81.6379042610703));
#40144=CARTESIAN_POINT('Origin',(6.02846516020393,0.,81.2945453548562));
#40145=CARTESIAN_POINT('Ctrl Pts',(3.53252939109094,-5.,79.9572514818469));
#40146=CARTESIAN_POINT('Ctrl Pts',(3.53252939109094,5.,79.9572514818469));
#40147=CARTESIAN_POINT('Ctrl Pts',(3.53834417123336,-5.,79.9497335880616));
#40148=CARTESIAN_POINT('Ctrl Pts',(3.53834417123336,5.,79.9497335880616));
#40149=CARTESIAN_POINT('Ctrl Pts',(3.54998918029107,-5.,79.9347768283301));
#40150=CARTESIAN_POINT('Ctrl Pts',(3.54998918029107,5.,79.9347768283301));
#40151=CARTESIAN_POINT('Ctrl Pts',(3.56750304019465,-5.,79.9125787721238));
#40152=CARTESIAN_POINT('Ctrl Pts',(3.56750304019465,5.,79.9125787721238));
#40153=CARTESIAN_POINT('Ctrl Pts',(3.59094771388259,-5.,79.8834563902682));
#40154=CARTESIAN_POINT('Ctrl Pts',(3.59094771388259,5.,79.8834563902682));
#40155=CARTESIAN_POINT('Ctrl Pts',(3.62040924457587,-5.,79.8478507289727));
#40156=CARTESIAN_POINT('Ctrl Pts',(3.62040924457587,5.,79.8478507289727));
#40157=CARTESIAN_POINT('Ctrl Pts',(3.65002752397834,-5.,79.8130505109097));
#40158=CARTESIAN_POINT('Ctrl Pts',(3.65002752397834,5.,79.8130505109097));
#40159=CARTESIAN_POINT('Ctrl Pts',(3.67980337276931,-5.,79.7790653235472));
#40160=CARTESIAN_POINT('Ctrl Pts',(3.67980337276931,5.,79.7790653235472));
#40161=CARTESIAN_POINT('Ctrl Pts',(3.70973695162199,-5.,79.7459050738843));
#40162=CARTESIAN_POINT('Ctrl Pts',(3.70973695162199,5.,79.7459050738843));
#40163=CARTESIAN_POINT('Ctrl Pts',(3.73982735215234,-5.,79.7135786367618));
#40164=CARTESIAN_POINT('Ctrl Pts',(3.73982735215234,5.,79.7135786367618));
#40165=CARTESIAN_POINT('Ctrl Pts',(3.77007204284678,-5.,79.6820926119545));
#40166=CARTESIAN_POINT('Ctrl Pts',(3.77007204284678,5.,79.6820926119545));
#40167=CARTESIAN_POINT('Ctrl Pts',(3.80046418983303,-5.,79.6514534737968));
#40168=CARTESIAN_POINT('Ctrl Pts',(3.80046418983303,5.,79.6514534737968));
#40169=CARTESIAN_POINT('Ctrl Pts',(3.83099022182597,-5.,79.6216693122348));
#40170=CARTESIAN_POINT('Ctrl Pts',(3.83099022182597,5.,79.6216693122348));
#40171=CARTESIAN_POINT('Ctrl Pts',(3.86162689742956,-5.,79.5927516847587));
#40172=CARTESIAN_POINT('Ctrl Pts',(3.86162689742956,5.,79.5927516847587));
#40173=CARTESIAN_POINT('Ctrl Pts',(3.89233923402316,-5.,79.5647169652776));
#40174=CARTESIAN_POINT('Ctrl Pts',(3.89233923402316,5.,79.5647169652776));
#40175=CARTESIAN_POINT('Ctrl Pts',(3.92307612443792,-5.,79.5375884641383));
#40176=CARTESIAN_POINT('Ctrl Pts',(3.92307612443792,5.,79.5375884641383));
#40177=CARTESIAN_POINT('Ctrl Pts',(3.95377356055667,-5.,79.5113954495259));
#40178=CARTESIAN_POINT('Ctrl Pts',(3.95377356055667,5.,79.5113954495259));
#40179=CARTESIAN_POINT('Ctrl Pts',(3.9843671659396,-5.,79.4861684201978));
#40180=CARTESIAN_POINT('Ctrl Pts',(3.9843671659396,5.,79.4861684201978));
#40181=CARTESIAN_POINT('Ctrl Pts',(4.01480276509681,-5.,79.4619349985923));
#40182=CARTESIAN_POINT('Ctrl Pts',(4.01480276509681,5.,79.4619349985923));
#40183=CARTESIAN_POINT('Ctrl Pts',(4.04504694245072,-5.,79.4387157037247));
#40184=CARTESIAN_POINT('Ctrl Pts',(4.04504694245072,5.,79.4387157037247));
#40185=CARTESIAN_POINT('Ctrl Pts',(4.07509984646481,-5.,79.4165186833579));
#40186=CARTESIAN_POINT('Ctrl Pts',(4.07509984646481,5.,79.4165186833579));
#40187=CARTESIAN_POINT('Ctrl Pts',(4.10500125173415,-5.,79.3953370081669));
#40188=CARTESIAN_POINT('Ctrl Pts',(4.10500125173415,5.,79.3953370081669));
#40189=CARTESIAN_POINT('Ctrl Pts',(4.13479151474939,-5.,79.3751639066383));
#40190=CARTESIAN_POINT('Ctrl Pts',(4.13479151474939,5.,79.3751639066383));
#40191=CARTESIAN_POINT('Ctrl Pts',(4.16447616102922,-5.,79.3560063825947));
#40192=CARTESIAN_POINT('Ctrl Pts',(4.16447616102922,5.,79.3560063825947));
#40193=CARTESIAN_POINT('Ctrl Pts',(4.19399149688981,-5.,79.3378983123566));
#40194=CARTESIAN_POINT('Ctrl Pts',(4.19399149688981,5.,79.3378983123566));
#40195=CARTESIAN_POINT('Ctrl Pts',(4.22316329868624,-5.,79.3209160650712));
#40196=CARTESIAN_POINT('Ctrl Pts',(4.22316329868624,5.,79.3209160650712));
#40197=CARTESIAN_POINT('Ctrl Pts',(4.25168596944548,-5.,79.3051860439254));
#40198=CARTESIAN_POINT('Ctrl Pts',(4.25168596944548,5.,79.3051860439254));
#40199=CARTESIAN_POINT('Ctrl Pts',(4.27919110463568,-5.,79.290857572383));
#40200=CARTESIAN_POINT('Ctrl Pts',(4.27919110463568,5.,79.290857572383));
#40201=CARTESIAN_POINT('Ctrl Pts',(4.30530568630548,-5.,79.2780795061304));
#40202=CARTESIAN_POINT('Ctrl Pts',(4.30530568630548,5.,79.2780795061304));
#40203=CARTESIAN_POINT('Ctrl Pts',(4.32970884225655,-5.,79.2669775144253));
#40204=CARTESIAN_POINT('Ctrl Pts',(4.32970884225655,5.,79.2669775144253));
#40205=CARTESIAN_POINT('Ctrl Pts',(4.35220362546771,-5.,79.2576246716733));
#40206=CARTESIAN_POINT('Ctrl Pts',(4.35220362546771,5.,79.2576246716733));
#40207=CARTESIAN_POINT('Ctrl Pts',(4.36860399348142,-5.,79.2515635749137));
#40208=CARTESIAN_POINT('Ctrl Pts',(4.36860399348142,5.,79.2515635749137));
#40209=CARTESIAN_POINT('Ctrl Pts',(4.37999667111292,-5.,79.2478185812853));
#40210=CARTESIAN_POINT('Ctrl Pts',(4.37999667111292,5.,79.2478185812853));
#40211=CARTESIAN_POINT('Ctrl Pts',(4.3871892149765,-5.,79.2456771677804));
#40212=CARTESIAN_POINT('Ctrl Pts',(4.3871892149765,5.,79.2456771677804));
#40213=CARTESIAN_POINT('Ctrl Pts',(4.39068483903982,-5.,79.2446952750862));
#40214=CARTESIAN_POINT('Ctrl Pts',(4.39068483903982,5.,79.2446952750862));
#40215=CARTESIAN_POINT('',(4.39068483903982,0.,79.2446952750862));
#40216=CARTESIAN_POINT('Ctrl Pts',(3.60696107140889,4.8,79.864228252917));
#40217=CARTESIAN_POINT('Ctrl Pts',(3.60696107140889,3.13333333333333,79.864228252917));
#40218=CARTESIAN_POINT('Ctrl Pts',(3.60696107140889,1.46666666666667,79.864228252917));
#40219=CARTESIAN_POINT('Ctrl Pts',(3.60696107140889,-1.73333333333333,79.864228252917));
#40220=CARTESIAN_POINT('Ctrl Pts',(3.60696107140887,-3.26666666666667,79.8642282529171));
#40221=CARTESIAN_POINT('Ctrl Pts',(3.60696107140887,-4.8,79.8642282529171));
#40222=CARTESIAN_POINT('Origin',(9.31000000000016,0.,78.));
#40223=CARTESIAN_POINT('',(4.67850553742098,0.,78.4144382259154));
#40224=CARTESIAN_POINT('',(4.81607260887647,0.,79.194619857239));
#40225=CARTESIAN_POINT('Origin',(4.39068483903982,0.,79.2446952750862));
#40226=CARTESIAN_POINT('Ctrl Pts',(4.2616449875437,-5.,78.5128739112901));
#40227=CARTESIAN_POINT('Ctrl Pts',(4.2616449875437,5.,78.5128739112901));
#40228=CARTESIAN_POINT('Ctrl Pts',(4.25802434832344,-5.,78.5131468077951));
#40229=CARTESIAN_POINT('Ctrl Pts',(4.25802434832344,5.,78.5131468077951));
#40230=CARTESIAN_POINT('Ctrl Pts',(4.25053316137154,-5.,78.5135945321785));
#40231=CARTESIAN_POINT('Ctrl Pts',(4.25053316137154,5.,78.5135945321785));
#40232=CARTESIAN_POINT('Ctrl Pts',(4.23854668300885,-5.,78.5139719145122));
#40233=CARTESIAN_POINT('Ctrl Pts',(4.23854668300885,5.,78.5139719145122));
#40234=CARTESIAN_POINT('Ctrl Pts',(4.22106236102646,-5.,78.5138856028362));
#40235=CARTESIAN_POINT('Ctrl Pts',(4.22106236102646,5.,78.5138856028362));
#40236=CARTESIAN_POINT('Ctrl Pts',(4.19672531862463,-5.,78.5127904745385));
#40237=CARTESIAN_POINT('Ctrl Pts',(4.19672531862463,5.,78.5127904745385));
#40238=CARTESIAN_POINT('Ctrl Pts',(4.16999674826607,-5.,78.510704385798));
#40239=CARTESIAN_POINT('Ctrl Pts',(4.16999674826607,5.,78.510704385798));
#40240=CARTESIAN_POINT('Ctrl Pts',(4.14108671252852,-5.,78.5076286442226));
#40241=CARTESIAN_POINT('Ctrl Pts',(4.14108671252852,5.,78.5076286442226));
#40242=CARTESIAN_POINT('Ctrl Pts',(4.110339714066,-5.,78.5035715955273));
#40243=CARTESIAN_POINT('Ctrl Pts',(4.110339714066,5.,78.5035715955273));
#40244=CARTESIAN_POINT('Ctrl Pts',(4.07815718673905,-5.,78.4985455386556));
#40245=CARTESIAN_POINT('Ctrl Pts',(4.07815718673905,5.,78.4985455386556));
#40246=CARTESIAN_POINT('Ctrl Pts',(4.04493638920224,-5.,78.4925647900071));
#40247=CARTESIAN_POINT('Ctrl Pts',(4.04493638920224,5.,78.4925647900071));
#40248=CARTESIAN_POINT('Ctrl Pts',(4.01100772111375,-5.,78.4856436094149));
#40249=CARTESIAN_POINT('Ctrl Pts',(4.01100772111375,5.,78.4856436094149));
#40250=CARTESIAN_POINT('Ctrl Pts',(3.97656101893434,-5.,78.477794172411));
#40251=CARTESIAN_POINT('Ctrl Pts',(3.97656101893434,5.,78.477794172411));
#40252=CARTESIAN_POINT('Ctrl Pts',(3.94166772153227,-5.,78.4690265277979));
#40253=CARTESIAN_POINT('Ctrl Pts',(3.94166772153227,5.,78.4690265277979));
#40254=CARTESIAN_POINT('Ctrl Pts',(3.906325032066,-5.,78.4593491468487));
#40255=CARTESIAN_POINT('Ctrl Pts',(3.906325032066,5.,78.4593491468487));
#40256=CARTESIAN_POINT('Ctrl Pts',(3.87049271184418,-5.,78.448769469149));
#40257=CARTESIAN_POINT('Ctrl Pts',(3.87049271184418,5.,78.448769469149));
#40258=CARTESIAN_POINT('Ctrl Pts',(3.83413101500406,-5.,78.4372945869717));
#40259=CARTESIAN_POINT('Ctrl Pts',(3.83413101500406,5.,78.4372945869717));
#40260=CARTESIAN_POINT('Ctrl Pts',(3.79724258873491,-5.,78.4249322074894));
#40261=CARTESIAN_POINT('Ctrl Pts',(3.79724258873491,5.,78.4249322074894));
#40262=CARTESIAN_POINT('Ctrl Pts',(3.75986585132571,-5.,78.4116901834742));
#40263=CARTESIAN_POINT('Ctrl Pts',(3.75986585132571,5.,78.4116901834742));
#40264=CARTESIAN_POINT('Ctrl Pts',(3.72206115851568,-5.,78.3975759424256));
#40265=CARTESIAN_POINT('Ctrl Pts',(3.72206115851568,5.,78.3975759424256));
#40266=CARTESIAN_POINT('Ctrl Pts',(3.68389943556036,-5.,78.3825961257671));
#40267=CARTESIAN_POINT('Ctrl Pts',(3.68389943556036,5.,78.3825961257671));
#40268=CARTESIAN_POINT('Ctrl Pts',(3.64545084072423,-5.,78.3667563445328));
#40269=CARTESIAN_POINT('Ctrl Pts',(3.64545084072423,5.,78.3667563445328));
#40270=CARTESIAN_POINT('Ctrl Pts',(3.60677137164415,-5.,78.3500610235961));
#40271=CARTESIAN_POINT('Ctrl Pts',(3.60677137164415,5.,78.3500610235961));
#40272=CARTESIAN_POINT('Ctrl Pts',(3.56789950143576,-5.,78.3325135846256));
#40273=CARTESIAN_POINT('Ctrl Pts',(3.56789950143576,5.,78.3325135846256));
#40274=CARTESIAN_POINT('Ctrl Pts',(3.52886102276017,-5.,78.31411693907));
#40275=CARTESIAN_POINT('Ctrl Pts',(3.52886102276017,5.,78.31411693907));
#40276=CARTESIAN_POINT('Ctrl Pts',(3.48967145537698,-5.,78.2948740473282));
#40277=CARTESIAN_POINT('Ctrl Pts',(3.48967145537698,5.,78.2948740473282));
#40278=CARTESIAN_POINT('Ctrl Pts',(3.45033943537775,-5.,78.2747886559578));
#40279=CARTESIAN_POINT('Ctrl Pts',(3.45033943537775,5.,78.2747886559578));
#40280=CARTESIAN_POINT('Ctrl Pts',(3.41086959886365,-5.,78.2538661008949));
#40281=CARTESIAN_POINT('Ctrl Pts',(3.41086959886365,5.,78.2538661008949));
#40282=CARTESIAN_POINT('Ctrl Pts',(3.37126583481318,-5.,78.2321144110957));
#40283=CARTESIAN_POINT('Ctrl Pts',(3.37126583481318,5.,78.2321144110957));
#40284=CARTESIAN_POINT('Ctrl Pts',(3.33153138063971,-5.,78.2095429510755));
#40285=CARTESIAN_POINT('Ctrl Pts',(3.33153138063971,5.,78.2095429510755));
#40286=CARTESIAN_POINT('Ctrl Pts',(3.29166874426803,-5.,78.1861610108276));
#40287=CARTESIAN_POINT('Ctrl Pts',(3.29166874426803,5.,78.1861610108276));
#40288=CARTESIAN_POINT('Ctrl Pts',(3.25967751619637,-5.,78.1668134742004));
#40289=CARTESIAN_POINT('Ctrl Pts',(3.25967751619637,5.,78.1668134742004));
#40290=CARTESIAN_POINT('Ctrl Pts',(3.23562768892866,-5.,78.1519442175444));
#40291=CARTESIAN_POINT('Ctrl Pts',(3.23562768892866,5.,78.1519442175444));
#40292=CARTESIAN_POINT('Ctrl Pts',(3.21956944675078,-5.,78.1418722885375));
#40293=CARTESIAN_POINT('Ctrl Pts',(3.21956944675078,5.,78.1418722885375));
#40294=CARTESIAN_POINT('Ctrl Pts',(3.21153406965502,-5.,78.1367965512051));
#40295=CARTESIAN_POINT('Ctrl Pts',(3.21153406965502,5.,78.1367965512051));
#40296=CARTESIAN_POINT('Ctrl Pts',(3.31329278848646,-4.8,78.1987526588035));
#40297=CARTESIAN_POINT('Ctrl Pts',(3.31329278848646,-3.13333333333333,78.1987526588035));
#40298=CARTESIAN_POINT('Ctrl Pts',(3.31329278848646,-1.46666666666667,78.1987526588035));
#40299=CARTESIAN_POINT('Ctrl Pts',(3.31329278848646,1.73333333333333,78.1987526588035));
#40300=CARTESIAN_POINT('Ctrl Pts',(3.31329278848646,3.26666666666667,78.1987526588035));
#40301=CARTESIAN_POINT('Ctrl Pts',(3.31329278848646,4.8,78.1987526588035));
#40302=CARTESIAN_POINT('',(4.2616449875437,0.,78.5128739112901));
#40303=CARTESIAN_POINT('Origin',(4.67850553742098,0.,78.4144382259154));
#40304=CARTESIAN_POINT('Origin',(9.31,0.,78.));
#40305=CARTESIAN_POINT('Origin',(9.31,0.,78.));
#40306=CARTESIAN_POINT('Origin',(9.31,0.,78.));
#40307=CARTESIAN_POINT('Origin',(9.31,0.,78.));
#40308=CARTESIAN_POINT('Origin',(9.31,0.,78.));
#40309=CARTESIAN_POINT('Origin',(9.31,0.,78.));
#40310=CARTESIAN_POINT('Origin',(9.31,0.,78.));
#40311=CARTESIAN_POINT('Origin',(9.31,0.,78.));
#40312=CARTESIAN_POINT('Origin',(9.31,0.,78.));
#40313=CARTESIAN_POINT('Origin',(9.31,0.,78.));
#40314=CARTESIAN_POINT('Origin',(9.31,0.,78.));
#40315=CARTESIAN_POINT('Origin',(9.31,0.,78.));
#40316=CARTESIAN_POINT('Origin',(9.31,0.,78.));
#40317=CARTESIAN_POINT('Origin',(9.31,0.,78.));
#40318=CARTESIAN_POINT('Origin',(9.31,0.,78.));
#40319=CARTESIAN_POINT('Origin',(9.31,0.,78.));
#40320=CARTESIAN_POINT('Origin',(9.31,0.,78.));
#40321=CARTESIAN_POINT('Origin',(9.31,0.,78.));
#40322=CARTESIAN_POINT('',(0.,0.,0.));
#40323=CARTESIAN_POINT('Origin',(0.,0.,57.95));
#40324=CARTESIAN_POINT('',(-1.18823416249667,3.04042717342579E-5,56.1580381236952));
#40325=CARTESIAN_POINT('',(-1.1882111814849,2.07922408733904E-5,56.1155118763048));
#40326=CARTESIAN_POINT('',(-1.188225,-1.45515594291686E-16,57.95));
#40327=CARTESIAN_POINT('',(0.511859986942129,1.07234629461565,56.061775));
#40328=CARTESIAN_POINT('Ctrl Pts',(-1.18823416249667,3.04042717342579E-5,
56.1580381236952));
#40329=CARTESIAN_POINT('Ctrl Pts',(-1.18827861610379,0.0433316730233904,
56.1562980870114));
#40330=CARTESIAN_POINT('Ctrl Pts',(-1.18595724154989,0.0866281961938818,
56.1545580503277));
#40331=CARTESIAN_POINT('Ctrl Pts',(-1.18123364237345,0.129661025825523,
56.1528180136439));
#40332=CARTESIAN_POINT('Ctrl Pts',(-1.15971967143524,0.325657132078954,
56.1448928918782));
#40333=CARTESIAN_POINT('Ctrl Pts',(-1.08837365745739,0.516183147128608,
56.1369677701125));
#40334=CARTESIAN_POINT('Ctrl Pts',(-0.975859421229326,0.678102705033355,
56.1290426483468));
#40335=CARTESIAN_POINT('Ctrl Pts',(-0.863345185001266,0.840022262938101,
56.121117526581));
#40336=CARTESIAN_POINT('Ctrl Pts',(-0.709662726523,0.973335363697939,56.1131924048153));
#40337=CARTESIAN_POINT('Ctrl Pts',(-0.5334751176618,1.06185197282687,56.1052672830496));
#40338=CARTESIAN_POINT('Ctrl Pts',(-0.357287508800601,1.15036858195579,
56.0973421612839));
#40339=CARTESIAN_POINT('Ctrl Pts',(-0.158594749556469,1.19408869945381,
56.0894170395182));
#40340=CARTESIAN_POINT('Ctrl Pts',(0.0384754792288307,1.18770519465287,
56.0814919177524));
#40341=CARTESIAN_POINT('Ctrl Pts',(0.201905880564523,1.18241135215836,56.074919611835));
#40342=CARTESIAN_POINT('Ctrl Pts',(0.364220404424889,1.14265929456453,56.0683473059175));
#40343=CARTESIAN_POINT('Ctrl Pts',(0.511881162716727,1.07235883428017,56.061775));
#40344=CARTESIAN_POINT('',(-0.511838811167444,1.07233375495118,56.061775));
#40345=CARTESIAN_POINT('Origin',(0.,0.,56.061775));
#40346=CARTESIAN_POINT('Ctrl Pts',(-0.511838811167444,1.07233375495118,
56.061775));
#40347=CARTESIAN_POINT('Ctrl Pts',(-0.689828373128891,0.987377028210158,
56.0697001217657));
#40348=CARTESIAN_POINT('Ctrl Pts',(-0.846158719658857,0.857268871760102,
56.0776252435314));
#40349=CARTESIAN_POINT('Ctrl Pts',(-0.961924008494834,0.697685904838996,
56.0855503652972));
#40350=CARTESIAN_POINT('Ctrl Pts',(-1.07768929733081,0.538102937917886,
56.0934754870629));
#40351=CARTESIAN_POINT('Ctrl Pts',(-1.1528895284728,0.349045160525724,56.1014006088286));
#40352=CARTESIAN_POINT('Ctrl Pts',(-1.17836884940845,0.153522240919442,
56.1093257305943));
#40353=CARTESIAN_POINT('Ctrl Pts',(-1.18499834973128,0.102648857679571,
56.1113877791645));
#40354=CARTESIAN_POINT('Ctrl Pts',(-1.18826176594027,0.0513377871083471,
56.1134498277346));
#40355=CARTESIAN_POINT('Ctrl Pts',(-1.1882111814849,2.07922408733904E-5,
56.1155118763048));
#40356=CARTESIAN_POINT('Origin',(0.,0.,57.95));
#40357=CARTESIAN_POINT('',(-1.18826932065667,-2.69461188108222E-5,56.4580381236952));
#40358=CARTESIAN_POINT('',(-1.18829206995915,-2.22507172762053E-5,56.4155118763048));
#40359=CARTESIAN_POINT('',(-1.188225,-1.45515594291686E-16,57.95));
#40360=CARTESIAN_POINT('Ctrl Pts',(-1.18826932065667,-2.69461188108222E-5,
56.4580381236952));
#40361=CARTESIAN_POINT('Ctrl Pts',(-1.18810768463847,0.165161660669492,
56.4513995482));
#40362=CARTESIAN_POINT('Ctrl Pts',(-1.15335574970162,0.330416144443476,
56.4447609727049));
#40363=CARTESIAN_POINT('Ctrl Pts',(-1.0864436295599,0.481419953396779,56.4381223972098));
#40364=CARTESIAN_POINT('Ctrl Pts',(-1.00656403790443,0.661688080786279,
56.430197275444));
#40365=CARTESIAN_POINT('Ctrl Pts',(-0.880851198609791,0.821646788192008,
56.4222721536783));
#40366=CARTESIAN_POINT('Ctrl Pts',(-0.724571239081175,0.941871249812796,
56.4143470319126));
#40367=CARTESIAN_POINT('Ctrl Pts',(-0.568291279552556,1.06209571143359,
56.4064219101469));
#40368=CARTESIAN_POINT('Ctrl Pts',(-0.381444199789957,1.14258592726943,
56.3984967883812));
#40369=CARTESIAN_POINT('Ctrl Pts',(-0.18672005555549,1.17356744699151,56.3905716666154));
#40370=CARTESIAN_POINT('Ctrl Pts',(0.00800408867897459,1.20454896671359,
56.3826465448497));
#40371=CARTESIAN_POINT('Ctrl Pts',(0.210605297385308,1.1860217903219,56.374721423084));
#40372=CARTESIAN_POINT('Ctrl Pts',(0.396480388623666,1.12023579351038,56.3667963013183));
#40373=CARTESIAN_POINT('Ctrl Pts',(0.582355479862024,1.05444979669886,56.3588711795526));
#40374=CARTESIAN_POINT('Ctrl Pts',(0.751504453632407,0.941404979467515,
56.3509460577869));
#40375=CARTESIAN_POINT('Ctrl Pts',(0.883386450102643,0.794829108512784,
56.3430209360211));
#40376=CARTESIAN_POINT('Ctrl Pts',(1.01526844657288,0.648253237558053,56.3350958142554));
#40377=CARTESIAN_POINT('Ctrl Pts',(1.10988346574297,0.468146312879939,56.3271706924897));
#40378=CARTESIAN_POINT('Ctrl Pts',(1.15574179108387,0.276379890303732,56.319245570724));
#40379=CARTESIAN_POINT('Ctrl Pts',(1.20160011642478,0.0846134677275266,
56.3113204489583));
#40380=CARTESIAN_POINT('Ctrl Pts',(1.1987017479365,-0.118812452746773,56.3033953271926));
#40381=CARTESIAN_POINT('Ctrl Pts',(1.14739865246892,-0.30919454104491,56.2954702054269));
#40382=CARTESIAN_POINT('Ctrl Pts',(1.09609555700134,-0.499576629343047,
56.2875450836611));
#40383=CARTESIAN_POINT('Ctrl Pts',(0.996387734554462,-0.676914885465023,
56.2796199618954));
#40384=CARTESIAN_POINT('Ctrl Pts',(0.860383356175942,-0.81967396751617,
56.2716948401297));
#40385=CARTESIAN_POINT('Ctrl Pts',(0.72437897779742,-0.962433049567319,
56.263769718364));
#40386=CARTESIAN_POINT('Ctrl Pts',(0.552078043487259,-1.07061295754764,
56.2558445965983));
#40387=CARTESIAN_POINT('Ctrl Pts',(0.364404171862087,-1.13107671147003,
56.2479194748325));
#40388=CARTESIAN_POINT('Ctrl Pts',(0.176730300236916,-1.19154046539241,
56.2399943530668));
#40389=CARTESIAN_POINT('Ctrl Pts',(-0.0263165087032649,-1.20428806525687,
56.2320692313011));
#40390=CARTESIAN_POINT('Ctrl Pts',(-0.220078951989418,-1.1677714664526,
56.2241441095354));
#40391=CARTESIAN_POINT('Ctrl Pts',(-0.41384139527557,-1.13125486764833,
56.2162189877697));
#40392=CARTESIAN_POINT('Ctrl Pts',(-0.598319472907694,-1.04547407017534,
56.2082938660039));
#40393=CARTESIAN_POINT('Ctrl Pts',(-0.751110831485251,-0.920846038545505,
56.2003687442382));
#40394=CARTESIAN_POINT('Ctrl Pts',(-0.903902190062808,-0.796218006915672,
56.1924436224725));
#40395=CARTESIAN_POINT('Ctrl Pts',(-1.0250068295858,-0.632742741128994,
56.1845185007068));
#40396=CARTESIAN_POINT('Ctrl Pts',(-1.09971818539801,-0.450272009507053,
56.1765933789411));
#40397=CARTESIAN_POINT('Ctrl Pts',(-1.15802594469153,-0.307864481469854,
56.1704082938591));
#40398=CARTESIAN_POINT('Ctrl Pts',(-1.18807614896463,-0.153887058438266,
56.1642232087771));
#40399=CARTESIAN_POINT('Ctrl Pts',(-1.18823416249667,3.04042717342579E-5,
56.1580381236952));
#40400=CARTESIAN_POINT('Ctrl Pts',(-1.1882111814849,2.07922408733904E-5,
56.1155118763048));
#40401=CARTESIAN_POINT('Ctrl Pts',(-1.18806735346424,-0.145890075929576,
56.1213749495004));
#40402=CARTESIAN_POINT('Ctrl Pts',(-1.16113150647432,-0.291848839038371,
56.1272380226959));
#40403=CARTESIAN_POINT('Ctrl Pts',(-1.10860087444441,-0.427930629202327,
56.1331010958914));
#40404=CARTESIAN_POINT('Ctrl Pts',(-1.03759516781542,-0.611872517897413,
56.1410262176572));
#40405=CARTESIAN_POINT('Ctrl Pts',(-0.919825343828156,-0.777768233467184,
56.1489513394229));
#40406=CARTESIAN_POINT('Ctrl Pts',(-0.769587398025842,-0.905462855000406,
56.1568764611886));
#40407=CARTESIAN_POINT('Ctrl Pts',(-0.619349452223529,-1.03315747653363,
56.1648015829543));
#40408=CARTESIAN_POINT('Ctrl Pts',(-0.43664338460617,-1.1226510040303,56.17272670472));
#40409=CARTESIAN_POINT('Ctrl Pts',(-0.243659060499568,-1.16307964514265,
56.1806518264858));
#40410=CARTESIAN_POINT('Ctrl Pts',(-0.0506747363929658,-1.203508286255,
56.1885769482515));
#40411=CARTESIAN_POINT('Ctrl Pts',(0.15258784420288,-1.19487204098302,56.1965020700172));
#40412=CARTESIAN_POINT('Ctrl Pts',(0.341446405860296,-1.13821776082292,
56.2044271917829));
#40413=CARTESIAN_POINT('Ctrl Pts',(0.530304967517711,-1.08156348066281,
56.2123523135486));
#40414=CARTESIAN_POINT('Ctrl Pts',(0.704759510236697,-0.976891165614581,
56.2202774353144));
#40415=CARTESIAN_POINT('Ctrl Pts',(0.843624313143388,-0.836912727100357,
56.2282025570801));
#40416=CARTESIAN_POINT('Ctrl Pts',(0.982489116050078,-0.696934288586134,
56.2361276788458));
#40417=CARTESIAN_POINT('Ctrl Pts',(1.08576417914447,-0.521649726605918,
56.2440528006115));
#40418=CARTESIAN_POINT('Ctrl Pts',(1.14090840415554,-0.332344578155793,
56.2519779223772));
#40419=CARTESIAN_POINT('Ctrl Pts',(1.1960526291666,-0.143039429705667,56.2599030441429));
#40420=CARTESIAN_POINT('Ctrl Pts',(1.20306601609434,0.0602863052143686,
56.2678281659087));
#40421=CARTESIAN_POINT('Ctrl Pts',(1.16109676099022,0.252941272364512,56.2757532876744));
#40422=CARTESIAN_POINT('Ctrl Pts',(1.1191275058861,0.445596239514657,56.2836784094401));
#40423=CARTESIAN_POINT('Ctrl Pts',(1.02817560875013,0.627580438894908,56.2916035312058));
#40424=CARTESIAN_POINT('Ctrl Pts',(0.89928600670914,0.776794433451253,56.2995286529715));
#40425=CARTESIAN_POINT('Ctrl Pts',(0.77039640466815,0.926008428007598,56.3074537747372));
#40426=CARTESIAN_POINT('Ctrl Pts',(0.603569097722146,1.04245221774004,56.315378896503));
#40427=CARTESIAN_POINT('Ctrl Pts',(0.41906298399761,1.1119852356127,56.3233040182687));
#40428=CARTESIAN_POINT('Ctrl Pts',(0.234556870273075,1.18151825348535,56.3312291400344));
#40429=CARTESIAN_POINT('Ctrl Pts',(0.0323719497700094,1.20414049949823,
56.3391542618001));
#40430=CARTESIAN_POINT('Ctrl Pts',(-0.162939135811373,1.17710482606222,
56.3470793835658));
#40431=CARTESIAN_POINT('Ctrl Pts',(-0.358250221392757,1.15006915262621,
56.3550045053316));
#40432=CARTESIAN_POINT('Ctrl Pts',(-0.546687472052457,1.0733755597413,56.3629296270973));
#40433=CARTESIAN_POINT('Ctrl Pts',(-0.705367732965258,0.956337440296682,
56.370854748863));
#40434=CARTESIAN_POINT('Ctrl Pts',(-0.864047993878058,0.839299320852068,
56.3787798706287));
#40435=CARTESIAN_POINT('Ctrl Pts',(-0.992971265043959,0.681916674847751,
56.3867049923944));
#40436=CARTESIAN_POINT('Ctrl Pts',(-1.07648155278485,0.503301504297487,
56.3946301141602));
#40437=CARTESIAN_POINT('Ctrl Pts',(-1.14982814256138,0.346424860753121,
56.4015907015417));
#40438=CARTESIAN_POINT('Ctrl Pts',(-1.18814313612308,0.173169438048752,
56.4085512889233));
#40439=CARTESIAN_POINT('Ctrl Pts',(-1.18829206995915,-2.22507172762053E-5,
56.4155118763048));
#40440=CARTESIAN_POINT('Origin',(0.,0.,57.95));
#40441=CARTESIAN_POINT('',(-1.1881295160484,7.99197013834352E-6,56.7580381236952));
#40442=CARTESIAN_POINT('',(-1.18812635417301,6.58327025343463E-7,56.7155118763048));
#40443=CARTESIAN_POINT('',(-1.188225,-1.45515594291686E-16,57.95));
#40444=CARTESIAN_POINT('Ctrl Pts',(-1.1881295160484,7.99197013834352E-6,
56.7580381236952));
#40445=CARTESIAN_POINT('Ctrl Pts',(-1.18815070391462,0.0899160987151799,
56.7544261311544));
#40446=CARTESIAN_POINT('Ctrl Pts',(-1.17807704964198,0.179819532343893,
56.7508141386136));
#40447=CARTESIAN_POINT('Ctrl Pts',(-1.15785703751179,0.267379902805148,
56.7472021460728));
#40448=CARTESIAN_POINT('Ctrl Pts',(-1.11349203497487,0.459497297821303,
56.739277024307));
#40449=CARTESIAN_POINT('Ctrl Pts',(-1.02028110348739,0.640334872175578,
56.7313519025413));
#40450=CARTESIAN_POINT('Ctrl Pts',(-0.889543452490429,0.787932343460453,
56.7234267807756));
#40451=CARTESIAN_POINT('Ctrl Pts',(-0.758805801493465,0.935529814745327,
56.7155016590099));
#40452=CARTESIAN_POINT('Ctrl Pts',(-0.590541430987019,1.0498871829608,56.7075765372442));
#40453=CARTESIAN_POINT('Ctrl Pts',(-0.405183777488024,1.1171172893659,56.6996514154785));
#40454=CARTESIAN_POINT('Ctrl Pts',(-0.21982612398903,1.18434739577099,56.6917262937127));
#40455=CARTESIAN_POINT('Ctrl Pts',(-0.0173751874974873,1.2044502403657,
56.683801171947));
#40456=CARTESIAN_POINT('Ctrl Pts',(0.177584098490914,1.174984604028,56.6758760501813));
#40457=CARTESIAN_POINT('Ctrl Pts',(0.372543384479318,1.1455189676903,56.6679509284156));
#40458=CARTESIAN_POINT('Ctrl Pts',(0.56001101996458,1.06648485042019,56.6600258066499));
#40459=CARTESIAN_POINT('Ctrl Pts',(0.717221591109313,0.947479878934791,
56.6521006848842));
#40460=CARTESIAN_POINT('Ctrl Pts',(0.874432162254045,0.828474907449395,
56.6441755631184));
#40461=CARTESIAN_POINT('Ctrl Pts',(1.00138566905825,0.669499081748719,56.6362504413527));
#40462=CARTESIAN_POINT('Ctrl Pts',(1.08266532177563,0.489857869962454,56.628325319587));
#40463=CARTESIAN_POINT('Ctrl Pts',(1.16394497449302,0.310216658176189,56.6204001978213));
#40464=CARTESIAN_POINT('Ctrl Pts',(1.19955077312359,0.109910060304336,56.6124750760556));
#40465=CARTESIAN_POINT('Ctrl Pts',(1.18515887404106,-0.0867373911377846,
56.6045499542899));
#40466=CARTESIAN_POINT('Ctrl Pts',(1.17076697495852,-0.283384842579906,
56.5966248325241));
#40467=CARTESIAN_POINT('Ctrl Pts',(1.10637737816288,-0.476373147592297,
56.5886997107584));
#40468=CARTESIAN_POINT('Ctrl Pts',(0.999809331035505,-0.642266481543283,
56.5807745889927));
#40469=CARTESIAN_POINT('Ctrl Pts',(0.893241283908128,-0.808159815494271,
56.572849467227));
#40470=CARTESIAN_POINT('Ctrl Pts',(0.744494786449013,-0.946958178383857,
56.5649243454613));
#40471=CARTESIAN_POINT('Ctrl Pts',(0.571633092951576,-1.04180638257905,
56.5569992236955));
#40472=CARTESIAN_POINT('Ctrl Pts',(0.39877139945414,-1.13665458677424,56.5490741019298));
#40473=CARTESIAN_POINT('Ctrl Pts',(0.201794509918382,-1.18755263227503,
56.5411489801641));
#40474=CARTESIAN_POINT('Ctrl Pts',(0.00462260872706689,-1.18831963849283,
56.5332238583984));
#40475=CARTESIAN_POINT('Ctrl Pts',(-0.192549292464249,-1.18908664471064,
56.5252987366327));
#40476=CARTESIAN_POINT('Ctrl Pts',(-0.389916205311122,-1.13972261164545,
56.5173736148669));
#40477=CARTESIAN_POINT('Ctrl Pts',(-0.563510582363015,-1.046222134781,56.5094484931012));
#40478=CARTESIAN_POINT('Ctrl Pts',(-0.737104959414911,-0.952721657916548,
56.5015233713355));
#40479=CARTESIAN_POINT('Ctrl Pts',(-0.886926800671826,-0.815084737252838,
56.4935982495698));
#40480=CARTESIAN_POINT('Ctrl Pts',(-0.994782265853485,-0.650025518946005,
56.4856731278041));
#40481=CARTESIAN_POINT('Ctrl Pts',(-1.10263773103514,-0.484966300639175,
56.4777480060383));
#40482=CARTESIAN_POINT('Ctrl Pts',(-1.16852682014155,-0.292484784689223,
56.4698228842726));
#40483=CARTESIAN_POINT('Ctrl Pts',(-1.1844481926866,-0.0959552530276115,
56.4618977625069));
#40484=CARTESIAN_POINT('Ctrl Pts',(-1.18703283215031,-0.0640510951492984,
56.4606112162363));
#40485=CARTESIAN_POINT('Ctrl Pts',(-1.18830064548179,-0.0320402577338833,
56.4593246699657));
#40486=CARTESIAN_POINT('Ctrl Pts',(-1.18826932065667,-2.69461188108222E-5,
56.4580381236952));
#40487=CARTESIAN_POINT('Ctrl Pts',(-1.18829206995915,-2.22507172762053E-5,
56.4155118763048));
#40488=CARTESIAN_POINT('Ctrl Pts',(-1.18831270784472,-0.0240215671124719,
56.416476410689));
#40489=CARTESIAN_POINT('Ctrl Pts',(-1.1876004858046,-0.0480196596965209,
56.4174409450732));
#40490=CARTESIAN_POINT('Ctrl Pts',(-1.18614706359603,-0.0719727779040691,
56.4184054794573));
#40491=CARTESIAN_POINT('Ctrl Pts',(-1.17420498235045,-0.268784194459149,
56.426330601223));
#40492=CARTESIAN_POINT('Ctrl Pts',(-1.11222351554338,-0.462559332473099,
56.4342557229888));
#40493=CARTESIAN_POINT('Ctrl Pts',(-1.00772947510678,-0.629766816194386,
56.4421808447545));
#40494=CARTESIAN_POINT('Ctrl Pts',(-0.903235434670179,-0.796974299915674,
56.4501059665202));
#40495=CARTESIAN_POINT('Ctrl Pts',(-0.756228820604034,-0.937614129344298,
56.4580310882859));
#40496=CARTESIAN_POINT('Ctrl Pts',(-0.584561602112513,-1.03460749599802,
56.4659562100516));
#40497=CARTESIAN_POINT('Ctrl Pts',(-0.412894383620994,-1.13160086265175,
56.4738813318173));
#40498=CARTESIAN_POINT('Ctrl Pts',(-0.216566560704099,-1.18494776653058,
56.4818064535831));
#40499=CARTESIAN_POINT('Ctrl Pts',(-0.0194194972431365,-1.1881699460625,
56.4897315753488));
#40500=CARTESIAN_POINT('Ctrl Pts',(0.177727566217826,-1.19139212559442,
56.4976566971145));
#40501=CARTESIAN_POINT('Ctrl Pts',(0.375693870222856,-1.14448958077944,
56.5055818188802));
#40502=CARTESIAN_POINT('Ctrl Pts',(0.55043907930015,-1.05315799266839,56.5135069406459));
#40503=CARTESIAN_POINT('Ctrl Pts',(0.725184288377445,-0.961826404557346,
56.5214320624117));
#40504=CARTESIAN_POINT('Ctrl Pts',(0.876708402527002,-0.826065773150231,
56.5293571841774));
#40505=CARTESIAN_POINT('Ctrl Pts',(0.986610863427943,-0.662362394554791,
56.5372823059431));
#40506=CARTESIAN_POINT('Ctrl Pts',(1.09651332432888,-0.498659015959353,
56.5452074277088));
#40507=CARTESIAN_POINT('Ctrl Pts',(1.16479413198121,-0.30701289017559,56.5531325494745));
#40508=CARTESIAN_POINT('Ctrl Pts',(1.18316150395738,-0.110696852303948,
56.5610576712402));
#40509=CARTESIAN_POINT('Ctrl Pts',(1.20152887593356,0.0856191855676947,
56.568982793006));
#40510=CARTESIAN_POINT('Ctrl Pts',(1.1699828122336,0.286605135527218,56.5769079147717));
#40511=CARTESIAN_POINT('Ctrl Pts',(1.09235415648164,0.467853966927145,56.5848330365374));
#40512=CARTESIAN_POINT('Ctrl Pts',(1.01472550072968,0.649102798327074,56.5927581583031));
#40513=CARTESIAN_POINT('Ctrl Pts',(0.891014252925719,0.810614511167405,
56.6006832800688));
#40514=CARTESIAN_POINT('Ctrl Pts',(0.736243474222775,0.932775688051391,
56.6086084018345));
#40515=CARTESIAN_POINT('Ctrl Pts',(0.581472695519832,1.05493686493538,56.6165335236003));
#40516=CARTESIAN_POINT('Ctrl Pts',(0.395642385917902,1.13774750586301,56.624458645366));
#40517=CARTESIAN_POINT('Ctrl Pts',(0.201319128128168,1.17115137629747,56.6323837671317));
#40518=CARTESIAN_POINT('Ctrl Pts',(0.00699587033843588,1.20455524673192,
56.6403088888974));
#40519=CARTESIAN_POINT('Ctrl Pts',(-0.1958203356391,1.18855234667319,56.6482340106631));
#40520=CARTESIAN_POINT('Ctrl Pts',(-0.382500199260759,1.12508601232077,
56.6561591324289));
#40521=CARTESIAN_POINT('Ctrl Pts',(-0.569180062882424,1.06161967796835,
56.6640842541946));
#40522=CARTESIAN_POINT('Ctrl Pts',(-0.739723584148212,0.950689909322242,
56.6720093759603));
#40523=CARTESIAN_POINT('Ctrl Pts',(-0.873420554445836,0.80576762942286,
56.679934497726));
#40524=CARTESIAN_POINT('Ctrl Pts',(-1.00711752474346,0.660845349523481,
56.6878596194917));
#40525=CARTESIAN_POINT('Ctrl Pts',(-1.10396794407292,0.481930558370832,
56.6957847412574));
#40526=CARTESIAN_POINT('Ctrl Pts',(-1.15221063632171,0.290750042306688,
56.7037098630232));
#40527=CARTESIAN_POINT('Ctrl Pts',(-1.17615815037868,0.195848661756558,
56.7076438674504));
#40528=CARTESIAN_POINT('Ctrl Pts',(-1.18812824895107,0.0979248876013811,
56.7115778718776));
#40529=CARTESIAN_POINT('Ctrl Pts',(-1.18812635417301,6.58327025343463E-7,
56.7155118763048));
#40530=CARTESIAN_POINT('Origin',(0.,0.,57.95));
#40531=CARTESIAN_POINT('',(-1.18831370045495,1.46328030788886E-5,57.0580381236952));
#40532=CARTESIAN_POINT('',(-1.18829575305801,2.12367321252666E-5,57.0155118763048));
#40533=CARTESIAN_POINT('',(-1.188225,-1.45515594291686E-16,57.95));
#40534=CARTESIAN_POINT('Ctrl Pts',(-1.18831370045495,1.46328030788886E-5,
57.0580381236952));
#40535=CARTESIAN_POINT('Ctrl Pts',(-1.18832270521549,0.0145798869936275,
57.0574527141087));
#40536=CARTESIAN_POINT('Ctrl Pts',(-1.18806045407433,0.0291448164884335,
57.0568673045222));
#40537=CARTESIAN_POINT('Ctrl Pts',(-1.18752484989022,0.0436996868738372,
57.0562818949358));
#40538=CARTESIAN_POINT('Ctrl Pts',(-1.18027398062638,0.240739712789417,
57.0483567731701));
#40539=CARTESIAN_POINT('Ctrl Pts',(-1.12292560142346,0.435936202127469,
57.0404316514043));
#40540=CARTESIAN_POINT('Ctrl Pts',(-1.02244389883069,0.605585176076476,
57.0325065296386));
#40541=CARTESIAN_POINT('Ctrl Pts',(-0.921962196237911,0.775234150025483,
57.0245814078729));
#40542=CARTESIAN_POINT('Ctrl Pts',(-0.778347170255276,0.919335608585445,
57.0166562861072));
#40543=CARTESIAN_POINT('Ctrl Pts',(-0.609038927231272,1.02039037473736,
57.0087311643415));
#40544=CARTESIAN_POINT('Ctrl Pts',(-0.439730684207273,1.12144514088928,
57.0008060425757));
#40545=CARTESIAN_POINT('Ctrl Pts',(-0.244729224141906,1.17945321463315,
56.99288092081));
#40546=CARTESIAN_POINT('Ctrl Pts',(-0.0477148421740822,1.18737029842252,
56.9849557990443));
#40547=CARTESIAN_POINT('Ctrl Pts',(0.149299539793748,1.19528738221189,56.9770306772786));
#40548=CARTESIAN_POINT('Ctrl Pts',(0.348326843664036,1.15311347604675,56.9691055555129));
#40549=CARTESIAN_POINT('Ctrl Pts',(0.525197889909765,1.0659700315553,56.9611804337472));
#40550=CARTESIAN_POINT('Ctrl Pts',(0.702068936155495,0.978826587063846,
56.9532553119814));
#40551=CARTESIAN_POINT('Ctrl Pts',(0.856783724776667,0.846713604246079,
56.9453301902157));
#40552=CARTESIAN_POINT('Ctrl Pts',(0.970554233080142,0.685674421566015,
56.93740506845));
#40553=CARTESIAN_POINT('Ctrl Pts',(1.08432474138362,0.524635238885952,56.9294799466843));
#40554=CARTESIAN_POINT('Ctrl Pts',(1.15715096936939,0.334669856343592,56.9215548249186));
#40555=CARTESIAN_POINT('Ctrl Pts',(1.18018915467806,0.138847005441106,56.9136297031528));
#40556=CARTESIAN_POINT('Ctrl Pts',(1.20322733998672,-0.0569758454613808,
56.9057045813871));
#40557=CARTESIAN_POINT('Ctrl Pts',(1.17647748261828,-0.25865616472399,56.8977794596214));
#40558=CARTESIAN_POINT('Ctrl Pts',(1.10318799167282,-0.441702599911483,
56.8898543378557));
#40559=CARTESIAN_POINT('Ctrl Pts',(1.02989850072736,-0.624749035098976,
56.88192921609));
#40560=CARTESIAN_POINT('Ctrl Pts',(0.910069376204889,-0.789161586211348,
56.8740040943243));
#40561=CARTESIAN_POINT('Ctrl Pts',(0.758252247790524,-0.914974568204106,
56.8660789725585));
#40562=CARTESIAN_POINT('Ctrl Pts',(0.606435119376161,-1.04078755019686,
56.8581538507928));
#40563=CARTESIAN_POINT('Ctrl Pts',(0.422629987069901,-1.12800096307001,
56.8502287290271));
#40564=CARTESIAN_POINT('Ctrl Pts',(0.229157503135587,-1.16602391506192,
56.8423036072614));
#40565=CARTESIAN_POINT('Ctrl Pts',(0.0356850192012729,-1.20404686705384,
56.8343784854957));
#40566=CARTESIAN_POINT('Ctrl Pts',(-0.167454816361101,-1.19287935816454,
56.8264533637299));
#40567=CARTESIAN_POINT('Ctrl Pts',(-0.355593412562655,-1.13387753160635,
56.8185282419642));
#40568=CARTESIAN_POINT('Ctrl Pts',(-0.543732008764212,-1.07487570504817,
56.8106031201985));
#40569=CARTESIAN_POINT('Ctrl Pts',(-0.716869365604949,-0.968039560821109,
56.8026779984328));
#40570=CARTESIAN_POINT('Ctrl Pts',(-0.853980288154606,-0.826342906536414,
56.7947528766671));
#40571=CARTESIAN_POINT('Ctrl Pts',(-0.991091210704261,-0.684646252251721,
56.7868277549014));
#40572=CARTESIAN_POINT('Ctrl Pts',(-1.09217569896284,-0.508089087909396,
56.7789026331357));
#40573=CARTESIAN_POINT('Ctrl Pts',(-1.14495840629895,-0.318111897899217,
56.7709775113699));
#40574=CARTESIAN_POINT('Ctrl Pts',(-1.17368460689391,-0.214719647972578,
56.766664382145));
#40575=CARTESIAN_POINT('Ctrl Pts',(-1.18810421533032,-0.107352496286196,
56.7623512529201));
#40576=CARTESIAN_POINT('Ctrl Pts',(-1.1881295160484,7.99197013834352E-6,
56.7580381236952));
#40577=CARTESIAN_POINT('Ctrl Pts',(-1.18812635417301,6.58327025343463E-7,
56.7155118763048));
#40578=CARTESIAN_POINT('Ctrl Pts',(-1.18812443188702,-0.0993452108875006,
56.7195029936433));
#40579=CARTESIAN_POINT('Ctrl Pts',(-1.17580038004544,-0.198691548531745,
56.7234941109818));
#40580=CARTESIAN_POINT('Ctrl Pts',(-1.15115986037899,-0.294882880829771,
56.7274852283203));
#40581=CARTESIAN_POINT('Ctrl Pts',(-1.10223142701937,-0.485889046926449,
56.735410350086));
#40582=CARTESIAN_POINT('Ctrl Pts',(-1.00473959513201,-0.664455138144163,
56.7433354718517));
#40583=CARTESIAN_POINT('Ctrl Pts',(-0.870523431726741,-0.808896713041235,
56.7512605936175));
#40584=CARTESIAN_POINT('Ctrl Pts',(-0.73630726832148,-0.953338287938303,
56.7591857153832));
#40585=CARTESIAN_POINT('Ctrl Pts',(-0.565366773398321,-1.06365534651473,
56.7671108371489));
#40586=CARTESIAN_POINT('Ctrl Pts',(-0.378460362661497,-1.12645137109791,
56.7750359589146));
#40587=CARTESIAN_POINT('Ctrl Pts',(-0.191553951924672,-1.18924739568109,
56.7829610806803));
#40588=CARTESIAN_POINT('Ctrl Pts',(0.0113183746258182,-1.20452238627102,
56.7908862024461));
#40589=CARTESIAN_POINT('Ctrl Pts',(0.205520511359668,-1.1704214014468,56.7988113242118));
#40590=CARTESIAN_POINT('Ctrl Pts',(0.399722648093518,-1.13632041662258,
56.8067364459775));
#40591=CARTESIAN_POINT('Ctrl Pts',(0.58525459501073,-1.0528434563842,56.8146615677432));
#40592=CARTESIAN_POINT('Ctrl Pts',(0.739586001522012,-0.930127670756498,
56.8225866895089));
#40593=CARTESIAN_POINT('Ctrl Pts',(0.893917408033295,-0.807411885128797,
56.8305118112747));
#40594=CARTESIAN_POINT('Ctrl Pts',(1.01704827413865,-0.64545727411177,56.8384369330404));
#40595=CARTESIAN_POINT('Ctrl Pts',(1.09402601820557,-0.463931039103322,
56.8463620548061));
#40596=CARTESIAN_POINT('Ctrl Pts',(1.17100376227249,-0.282404804094877,
56.8542871765718));
#40597=CARTESIAN_POINT('Ctrl Pts',(1.20182838430099,-0.081306945095011,
56.8622122983375));
#40598=CARTESIAN_POINT('Ctrl Pts',(1.18275665002534,0.114941917397725,56.8701374201032));
#40599=CARTESIAN_POINT('Ctrl Pts',(1.16368491574969,0.311190779890463,56.878062541869));
#40600=CARTESIAN_POINT('Ctrl Pts',(1.09471682516991,0.50259064587607,56.8859876636347));
#40601=CARTESIAN_POINT('Ctrl Pts',(0.984227621935687,0.665898585201267,
56.8939127854004));
#40602=CARTESIAN_POINT('Ctrl Pts',(0.87373841870147,0.829206524526464,56.9018379071661));
#40603=CARTESIAN_POINT('Ctrl Pts',(0.721728102812821,0.964422537191249,
56.9097630289318));
#40604=CARTESIAN_POINT('Ctrl Pts',(0.546656275255271,1.05512646364228,56.9176881506976));
#40605=CARTESIAN_POINT('Ctrl Pts',(0.371584447697719,1.14583039009331,56.9256132724633));
#40606=CARTESIAN_POINT('Ctrl Pts',(0.173451108471265,1.19202223033058,56.933538394229));
#40607=CARTESIAN_POINT('Ctrl Pts',(-0.0236831228360759,1.18809260886808,
56.9414635159947));
#40608=CARTESIAN_POINT('Ctrl Pts',(-0.220817354143417,1.18416298740558,
56.9493886377604));
#40609=CARTESIAN_POINT('Ctrl Pts',(-0.416952477531646,1.1301119042433,56.9573137595261));
#40610=CARTESIAN_POINT('Ctrl Pts',(-0.588270529753804,1.03250313383418,
56.9652388812919));
#40611=CARTESIAN_POINT('Ctrl Pts',(-0.759588581975962,0.93489436342506,
56.9731640030576));
#40612=CARTESIAN_POINT('Ctrl Pts',(-0.90608956303205,0.793727905769093,
56.9810891248233));
#40613=CARTESIAN_POINT('Ctrl Pts',(-1.00998290628536,0.62614652164298,56.989014246589));
#40614=CARTESIAN_POINT('Ctrl Pts',(-1.11387624953867,0.458565137516867,
56.9969393683547));
#40615=CARTESIAN_POINT('Ctrl Pts',(-1.17516195498921,0.264568826920607,
57.0048644901205));
#40616=CARTESIAN_POINT('Ctrl Pts',(-1.18639770096215,0.0677158231578859,
57.0127896118862));
#40617=CARTESIAN_POINT('Ctrl Pts',(-1.1876841868309,0.0451762776598449,
57.0136970333591));
#40618=CARTESIAN_POINT('Ctrl Pts',(-1.18831451240506,0.0225992806104096,
57.014604454832));
#40619=CARTESIAN_POINT('Ctrl Pts',(-1.18829575305801,2.12367321252666E-5,
57.0155118763048));
#40620=CARTESIAN_POINT('Origin',(0.,0.,57.95));
#40621=CARTESIAN_POINT('',(-1.1881820096365,-2.79964409908851E-5,57.3580381236952));
#40622=CARTESIAN_POINT('',(-1.18820495619059,-3.01830341203513E-5,57.3155118763048));
#40623=CARTESIAN_POINT('',(-1.188225,-1.45515594291686E-16,57.95));
#40624=CARTESIAN_POINT('Ctrl Pts',(-1.1881820096365,-2.79964409908851E-5,
57.3580381236952));
#40625=CARTESIAN_POINT('Ctrl Pts',(-1.18806234971613,0.136458721817245,
57.3525541752973));
#40626=CARTESIAN_POINT('Ctrl Pts',(-1.1645682320165,0.272985576997064,57.3470702268995));
#40627=CARTESIAN_POINT('Ctrl Pts',(-1.11848096038993,0.401404126766149,
57.3415862785016));
#40628=CARTESIAN_POINT('Ctrl Pts',(-1.05187799242009,0.58698804733984,57.3336611567359));
#40629=CARTESIAN_POINT('Ctrl Pts',(-0.938090234140422,0.755638135133434,
57.3257360349702));
#40630=CARTESIAN_POINT('Ctrl Pts',(-0.790935672853952,0.886874113471996,
57.3178109132045));
#40631=CARTESIAN_POINT('Ctrl Pts',(-0.643781111567482,1.01811009181056,
57.3098857914388));
#40632=CARTESIAN_POINT('Ctrl Pts',(-0.463259747274216,1.11193196069409,
57.3019606696731));
#40633=CARTESIAN_POINT('Ctrl Pts',(-0.271293462938056,1.15694632058136,
57.2940355479073));
#40634=CARTESIAN_POINT('Ctrl Pts',(-0.0793271786018923,1.20196068046864,
57.2861104261416));
#40635=CARTESIAN_POINT('Ctrl Pts',(0.124084025777165,1.19816753135966,57.2781853043759));
#40636=CARTESIAN_POINT('Ctrl Pts',(0.314238605130466,1.14602750001269,57.2702601826102));
#40637=CARTESIAN_POINT('Ctrl Pts',(0.504393184483765,1.09388746866572,57.2623350608444));
#40638=CARTESIAN_POINT('Ctrl Pts',(0.681291138811312,0.993400555080754,
57.2544099390787));
#40639=CARTESIAN_POINT('Ctrl Pts',(0.823450599379697,0.856769538511313,
57.246484817313));
#40640=CARTESIAN_POINT('Ctrl Pts',(0.965610059948084,0.720138521941871,
57.2385596955473));
#40641=CARTESIAN_POINT('Ctrl Pts',(1.07303102675731,0.547363402387949,57.2306345737816));
#40642=CARTESIAN_POINT('Ctrl Pts',(1.13266867338764,0.359425385950907,57.2227094520159));
#40643=CARTESIAN_POINT('Ctrl Pts',(1.19230632001797,0.171487369513864,57.2147843302501));
#40644=CARTESIAN_POINT('Ctrl Pts',(1.20416064646939,-0.0316135438062997,
57.2068592084844));
#40645=CARTESIAN_POINT('Ctrl Pts',(1.1667921048075,-0.225213489601638,57.1989340867187));
#40646=CARTESIAN_POINT('Ctrl Pts',(1.12942356314562,-0.418813435396977,
57.191008964953));
#40647=CARTESIAN_POINT('Ctrl Pts',(1.04283215337043,-0.602912413667489,
57.1830838431873));
#40648=CARTESIAN_POINT('Ctrl Pts',(0.917533233363273,-0.755154088523403,
57.1751587214215));
#40649=CARTESIAN_POINT('Ctrl Pts',(0.792234313356116,-0.907395763379314,
57.1672335996558));
#40650=CARTESIAN_POINT('Ctrl Pts',(0.628227883116994,-1.02778013482063,
57.1593084778901));
#40651=CARTESIAN_POINT('Ctrl Pts',(0.445430309792281,-1.10168814591881,
57.1513833561244));
#40652=CARTESIAN_POINT('Ctrl Pts',(0.262632736467569,-1.17559615701699,
57.1434582343587));
#40653=CARTESIAN_POINT('Ctrl Pts',(0.0610440200572671,-1.20302780777205,
57.135533112593));
#40654=CARTESIAN_POINT('Ctrl Pts',(-0.134855610933311,-1.18065189448011,
57.1276079908272));
#40655=CARTESIAN_POINT('Ctrl Pts',(-0.330755241923892,-1.15827598118818,
57.1196828690615));
#40656=CARTESIAN_POINT('Ctrl Pts',(-0.520965787494748,-1.08609250384925,
57.1117577472958));
#40657=CARTESIAN_POINT('Ctrl Pts',(-0.68238874440318,-0.972867171432731,
57.1038326255301));
#40658=CARTESIAN_POINT('Ctrl Pts',(-0.843811701311613,-0.859641839016208,
57.0959075037643));
#40659=CARTESIAN_POINT('Ctrl Pts',(-0.976447069557621,-0.705374651522084,
57.0879823819986));
#40660=CARTESIAN_POINT('Ctrl Pts',(-1.06418807401824,-0.528799276528467,
57.0800572602329));
#40661=CARTESIAN_POINT('Ctrl Pts',(-1.14544786258642,-0.365267097628355,
57.0727175480537));
#40662=CARTESIAN_POINT('Ctrl Pts',(-1.18820080112409,-0.182600712158311,
57.0653778358744));
#40663=CARTESIAN_POINT('Ctrl Pts',(-1.18831370045495,1.46328030788886E-5,
57.0580381236952));
#40664=CARTESIAN_POINT('Ctrl Pts',(-1.18829575305801,2.12367321252666E-5,
57.0155118763048));
#40665=CARTESIAN_POINT('Ctrl Pts',(-1.18815067441569,-0.174589955388741,
57.0225295765977));
#40666=CARTESIAN_POINT('Ctrl Pts',(-1.14918402982291,-0.349263758015375,
57.0295472768905));
#40667=CARTESIAN_POINT('Ctrl Pts',(-1.07466852275288,-0.507161220676781,
57.0365649771833));
#40668=CARTESIAN_POINT('Ctrl Pts',(-0.990517812075319,-0.685475563819546,
57.044490098949));
#40669=CARTESIAN_POINT('Ctrl Pts',(-0.861030604224841,-0.84239455317589,
57.0524152207148));
#40670=CARTESIAN_POINT('Ctrl Pts',(-0.701931372739155,-0.958862495626329,
57.0603403424805));
#40671=CARTESIAN_POINT('Ctrl Pts',(-0.542832141253469,-1.07533043807677,
57.0682654642462));
#40672=CARTESIAN_POINT('Ctrl Pts',(-0.354120886132576,-1.1513473336213,
57.0761905860119));
#40673=CARTESIAN_POINT('Ctrl Pts',(-0.158714042031886,-1.17768195639405,
57.0841157077776));
#40674=CARTESIAN_POINT('Ctrl Pts',(0.0366928020688043,-1.20401657916681,
57.0920408295433));
#40675=CARTESIAN_POINT('Ctrl Pts',(0.238795235149295,-1.18066892916778,
57.0999659513091));
#40676=CARTESIAN_POINT('Ctrl Pts',(0.42305064474897,-1.11047426333603,57.1078910730748));
#40677=CARTESIAN_POINT('Ctrl Pts',(0.607306054348645,-1.04027959750429,
57.1158161948405));
#40678=CARTESIAN_POINT('Ctrl Pts',(0.773714440467504,-0.923237915839822,
57.1237413166062));
#40679=CARTESIAN_POINT('Ctrl Pts',(0.902067750839875,-0.773562350718361,
57.1316664383719));
#40680=CARTESIAN_POINT('Ctrl Pts',(1.03042106121224,-0.623886785596901,
57.1395915601377));
#40681=CARTESIAN_POINT('Ctrl Pts',(1.12071929583812,-0.441577337018447,
57.1475166819034));
#40682=CARTESIAN_POINT('Ctrl Pts',(1.16199695299385,-0.248773026647261,
57.1554418036691));
#40683=CARTESIAN_POINT('Ctrl Pts',(1.20327461014957,-0.0559687162760749,
57.1633669254348));
#40684=CARTESIAN_POINT('Ctrl Pts',(1.19553168983515,0.147330455887844,57.1712920472006));
#40685=CARTESIAN_POINT('Ctrl Pts',(1.13970846520658,0.33643654957613,57.1792171689663));
#40686=CARTESIAN_POINT('Ctrl Pts',(1.08388524057801,0.525542643264417,57.187142290732));
#40687=CARTESIAN_POINT('Ctrl Pts',(0.979981711635303,0.700455658477069,
57.1950674124977));
#40688=CARTESIAN_POINT('Ctrl Pts',(0.840615559448702,0.839934770542912,
57.2029925342634));
#40689=CARTESIAN_POINT('Ctrl Pts',(0.701249407262101,0.979413882608754,
57.2109176560291));
#40690=CARTESIAN_POINT('Ctrl Pts',(0.526420631831606,1.08345909152779,57.2188427777948));
#40691=CARTESIAN_POINT('Ctrl Pts',(0.33735982804395,1.13943551110907,57.2267678995606));
#40692=CARTESIAN_POINT('Ctrl Pts',(0.14829902425629,1.19541193069035,57.2346930213263));
#40693=CARTESIAN_POINT('Ctrl Pts',(-0.0549938078885346,1.20331956093389,
57.242618143092));
#40694=CARTESIAN_POINT('Ctrl Pts',(-0.247831498031896,1.16219812688607,
57.2505432648577));
#40695=CARTESIAN_POINT('Ctrl Pts',(-0.440669188175249,1.12107669283826,
57.2584683866234));
#40696=CARTESIAN_POINT('Ctrl Pts',(-0.623051736317142,1.0309261944991,57.2663935083891));
#40697=CARTESIAN_POINT('Ctrl Pts',(-0.772831243838051,0.902694193014421,
57.2743186301549));
#40698=CARTESIAN_POINT('Ctrl Pts',(-0.922610751358966,0.774462191529739,
57.2822437519206));
#40699=CARTESIAN_POINT('Ctrl Pts',(-1.03978721825889,0.608148686899538,
57.2901688736863));
#40700=CARTESIAN_POINT('Ctrl Pts',(-1.11013114431464,0.423950209313431,
57.298093995452));
#40701=CARTESIAN_POINT('Ctrl Pts',(-1.16166524725872,0.28900603092703,57.3038999557363));
#40702=CARTESIAN_POINT('Ctrl Pts',(-1.18806405705757,0.144462885027062,
57.3097059160205));
#40703=CARTESIAN_POINT('Ctrl Pts',(-1.18820495619059,-3.01830341203513E-5,
57.3155118763048));
#40704=CARTESIAN_POINT('Origin',(0.,0.,57.95));
#40705=CARTESIAN_POINT('',(-1.18818092497865,2.78399633203974E-5,57.6580381236952));
#40706=CARTESIAN_POINT('',(-1.18816109645034,2.38868568558623E-5,57.6155118763048));
#40707=CARTESIAN_POINT('',(-1.188225,-1.45515594291686E-16,57.95));
#40708=CARTESIAN_POINT('Ctrl Pts',(-1.18818092497865,2.78399633203974E-5,
57.6580381236952));
#40709=CARTESIAN_POINT('Ctrl Pts',(-1.18823417132103,0.0611879018643663,
57.6555807582517));
#40710=CARTESIAN_POINT('Ctrl Pts',(-1.18359441363642,0.122339960905958,
57.6531233928081));
#40711=CARTESIAN_POINT('Ctrl Pts',(-1.17419209887383,0.18275077751389,57.6506660273646));
#40712=CARTESIAN_POINT('Ctrl Pts',(-1.14386918147067,0.377578567107811,
57.6427409055989));
#40713=CARTESIAN_POINT('Ctrl Pts',(-1.06401121614902,0.564696742125061,
57.6348157838332));
#40714=CARTESIAN_POINT('Ctrl Pts',(-0.944315874851311,0.721382325984963,
57.6268906620675));
#40715=CARTESIAN_POINT('Ctrl Pts',(-0.824620533553604,0.878067909844868,
57.6189655403018));
#40716=CARTESIAN_POINT('Ctrl Pts',(-0.665087816279843,1.00432090254743,
57.611040418536));
#40717=CARTESIAN_POINT('Ctrl Pts',(-0.485090818124233,1.08480958232827,
57.6031152967703));
#40718=CARTESIAN_POINT('Ctrl Pts',(-0.305093819968621,1.16529826210911,
57.5951901750046));
#40719=CARTESIAN_POINT('Ctrl Pts',(-0.104632540931167,1.20002262896824,
57.5872650532389));
#40720=CARTESIAN_POINT('Ctrl Pts',(0.0919497025332866,1.18476587727015,
57.5793399314732));
#40721=CARTESIAN_POINT('Ctrl Pts',(0.288531945997738,1.16950912557206,57.5714148097074));
#40722=CARTESIAN_POINT('Ctrl Pts',(0.481235153889179,1.10427125531675,57.5634896879417));
#40723=CARTESIAN_POINT('Ctrl Pts',(0.646658122772754,0.996974525247105,
57.555564566176));
#40724=CARTESIAN_POINT('Ctrl Pts',(0.812081091656327,0.889677795177463,
57.5476394444103));
#40725=CARTESIAN_POINT('Ctrl Pts',(0.950223821532038,0.740322205293489,
57.5397143226446));
#40726=CARTESIAN_POINT('Ctrl Pts',(1.04431074254694,0.567044975941711,57.5317892008789));
#40727=CARTESIAN_POINT('Ctrl Pts',(1.13839766356184,0.39376774658993,57.5238640791131));
#40728=CARTESIAN_POINT('Ctrl Pts',(1.18842877571593,0.19656887777034,57.5159389573474));
#40729=CARTESIAN_POINT('Ctrl Pts',(1.18832847577251,-0.000604489746206457,
57.5080138355817));
#40730=CARTESIAN_POINT('Ctrl Pts',(1.18822817582909,-0.197777857262752,
57.500088713816));
#40731=CARTESIAN_POINT('Ctrl Pts',(1.13799646378815,-0.394925723476249,
57.4921635920503));
#40732=CARTESIAN_POINT('Ctrl Pts',(1.0437333030349,-0.568107141193917,57.4842384702846));
#40733=CARTESIAN_POINT('Ctrl Pts',(0.949470142281659,-0.741288558911583,
57.4763133485188));
#40734=CARTESIAN_POINT('Ctrl Pts',(0.811175532816112,-0.890503528133416,
57.4683882267531));
#40735=CARTESIAN_POINT('Ctrl Pts',(0.645643488217273,-0.997631904994174,
57.4604631049874));
#40736=CARTESIAN_POINT('Ctrl Pts',(0.480111443618431,-1.10476028185493,
57.4525379832217));
#40737=CARTESIAN_POINT('Ctrl Pts',(0.287341963886296,-1.16980206635462,
57.444612861456));
#40738=CARTESIAN_POINT('Ctrl Pts',(0.0907443002762212,-1.18485881171853,
57.4366877396902));
#40739=CARTESIAN_POINT('Ctrl Pts',(-0.105853363333853,-1.19991555708245,
57.4287626179245));
#40740=CARTESIAN_POINT('Ctrl Pts',(-0.306279210821867,-1.16498726331059,
57.4208374961588));
#40741=CARTESIAN_POINT('Ctrl Pts',(-0.486194228416377,-1.08431550020936,
57.4129123743931));
#40742=CARTESIAN_POINT('Ctrl Pts',(-0.666109246010887,-1.00364373710813,
57.4049872526274));
#40743=CARTESIAN_POINT('Ctrl Pts',(-0.825513433711893,-0.877228504677525,
57.3970621308616));
#40744=CARTESIAN_POINT('Ctrl Pts',(-0.945049304606873,-0.720421226506923,
57.3891370090959));
#40745=CARTESIAN_POINT('Ctrl Pts',(-1.06458517550185,-0.563613948336321,
57.3812118873302));
#40746=CARTESIAN_POINT('Ctrl Pts',(-1.14425272959081,-0.376414624425722,
57.3732867655645));
#40747=CARTESIAN_POINT('Ctrl Pts',(-1.17437741780528,-0.181556085793528,
57.3653616437988));
#40748=CARTESIAN_POINT('Ctrl Pts',(-1.18365671833321,-0.121533856599753,
57.3629204704309));
#40749=CARTESIAN_POINT('Ctrl Pts',(-1.18823527611343,-0.0607849032365112,
57.360479297063));
#40750=CARTESIAN_POINT('Ctrl Pts',(-1.1881820096365,-2.79964409908851E-5,
57.3580381236952));
#40751=CARTESIAN_POINT('Ctrl Pts',(-1.18820495619059,-3.01830341203513E-5,
57.3155118763048));
#40752=CARTESIAN_POINT('Ctrl Pts',(-1.18825638403385,-0.0527698039030566,
57.3176310377863));
#40753=CARTESIAN_POINT('Ctrl Pts',(-1.18480964802288,-0.10550275324021,
57.3197501992677));
#40754=CARTESIAN_POINT('Ctrl Pts',(-1.17781015957882,-0.157759835025051,
57.3218693607492));
#40755=CARTESIAN_POINT('Ctrl Pts',(-1.15163386357572,-0.353187951235413,
57.3297944825149));
#40756=CARTESIAN_POINT('Ctrl Pts',(-1.07576988635795,-0.541960733114136,
57.3377196042806));
#40757=CARTESIAN_POINT('Ctrl Pts',(-0.959430883924738,-0.701154274411576,
57.3456447260463));
#40758=CARTESIAN_POINT('Ctrl Pts',(-0.843091881491527,-0.860347815709018,
57.3535698478121));
#40759=CARTESIAN_POINT('Ctrl Pts',(-0.686277853842878,-0.989962116425177,
57.3614949695778));
#40760=CARTESIAN_POINT('Ctrl Pts',(-0.508031747915679,-1.07425726930934,
57.3694200913435));
#40761=CARTESIAN_POINT('Ctrl Pts',(-0.329785641988481,-1.15855242219351,
57.3773452131092));
#40762=CARTESIAN_POINT('Ctrl Pts',(-0.130107457782735,-1.19752842724568,
57.385270334875));
#40763=CARTESIAN_POINT('Ctrl Pts',(0.0667545845435723,-1.18645217476165,
57.3931954566407));
#40764=CARTESIAN_POINT('Ctrl Pts',(0.263616626869876,-1.17537592227761,
57.4011205784064));
#40765=CARTESIAN_POINT('Ctrl Pts',(0.457662527316743,-1.11424741225737,
57.4090457001721));
#40766=CARTESIAN_POINT('Ctrl Pts',(0.625328030562507,-1.0104898771126,57.4169708219378));
#40767=CARTESIAN_POINT('Ctrl Pts',(0.792993533808274,-0.90673234196783,
57.4248959437035));
#40768=CARTESIAN_POINT('Ctrl Pts',(0.934278639852939,-0.760345781698527,
57.4328210654692));
#40769=CARTESIAN_POINT('Ctrl Pts',(1.03202617967454,-0.589106868081328,
57.440746187235));
#40770=CARTESIAN_POINT('Ctrl Pts',(1.12977371949615,-0.417867954464128,
57.4486713090007));
#40771=CARTESIAN_POINT('Ctrl Pts',(1.1839836930947,-0.221776687499036,57.4565964307664));
#40772=CARTESIAN_POINT('Ctrl Pts',(1.18807303091852,-0.0246457046624006,
57.4645215525321));
#40773=CARTESIAN_POINT('Ctrl Pts',(1.19216236874234,0.172485278174231,57.4724466742978));
#40774=CARTESIAN_POINT('Ctrl Pts',(1.14613107079145,0.370655976882405,57.4803717960636));
#40775=CARTESIAN_POINT('Ctrl Pts',(1.05556901685821,0.545801235069337,57.4882969178293));
#40776=CARTESIAN_POINT('Ctrl Pts',(0.965006962924976,0.720946493256271,
57.496222039595));
#40777=CARTESIAN_POINT('Ctrl Pts',(0.829914153009402,0.873066310921964,
57.5041471613607));
#40778=CARTESIAN_POINT('Ctrl Pts',(0.666695785353968,0.983687789568155,
57.5120722831264));
#40779=CARTESIAN_POINT('Ctrl Pts',(0.503477417698534,1.09430926821435,57.5199974048921));
#40780=CARTESIAN_POINT('Ctrl Pts',(0.312133492303237,1.16343240784103,57.5279225266578));
#40781=CARTESIAN_POINT('Ctrl Pts',(0.115900146091773,1.18266313618466,57.5358476484236));
#40782=CARTESIAN_POINT('Ctrl Pts',(-0.0803332001196921,1.20189386452828,
57.5437727701893));
#40783=CARTESIAN_POINT('Ctrl Pts',(-0.281455967147326,1.17123218158885,
57.551697891955));
#40784=CARTESIAN_POINT('Ctrl Pts',(-0.463044509748822,1.09440153487909,
57.5596230137207));
#40785=CARTESIAN_POINT('Ctrl Pts',(-0.644633052350318,1.01757088816933,
57.5675481354864));
#40786=CARTESIAN_POINT('Ctrl Pts',(-0.806687370525673,0.89457127768925,
57.5754732572522));
#40787=CARTESIAN_POINT('Ctrl Pts',(-0.929528154788486,0.740339345847389,
57.5833983790179));
#40788=CARTESIAN_POINT('Ctrl Pts',(-1.0523689390513,0.58610741400553,57.5913235007836));
#40789=CARTESIAN_POINT('Ctrl Pts',(-1.13599618940157,0.400643160801886,
57.5992486225493));
#40790=CARTESIAN_POINT('Ctrl Pts',(-1.17025450510903,0.206468716337991,
57.607173744315));
#40791=CARTESIAN_POINT('Ctrl Pts',(-1.18226905691703,0.13837082901852,57.609953121645));
#40792=CARTESIAN_POINT('Ctrl Pts',(-1.18821153704315,0.0692016423874921,
57.6127324989749));
#40793=CARTESIAN_POINT('Ctrl Pts',(-1.18816109645034,2.38868568558623E-5,
57.6155118763048));
#40794=CARTESIAN_POINT('Origin',(0.,0.,57.95));
#40795=CARTESIAN_POINT('',(-1.18831445454319,-1.42653502743784E-5,57.9580381236952));
#40796=CARTESIAN_POINT('',(-1.18832572782012,-6.43342140850944E-6,57.9155118763048));
#40797=CARTESIAN_POINT('',(-1.188225,-1.45515594291686E-16,57.95));
#40798=CARTESIAN_POINT('Ctrl Pts',(-1.18831445454319,-1.42653502743784E-5,
57.9580381236952));
#40799=CARTESIAN_POINT('Ctrl Pts',(-1.18820367858962,0.183003608488043,
57.9506822194403));
#40800=CARTESIAN_POINT('Ctrl Pts',(-1.14525528855688,0.366071677622651,
57.9433263151854));
#40801=CARTESIAN_POINT('Ctrl Pts',(-1.06364953455008,0.529881684332512,
57.9359704109305));
#40802=CARTESIAN_POINT('Ctrl Pts',(-0.975728931606305,0.706367702180658,
57.9280452891648));
#40803=CARTESIAN_POINT('Ctrl Pts',(-0.842936683969155,0.860499869539008,
57.920120167399));
#40804=CARTESIAN_POINT('Ctrl Pts',(-0.681398617646076,0.973560915202376,
57.9121950456333));
#40805=CARTESIAN_POINT('Ctrl Pts',(-0.519860551322997,1.08662196086574,
57.9042699238676));
#40806=CARTESIAN_POINT('Ctrl Pts',(-0.329576666313986,1.15861188483414,
57.8963448021019));
#40807=CARTESIAN_POINT('Ctrl Pts',(-0.133654371946536,1.1807884825824,57.8884196803362));
#40808=CARTESIAN_POINT('Ctrl Pts',(0.0622679224209139,1.20296508033066,
57.8804945585704));
#40809=CARTESIAN_POINT('Ctrl Pts',(0.263828626146796,1.17532835185877,57.8725694368047));
#40810=CARTESIAN_POINT('Ctrl Pts',(0.446550912488195,1.10123440479111,57.864644315039));
#40811=CARTESIAN_POINT('Ctrl Pts',(0.629273198829594,1.02714045772345,57.8567191932733));
#40812=CARTESIAN_POINT('Ctrl Pts',(0.793157067786511,0.90658929206001,57.8487940715076));
#40813=CARTESIAN_POINT('Ctrl Pts',(0.918301035625923,0.754220219636168,
57.8408689497419));
#40814=CARTESIAN_POINT('Ctrl Pts',(1.04344500346533,0.601851147212326,57.8329438279761));
#40815=CARTESIAN_POINT('Ctrl Pts',(1.12984907018724,0.417664168028081,57.8250187062104));
#40816=CARTESIAN_POINT('Ctrl Pts',(1.16702062819532,0.224026304496317,57.8170935844447));
#40817=CARTESIAN_POINT('Ctrl Pts',(1.20419218620339,0.0303884409645555,
57.809168462679));
#40818=CARTESIAN_POINT('Ctrl Pts',(1.19213123549764,-0.172700306914724,
57.8012433409133));
#40819=CARTESIAN_POINT('Ctrl Pts',(1.13230241573907,-0.360577552062159,
57.7933182191476));
#40820=CARTESIAN_POINT('Ctrl Pts',(1.0724735959805,-0.548454797209594,57.7853930973818));
#40821=CARTESIAN_POINT('Ctrl Pts',(0.96487690716912,-0.721120539625185,
57.7774679756161));
#40822=CARTESIAN_POINT('Ctrl Pts',(0.822578514789886,-0.857606855584618,
57.7695428538504));
#40823=CARTESIAN_POINT('Ctrl Pts',(0.680280122410652,-0.994093171544052,
57.7616177320847));
#40824=CARTESIAN_POINT('Ctrl Pts',(0.503280026463566,-1.09440006104733,
57.753692610319));
#40825=CARTESIAN_POINT('Ctrl Pts',(0.313072499402984,-1.14634660633564,
57.7457674885532));
#40826=CARTESIAN_POINT('Ctrl Pts',(0.122864972342397,-1.19829315162395,
57.7378423667875));
#40827=CARTESIAN_POINT('Ctrl Pts',(-0.0805499858316875,-1.2018793526973,
57.7299172450218));
#40828=CARTESIAN_POINT('Ctrl Pts',(-0.27247037420288,-1.1566697138429,57.7219921232561));
#40829=CARTESIAN_POINT('Ctrl Pts',(-0.464390762574071,-1.1114600749885,
57.7140670014904));
#40830=CARTESIAN_POINT('Ctrl Pts',(-0.64481658114237,-1.01745459620635,
57.7061418797247));
#40831=CARTESIAN_POINT('Ctrl Pts',(-0.791837549682469,-0.886068973981448,
57.6982167579589));
#40832=CARTESIAN_POINT('Ctrl Pts',(-0.938858518222567,-0.754683351756544,
57.6902916361932));
#40833=CARTESIAN_POINT('Ctrl Pts',(-1.05247463673446,-0.585917586088883,
57.6823665144275));
#40834=CARTESIAN_POINT('Ctrl Pts',(-1.11888876124807,-0.400266001169753,
57.6744413926618));
#40835=CARTESIAN_POINT('Ctrl Pts',(-1.16470966595187,-0.272179940516427,
57.6689736363396));
#40836=CARTESIAN_POINT('Ctrl Pts',(-1.18806244930546,-0.136056239841935,
57.6635058800174));
#40837=CARTESIAN_POINT('Ctrl Pts',(-1.18818092497865,2.78399633203974E-5,
57.6580381236952));
#40838=CARTESIAN_POINT('Ctrl Pts',(-1.18816109645034,2.38868568558623E-5,
57.6155118763048));
#40839=CARTESIAN_POINT('Ctrl Pts',(-1.18806771064159,-0.128051940332391,
57.6206576207406));
#40840=CARTESIAN_POINT('Ctrl Pts',(-1.16743245670349,-0.256157139044143,
57.6258033651764));
#40841=CARTESIAN_POINT('Ctrl Pts',(-1.12675762900519,-0.377547590421175,
57.6309491096122));
#40842=CARTESIAN_POINT('Ctrl Pts',(-1.06411305612924,-0.56450481699229,
57.6388742313779));
#40843=CARTESIAN_POINT('Ctrl Pts',(-0.953934529312678,-0.735534634410373,
57.6467993531436));
#40844=CARTESIAN_POINT('Ctrl Pts',(-0.809601743415808,-0.869867779959869,
57.6547244749094));
#40845=CARTESIAN_POINT('Ctrl Pts',(-0.665268957518935,-1.00420092550937,
57.6626495966751));
#40846=CARTESIAN_POINT('Ctrl Pts',(-0.486781912541746,-1.10183739919028,
57.6705747184408));
#40847=CARTESIAN_POINT('Ctrl Pts',(-0.295815450827041,-1.15092056919938,
57.6784998402065));
#40848=CARTESIAN_POINT('Ctrl Pts',(-0.104848989112345,-1.20000373920847,
57.6864249619722));
#40849=CARTESIAN_POINT('Ctrl Pts',(0.0985968893398703,-1.20053360554576,
57.6943500837379));
#40850=CARTESIAN_POINT('Ctrl Pts',(0.289816428762806,-1.15244582309686,
57.7022752055036));
#40851=CARTESIAN_POINT('Ctrl Pts',(0.481035968185751,-1.10435804064796,
57.7102003272694));
#40852=CARTESIAN_POINT('Ctrl Pts',(0.660029168579411,-1.00765260941287,
57.7181254490351));
#40853=CARTESIAN_POINT('Ctrl Pts',(0.805059721857905,-0.874073098657258,
57.7260505708008));
#40854=CARTESIAN_POINT('Ctrl Pts',(0.950090275136396,-0.740493587901643,
57.7339756925665));
#40855=CARTESIAN_POINT('Ctrl Pts',(1.06115818129972,-0.5700399976255,57.7419008143322));
#40856=CARTESIAN_POINT('Ctrl Pts',(1.124775742371,-0.383411615536077,57.749825936098));
#40857=CARTESIAN_POINT('Ctrl Pts',(1.18839330344229,-0.196783233446657,
57.7577510578637));
#40858=CARTESIAN_POINT('Ctrl Pts',(1.20456051942155,0.0060199404560462,
57.7656761796294));
#40859=CARTESIAN_POINT('Ctrl Pts',(1.17131410015784,0.200370198197361,57.7736013013951));
#40860=CARTESIAN_POINT('Ctrl Pts',(1.13806768089414,0.394720455938679,57.7815264231608));
#40861=CARTESIAN_POINT('Ctrl Pts',(1.05540762638747,0.580617797518612,57.7894515449266));
#40862=CARTESIAN_POINT('Ctrl Pts',(0.93337188448839,0.735487500098281,57.7973766666923));
#40863=CARTESIAN_POINT('Ctrl Pts',(0.811336142589308,0.890357202677951,
57.805301788458));
#40864=CARTESIAN_POINT('Ctrl Pts',(0.649924713297808,1.01419926625736,57.8132269102237));
#40865=CARTESIAN_POINT('Ctrl Pts',(0.468738835923253,1.09197474387073,57.8211520319894));
#40866=CARTESIAN_POINT('Ctrl Pts',(0.287552958548701,1.1697502214841,57.8290771537551));
#40867=CARTESIAN_POINT('Ctrl Pts',(0.0865926330910932,1.20145911313143,
57.8370022755208));
#40868=CARTESIAN_POINT('Ctrl Pts',(-0.109738221543257,1.18325080193793,
57.8449273972866));
#40869=CARTESIAN_POINT('Ctrl Pts',(-0.30606907617761,1.16504249074443,57.8528525190523));
#40870=CARTESIAN_POINT('Ctrl Pts',(-0.4977704599887,1.09691697671011,57.860777640818));
#40871=CARTESIAN_POINT('Ctrl Pts',(-0.661562827553329,0.987147183936556,
57.8687027625837));
#40872=CARTESIAN_POINT('Ctrl Pts',(-0.82535519511796,0.877377391163003,
57.8766278843495));
#40873=CARTESIAN_POINT('Ctrl Pts',(-0.961238546436123,0.725963319650224,
57.8845530061152));
#40874=CARTESIAN_POINT('Ctrl Pts',(-1.05271168268295,0.551292164552578,
57.8924781278809));
#40875=CARTESIAN_POINT('Ctrl Pts',(-1.14133152854122,0.382069467313122,
57.9001560440222));
#40876=CARTESIAN_POINT('Ctrl Pts',(-1.18826849441849,0.191017958341526,
57.9078339601635));
#40877=CARTESIAN_POINT('Ctrl Pts',(-1.18832572782012,-6.43342140850944E-6,
57.9155118763048));
#40878=CARTESIAN_POINT('Origin',(0.,0.,57.95));
#40879=CARTESIAN_POINT('',(-1.18812981577958,-8.35218226485912E-6,58.2580381236952));
#40880=CARTESIAN_POINT('',(-1.18813848747178,-1.51983744768193E-5,58.2155118763048));
#40881=CARTESIAN_POINT('',(-1.188225,-1.45515594291686E-16,57.95));
#40882=CARTESIAN_POINT('Ctrl Pts',(-1.18812981577958,-8.35218226485912E-6,
58.2580381236952));
#40883=CARTESIAN_POINT('Ctrl Pts',(-1.18810326726687,0.107755104213723,
58.2537088023946));
#40884=CARTESIAN_POINT('Ctrl Pts',(-1.17357378535918,0.215525578981994,
58.2493794810941));
#40885=CARTESIAN_POINT('Ctrl Pts',(-1.14463417372155,0.319276588694579,
58.2450501597935));
#40886=CARTESIAN_POINT('Ctrl Pts',(-1.09165821509935,0.509199980423857,
58.2371250380278));
#40887=CARTESIAN_POINT('Ctrl Pts',(-0.990394153790361,0.685654212264053,
58.229199916262));
#40888=CARTESIAN_POINT('Ctrl Pts',(-0.853139143149014,0.827211299588345,
58.2212747944963));
#40889=CARTESIAN_POINT('Ctrl Pts',(-0.715884132507665,0.968768386912637,
58.2133496727306));
#40890=CARTESIAN_POINT('Ctrl Pts',(-0.542638172533966,1.07542832972103,
58.2054245509649));
#40891=CARTESIAN_POINT('Ctrl Pts',(-0.354439646542703,1.13423871768616,
58.1974994291992));
#40892=CARTESIAN_POINT('Ctrl Pts',(-0.16624112055144,1.1930491056513,58.1895743074335));
#40893=CARTESIAN_POINT('Ctrl Pts',(0.0369099714573795,1.20400993877317,
58.1816491856678));
#40894=CARTESIAN_POINT('Ctrl Pts',(0.230343671551399,1.16579017182162,58.173724063902));
#40895=CARTESIAN_POINT('Ctrl Pts',(0.423777371645419,1.12757040487008,58.1657989421363));
#40896=CARTESIAN_POINT('Ctrl Pts',(0.607493679824638,1.0401700378451,58.1578738203706));
#40897=CARTESIAN_POINT('Ctrl Pts',(0.759182730316479,0.914202665566497,
58.1499486986049));
#40898=CARTESIAN_POINT('Ctrl Pts',(0.910871780808321,0.788235293287889,
58.1420235768392));
#40899=CARTESIAN_POINT('Ctrl Pts',(1.03053357361278,0.623700915755645,58.1340984550734));
#40900=CARTESIAN_POINT('Ctrl Pts',(1.10363679922321,0.440580012188506,58.1261733333077));
#40901=CARTESIAN_POINT('Ctrl Pts',(1.17674002483363,0.257459108621373,58.118248211542));
#40902=CARTESIAN_POINT('Ctrl Pts',(1.20328468325001,0.0557516790193457,
58.1103230897763));
#40903=CARTESIAN_POINT('Ctrl Pts',(1.18004728401516,-0.140047631997551,
58.1023979680106));
#40904=CARTESIAN_POINT('Ctrl Pts',(1.1568098847803,-0.335846943014454,58.0944728462449));
#40905=CARTESIAN_POINT('Ctrl Pts',(1.0837904278942,-0.525738135446225,58.0865477244791));
#40906=CARTESIAN_POINT('Ctrl Pts',(0.969856140757953,-0.686661487178189,
58.0786226027134));
#40907=CARTESIAN_POINT('Ctrl Pts',(0.855921853621706,-0.847584838910152,
58.0706974809477));
#40908=CARTESIAN_POINT('Ctrl Pts',(0.701072736235314,-0.979540349942306,
58.062772359182));
#40909=CARTESIAN_POINT('Ctrl Pts',(0.524113123707244,-1.0665038046334,58.0548472374163));
#40910=CARTESIAN_POINT('Ctrl Pts',(0.347153511179174,-1.15346725932448,
58.0469221156505));
#40911=CARTESIAN_POINT('Ctrl Pts',(0.148083403509426,-1.19543865767451,
58.0389969938848));
#40912=CARTESIAN_POINT('Ctrl Pts',(-0.0489228218313184,-1.18732113989591,
58.0310718721191));
#40913=CARTESIAN_POINT('Ctrl Pts',(-0.245929047172062,-1.17920362211732,
58.0231467503534));
#40914=CARTESIAN_POINT('Ctrl Pts',(-0.440871390183802,-1.12099718821011,
58.0152216285877));
#40915=CARTESIAN_POINT('Ctrl Pts',(-0.610076734695811,-1.01977022388505,
58.007296506822));
#40916=CARTESIAN_POINT('Ctrl Pts',(-0.779282079207818,-0.918543259559998,
57.9993713850562));
#40917=CARTESIAN_POINT('Ctrl Pts',(-0.922750425220095,-0.774295764817101,
57.9914462632905));
#40918=CARTESIAN_POINT('Ctrl Pts',(-1.02305947868662,-0.604544650798541,
57.9835211415248));
#40919=CARTESIAN_POINT('Ctrl Pts',(-1.12336853215315,-0.434793536779981,
57.9755960197591));
#40920=CARTESIAN_POINT('Ctrl Pts',(-1.18051829307393,-0.239538803485758,
57.9676708979934));
#40921=CARTESIAN_POINT('Ctrl Pts',(-1.1875686944091,-0.0424915026696703,
57.9597457762276));
#40922=CARTESIAN_POINT('Ctrl Pts',(-1.18807508560623,-0.0283386886939873,
57.9591765587168));
#40923=CARTESIAN_POINT('Ctrl Pts',(-1.18832302665212,-0.0141766273077396,
57.958607341206));
#40924=CARTESIAN_POINT('Ctrl Pts',(-1.18831445454319,-1.42653502743784E-5,
57.9580381236952));
#40925=CARTESIAN_POINT('Ctrl Pts',(-1.18832572782012,-6.43342140850944E-6,
57.9155118763048));
#40926=CARTESIAN_POINT('Ctrl Pts',(-1.18832757056215,-0.00615683975214519,
57.9157590819292));
#40927=CARTESIAN_POINT('Ctrl Pts',(-1.18828081567409,-0.012307217971969,
57.9160062875536));
#40928=CARTESIAN_POINT('Ctrl Pts',(-1.18818528970154,-0.0184568385994857,
57.916253493178));
#40929=CARTESIAN_POINT('Ctrl Pts',(-1.18512283929783,-0.215606447971398,
57.9241786149437));
#40930=CARTESIAN_POINT('Ctrl Pts',(-1.13193501731493,-0.411977428032717,
57.9321037367095));
#40931=CARTESIAN_POINT('Ctrl Pts',(-1.03508076678807,-0.583723173927203,
57.9400288584752));
#40932=CARTESIAN_POINT('Ctrl Pts',(-0.938226516261208,-0.755468919821696,
57.9479539802409));
#40933=CARTESIAN_POINT('Ctrl Pts',(-0.797705837190388,-0.902589431549353,
57.9558791020066));
#40934=CARTESIAN_POINT('Ctrl Pts',(-0.630583069260051,-1.00721890883601,
57.9638042237723));
#40935=CARTESIAN_POINT('Ctrl Pts',(-0.463460301329717,-1.11184838612266,
57.9717293455381));
#40936=CARTESIAN_POINT('Ctrl Pts',(-0.269735444539866,-1.17398682896832,
57.9796544673038));
#40937=CARTESIAN_POINT('Ctrl Pts',(-0.0729337677935576,-1.18608836225201,
57.9875795890695));
#40938=CARTESIAN_POINT('Ctrl Pts',(0.123867908952751,-1.19818989553571,
57.9955047108352));
#40939=CARTESIAN_POINT('Ctrl Pts',(0.323746405655516,-1.16025451925745,
58.0034298326009));
#40940=CARTESIAN_POINT('Ctrl Pts',(0.502429176907867,-1.07688897280356,
58.0113549543667));
#40941=CARTESIAN_POINT('Ctrl Pts',(0.681111948160215,-0.993523426349675,
58.0192800761324));
#40942=CARTESIAN_POINT('Ctrl Pts',(0.838598993962152,-0.864727709720157,
58.0272051978981));
#40943=CARTESIAN_POINT('Ctrl Pts',(0.955765638406653,-0.706142324177889,
58.0351303196638));
#40944=CARTESIAN_POINT('Ctrl Pts',(1.07293228285115,-0.547556938635621,
58.0430554414295));
#40945=CARTESIAN_POINT('Ctrl Pts',(1.14977852593822,-0.359181884180608,
58.0509805631953));
#40946=CARTESIAN_POINT('Ctrl Pts',(1.17697242873772,-0.163892768435502,
58.058905684961));
#40947=CARTESIAN_POINT('Ctrl Pts',(1.20416633153722,0.0313963473096032,
58.0668308067267));
#40948=CARTESIAN_POINT('Ctrl Pts',(1.18170789404915,0.2335995243448,58.0747559284924));
#40949=CARTESIAN_POINT('Ctrl Pts',(1.11232439035596,0.418161916216034,58.0826810502581));
#40950=CARTESIAN_POINT('Ctrl Pts',(1.04294088666277,0.60272430808727,58.0906061720238));
#40951=CARTESIAN_POINT('Ctrl Pts',(0.926632316764456,0.769645914794549,
58.0985312937895));
#40952=CARTESIAN_POINT('Ctrl Pts',(0.777522786508502,0.898656360359332,
58.1064564155553));
#40953=CARTESIAN_POINT('Ctrl Pts',(0.628413256252548,1.02766680592411,58.114381537321));
#40954=CARTESIAN_POINT('Ctrl Pts',(0.446502765638955,1.1187660903464,58.1223066590867));
#40955=CARTESIAN_POINT('Ctrl Pts',(0.253881888272399,1.16089143521755,58.1302317808524));
#40956=CARTESIAN_POINT('Ctrl Pts',(0.0612610109058417,1.20301678008871,
58.1381569026181));
#40957=CARTESIAN_POINT('Ctrl Pts',(-0.142070253213676,1.19616818540873,
58.1460820243839));
#40958=CARTESIAN_POINT('Ctrl Pts',(-0.331420066682969,1.14117732055719,
58.1540071461496));
#40959=CARTESIAN_POINT('Ctrl Pts',(-0.520769880152256,1.08618645570565,
58.1619322679153));
#40960=CARTESIAN_POINT('Ctrl Pts',(-0.696138242971318,0.983053320682559,
58.169857389681));
#40961=CARTESIAN_POINT('Ctrl Pts',(-0.836229034648592,0.844302042615622,
58.1777825114468));
#40962=CARTESIAN_POINT('Ctrl Pts',(-0.976319826325865,0.705550764548685,
58.1857076332125));
#40963=CARTESIAN_POINT('Ctrl Pts',(-1.08113304686135,0.531181343437903,
58.1936327549782));
#40964=CARTESIAN_POINT('Ctrl Pts',(-1.13794054542014,0.342368591788372,
58.2015578767439));
#40965=CARTESIAN_POINT('Ctrl Pts',(-1.17128143419471,0.231552500397665,
58.2062092099309));
#40966=CARTESIAN_POINT('Ctrl Pts',(-1.18808611145214,0.115761211072918,
58.2108605431178));
#40967=CARTESIAN_POINT('Ctrl Pts',(-1.18813848747178,-1.51983744768193E-5,
58.2155118763048));
#40968=CARTESIAN_POINT('Origin',(0.,0.,57.95));
#40969=CARTESIAN_POINT('',(-1.18826810796675,2.71338473248756E-5,58.5580381236952));
#40970=CARTESIAN_POINT('',(-1.18824324986219,2.98497152091627E-5,58.5155118763048));
#40971=CARTESIAN_POINT('',(-1.188225,-1.45515594291686E-16,57.95));
#40972=CARTESIAN_POINT('Ctrl Pts',(-1.18826810796675,2.71338473248756E-5,
58.5580381236952));
#40973=CARTESIAN_POINT('Ctrl Pts',(-1.18829995724248,0.0324434506831562,
58.5567353853489));
#40974=CARTESIAN_POINT('Ctrl Pts',(-1.18699999162847,0.06485722040431,58.5554326470027));
#40975=CARTESIAN_POINT('Ctrl Pts',(-1.18434995694146,0.0971602348310493,
58.5541299086565));
#40976=CARTESIAN_POINT('Ctrl Pts',(-1.16822864782457,0.293673466727152,
58.5462047868908));
#40977=CARTESIAN_POINT('Ctrl Pts',(-1.1021437663709,0.486087848960798,58.538279665125));
#40978=CARTESIAN_POINT('Ctrl Pts',(-0.994120429400183,0.651037252074617,
58.5303545433593));
#40979=CARTESIAN_POINT('Ctrl Pts',(-0.886097092429467,0.815986655188435,
58.5224294215936));
#40980=CARTESIAN_POINT('Ctrl Pts',(-0.736135299941706,0.953471079182426,
58.5145042998279));
#40981=CARTESIAN_POINT('Ctrl Pts',(-0.562445887406952,1.04679489656698,
58.5065791780622));
#40982=CARTESIAN_POINT('Ctrl Pts',(-0.388756474872198,1.14011871395154,
58.4986540562965));
#40983=CARTESIAN_POINT('Ctrl Pts',(-0.191339442290451,1.18928192472666,
58.4907289345308));
#40984=CARTESIAN_POINT('Ctrl Pts',(0.00583157652335925,1.18831432056292,
58.4828038127651));
#40985=CARTESIAN_POINT('Ctrl Pts',(0.203002595337164,1.18734671639919,58.4748786909993));
#40986=CARTESIAN_POINT('Ctrl Pts',(0.399927600383042,1.1362482972966,58.4669535692336));
#40987=CARTESIAN_POINT('Ctrl Pts',(0.572692707948748,1.04122427651395,58.4590284474679));
#40988=CARTESIAN_POINT('Ctrl Pts',(0.745457815514457,0.946200255731301,
58.4511033257021));
#40989=CARTESIAN_POINT('Ctrl Pts',(0.894063025599998,0.807250633268592,
58.4431782039364));
#40990=CARTESIAN_POINT('Ctrl Pts',(1.00046224135654,0.641248965191775,58.4352530821707));
#40991=CARTESIAN_POINT('Ctrl Pts',(1.10686145711308,0.475247297114954,58.427327960405));
#40992=CARTESIAN_POINT('Ctrl Pts',(1.17105467854062,0.282193583424028,58.4194028386393));
#40993=CARTESIAN_POINT('Ctrl Pts',(1.18524650539542,0.0855315917519751,
58.4114777168736));
#40994=CARTESIAN_POINT('Ctrl Pts',(1.19943833225021,-0.111130399920075,
58.4035525951079));
#40995=CARTESIAN_POINT('Ctrl Pts',(1.16362876453227,-0.31140066957325,58.3956274733421));
#40996=CARTESIAN_POINT('Ctrl Pts',(1.08216639087305,-0.490959096264115,
58.3877023515764));
#40997=CARTESIAN_POINT('Ctrl Pts',(1.00070401721382,-0.670517522954981,
58.3797772298107));
#40998=CARTESIAN_POINT('Ctrl Pts',(0.873588837613317,-0.829364106683535,
58.371852108045));
#40999=CARTESIAN_POINT('Ctrl Pts',(0.716257274796604,-0.948209074013012,
58.3639269862793));
#41000=CARTESIAN_POINT('Ctrl Pts',(0.558925711979891,-1.06705404134249,
58.3560018645135));
#41001=CARTESIAN_POINT('Ctrl Pts',(0.371377765946969,-1.14589739227289,
58.3480767427478));
#41002=CARTESIAN_POINT('Ctrl Pts',(0.176388603167195,-1.17516466608403,
58.3401516209821));
#41003=CARTESIAN_POINT('Ctrl Pts',(-0.0186005596125763,-1.20443193989518,
58.3322264992164));
#41004=CARTESIAN_POINT('Ctrl Pts',(-0.2210309391392,-1.18412313658707,58.3243013774507));
#41005=CARTESIAN_POINT('Ctrl Pts',(-0.406320098282897,-1.11670448618739,
58.316376255685));
#41006=CARTESIAN_POINT('Ctrl Pts',(-0.591609257426595,-1.04928583578771,
58.3084511339192));
#41007=CARTESIAN_POINT('Ctrl Pts',(-0.759757196187365,-0.934757338296458,
58.3005260121535));
#41008=CARTESIAN_POINT('Ctrl Pts',(-0.890344617112157,-0.787026933795204,
58.2926008903878));
#41009=CARTESIAN_POINT('Ctrl Pts',(-1.02093203803695,-0.639296529293947,
58.2846757686221));
#41010=CARTESIAN_POINT('Ctrl Pts',(-1.11395894112576,-0.458364217782691,
58.2767506468564));
#41011=CARTESIAN_POINT('Ctrl Pts',(-1.15812846470246,-0.266201786217879,
58.2688255250906));
#41012=CARTESIAN_POINT('Ctrl Pts',(-1.17816914017951,-0.179013503030185,
58.2652297246255));
#41013=CARTESIAN_POINT('Ctrl Pts',(-1.18815186615369,-0.0895133484008016,
58.2616339241603));
#41014=CARTESIAN_POINT('Ctrl Pts',(-1.18812981577958,-8.35218226485912E-6,
58.2580381236952));
#41015=CARTESIAN_POINT('Ctrl Pts',(-1.18813848747178,-1.51983744768193E-5,
58.2155118763048));
#41016=CARTESIAN_POINT('Ctrl Pts',(-1.18817535174446,-0.0815031227393336,
58.2187856648836));
#41017=CARTESIAN_POINT('Ctrl Pts',(-1.17991331027786,-0.162983675776645,
58.2220594534623));
#41018=CARTESIAN_POINT('Ctrl Pts',(-1.16327701820942,-0.242716947204002,
58.2253332420411));
#41019=CARTESIAN_POINT('Ctrl Pts',(-1.12300421585783,-0.435733652358568,
58.2332583638068));
#41020=CARTESIAN_POINT('Ctrl Pts',(-1.03365683457257,-0.61851098047942,
58.2411834855725));
#41021=CARTESIAN_POINT('Ctrl Pts',(-0.906084907773975,-0.768853092247442,
58.2491086073382));
#41022=CARTESIAN_POINT('Ctrl Pts',(-0.778512980975379,-0.919195204015464,
58.2570337291039));
#41023=CARTESIAN_POINT('Ctrl Pts',(-0.612716508663446,-1.03710209943066,
58.2649588508696));
#41024=CARTESIAN_POINT('Ctrl Pts',(-0.428829234431794,-1.10825557758618,
58.2728839726354));
#41025=CARTESIAN_POINT('Ctrl Pts',(-0.244941960200139,-1.17940905574169,
58.2808090944011));
#41026=CARTESIAN_POINT('Ctrl Pts',(-0.0429638840487702,-1.20380911663754,
58.2887342161668));
#41027=CARTESIAN_POINT('Ctrl Pts',(0.152577483032149,-1.17849270223697,
58.2966593379325));
#41028=CARTESIAN_POINT('Ctrl Pts',(0.348118850113065,-1.15317628783641,
58.3045844596982));
#41029=CARTESIAN_POINT('Ctrl Pts',(0.537223508123526,-1.07814339813944,
58.312509581464));
#41030=CARTESIAN_POINT('Ctrl Pts',(0.69692724893745,-0.962505764784142,
58.3204347032297));
#41031=CARTESIAN_POINT('Ctrl Pts',(0.856630989751369,-0.846868131428849,
58.3283598249954));
#41032=CARTESIAN_POINT('Ctrl Pts',(0.986933813368754,-0.690625754415232,
58.3362849467611));
#41033=CARTESIAN_POINT('Ctrl Pts',(1.07201220072642,-0.512752161426865,
58.3442100685268));
#41034=CARTESIAN_POINT('Ctrl Pts',(1.15709058808409,-0.334878568438493,
58.3521351902925));
#41035=CARTESIAN_POINT('Ctrl Pts',(1.19694453918204,-0.135373759475367,
58.3600603120583));
#41036=CARTESIAN_POINT('Ctrl Pts',(1.18673432961957,0.0615350993874707,
58.367985433824));
#41037=CARTESIAN_POINT('Ctrl Pts',(1.17652412005709,0.258443958250309,58.3759105555897));
#41038=CARTESIAN_POINT('Ctrl Pts',(1.11624974983419,0.452756867012861,58.3838356773554));
#41039=CARTESIAN_POINT('Ctrl Pts',(1.01323072761359,0.620877145797678,58.3917607991211));
#41040=CARTESIAN_POINT('Ctrl Pts',(0.910211705392977,0.788997424582495,
58.3996859208868));
#41041=CARTESIAN_POINT('Ctrl Pts',(0.764448031174658,0.930925073389578,
58.4076110426526));
#41042=CARTESIAN_POINT('Ctrl Pts',(0.593640735632269,1.0294248950517,58.4155361644183));
#41043=CARTESIAN_POINT('Ctrl Pts',(0.422833440089881,1.12792471671382,58.423461286184));
#41044=CARTESIAN_POINT('Ctrl Pts',(0.226982523223422,1.18299671123099,58.4313864079497));
#41045=CARTESIAN_POINT('Ctrl Pts',(0.0298714352340844,1.18795312824677,
58.4393115297154));
#41046=CARTESIAN_POINT('Ctrl Pts',(-0.167239652755254,1.19290954526255,
58.4472366514811));
#41047=CARTESIAN_POINT('Ctrl Pts',(-0.365610911867472,1.14775038477695,
58.4551617732469));
#41048=CARTESIAN_POINT('Ctrl Pts',(-0.54115283035594,1.05795961725955,58.4630868950126));
#41049=CARTESIAN_POINT('Ctrl Pts',(-0.716694748844407,0.968168849742159,
58.4710120167783));
#41050=CARTESIAN_POINT('Ctrl Pts',(-0.869407326709119,0.833746475192972,
58.478937138544));
#41051=CARTESIAN_POINT('Ctrl Pts',(-0.9807456827269,0.671016276528948,58.4868622603097));
#41052=CARTESIAN_POINT('Ctrl Pts',(-1.09208403874468,0.508286077864927,
58.4947873820755));
#41053=CARTESIAN_POINT('Ctrl Pts',(-1.16204817291552,0.317248055086073,
58.5027125038412));
#41054=CARTESIAN_POINT('Ctrl Pts',(-1.18214188554047,0.121101197372472,
58.5106376256069));
#41055=CARTESIAN_POINT('Ctrl Pts',(-1.18626135085938,0.0808886098409063,
58.5122623758395));
#41056=CARTESIAN_POINT('Ctrl Pts',(-1.18828475300578,0.0404612970186917,
58.5138871260722));
#41057=CARTESIAN_POINT('Ctrl Pts',(-1.18824324986219,2.98497152091627E-5,
58.5155118763048));
#41058=CARTESIAN_POINT('Origin',(0.,0.,57.95));
#41059=CARTESIAN_POINT('',(-1.18823546047583,-3.02886631483035E-5,58.8580381236952));
#41060=CARTESIAN_POINT('',(-1.1882605894663,-2.81773776290431E-5,58.8155118763048));
#41061=CARTESIAN_POINT('',(-1.188225,-1.45515594291686E-16,57.95));
#41062=CARTESIAN_POINT('Ctrl Pts',(-1.18823546047583,-3.02886631483035E-5,
58.8580381236952));
#41063=CARTESIAN_POINT('Ctrl Pts',(-1.18807696349612,0.154289641889854,
58.8518368465376));
#41064=CARTESIAN_POINT('Ctrl Pts',(-1.15786515478889,0.308669815085824,
58.84563556938));
#41065=CARTESIAN_POINT('Ctrl Pts',(-1.09925951056845,0.451390584931154,
58.8394342922223));
#41066=CARTESIAN_POINT('Ctrl Pts',(-1.02436254099252,0.633785187006535,
58.8315091704566));
#41067=CARTESIAN_POINT('Ctrl Pts',(-0.90309166668407,0.797137202885021,
58.8235840486909));
#41068=CARTESIAN_POINT('Ctrl Pts',(-0.750173598378564,0.921609735210858,
58.8156589269252));
#41069=CARTESIAN_POINT('Ctrl Pts',(-0.597255530073064,1.04608226753669,
58.8077338051595));
#41070=CARTESIAN_POINT('Ctrl Pts',(-0.412690267770512,1.13167531630988,
58.7998086833938));
#41071=CARTESIAN_POINT('Ctrl Pts',(-0.218890771262336,1.16799476111661,
58.791883561628));
#41072=CARTESIAN_POINT('Ctrl Pts',(-0.0250912747541551,1.20431420592335,
58.7839584398623));
#41073=CARTESIAN_POINT('Ctrl Pts',(0.17794245595965,1.19136004676362,58.7760333180966));
#41074=CARTESIAN_POINT('Ctrl Pts',(0.365554714891826,1.1307053914084,58.7681081963309));
#41075=CARTESIAN_POINT('Ctrl Pts',(0.553166973824001,1.07005073605319,58.7601830745652));
#41076=CARTESIAN_POINT('Ctrl Pts',(0.725357760974547,0.961695584502476,
58.7522579527995));
#41077=CARTESIAN_POINT('Ctrl Pts',(0.861216829525005,0.818798207302978,
58.7443328310337));
#41078=CARTESIAN_POINT('Ctrl Pts',(0.997075898075464,0.67590083010348,58.736407709268));
#41079=CARTESIAN_POINT('Ctrl Pts',(1.09660324802584,0.498461227255193,58.7284825875023));
#41080=CARTESIAN_POINT('Ctrl Pts',(1.14771262617356,0.308027043393035,58.7205574657366));
#41081=CARTESIAN_POINT('Ctrl Pts',(1.19882200432129,0.117592859530876,58.7126323439708));
#41082=CARTESIAN_POINT('Ctrl Pts',(1.20151341066637,-0.085835905345154,
58.7047072222051));
#41083=CARTESIAN_POINT('Ctrl Pts',(1.15546001023758,-0.277555573681085,
58.6967821004394));
#41084=CARTESIAN_POINT('Ctrl Pts',(1.10940660980879,-0.469275242017015,
58.6888569786737));
#41085=CARTESIAN_POINT('Ctrl Pts',(1.01460840260613,-0.649285813812847,
58.680931856908));
#41086=CARTESIAN_POINT('Ctrl Pts',(0.88257735128077,-0.795727434958663,
58.6730067351423));
#41087=CARTESIAN_POINT('Ctrl Pts',(0.750546299955413,-0.942169056104479,
58.6650816133765));
#41088=CARTESIAN_POINT('Ctrl Pts',(0.581282404507365,-1.05504172660028,
58.6571564916108));
#41089=CARTESIAN_POINT('Ctrl Pts',(0.395340480265844,-1.12063858420226,
58.6492313698451));
#41090=CARTESIAN_POINT('Ctrl Pts',(0.209398556024328,-1.18623544180424,
58.6413062480794));
#41091=CARTESIAN_POINT('Ctrl Pts',(0.00677860298933977,-1.20455648651239,
58.6333811263137));
#41092=CARTESIAN_POINT('Ctrl Pts',(-0.187913920565669,-1.17337687474967,
58.625456004548));
#41093=CARTESIAN_POINT('Ctrl Pts',(-0.382606444120684,-1.14219726298696,
58.6175308827822));
#41094=CARTESIAN_POINT('Ctrl Pts',(-0.569371538195719,-1.06151699475336,
58.6096057610165));
#41095=CARTESIAN_POINT('Ctrl Pts',(-0.725529103124543,-0.941133599580297,
58.6016806392508));
#41096=CARTESIAN_POINT('Ctrl Pts',(-0.881686668053367,-0.820750204407234,
58.5937555174851));
#41097=CARTESIAN_POINT('Ctrl Pts',(-1.00723670383598,-0.660663682294702,
58.5858303957194));
#41098=CARTESIAN_POINT('Ctrl Pts',(-1.08693285333723,-0.480314380459157,
58.5779052739537));
#41099=CARTESIAN_POINT('Ctrl Pts',(-1.15352848109623,-0.329611052295889,
58.5712828905342));
#41100=CARTESIAN_POINT('Ctrl Pts',(-1.18810620429966,-0.164759048855221,
58.5646605071147));
#41101=CARTESIAN_POINT('Ctrl Pts',(-1.18826810796675,2.71338473248756E-5,
58.5580381236952));
#41102=CARTESIAN_POINT('Ctrl Pts',(-1.18824324986219,2.98497152091627E-5,
58.5155118763048));
#41103=CARTESIAN_POINT('Ctrl Pts',(-1.18808231114118,-0.156753103451461,
58.5218122478379));
#41104=CARTESIAN_POINT('Ctrl Pts',(-1.15687154130276,-0.313598226513166,
58.528112619371));
#41105=CARTESIAN_POINT('Ctrl Pts',(-1.09642773814146,-0.458226093307908,
58.534412990904));
#41106=CARTESIAN_POINT('Ctrl Pts',(-1.02039658703845,-0.640150833626332,
58.5423381126698));
#41107=CARTESIAN_POINT('Ctrl Pts',(-0.898110993753373,-0.802744621614826,
58.5502632344355));
#41108=CARTESIAN_POINT('Ctrl Pts',(-0.744420892944448,-0.926262636460101,
58.5581883562012));
#41109=CARTESIAN_POINT('Ctrl Pts',(-0.590730792135523,-1.04978065130538,
58.5661134779669));
#41110=CARTESIAN_POINT('Ctrl Pts',(-0.405636183802751,-1.13422289300743,
58.5740385997326));
#41111=CARTESIAN_POINT('Ctrl Pts',(-0.211614309667662,-1.16933499113732,
58.5819637214984));
#41112=CARTESIAN_POINT('Ctrl Pts',(-0.0175924355325727,-1.2044470892672,
58.5898888432641));
#41113=CARTESIAN_POINT('Ctrl Pts',(0.185356704404831,-1.19022904382492,
58.5978139650298));
#41114=CARTESIAN_POINT('Ctrl Pts',(0.372587676565259,-1.12840744451015,
58.6057390867955));
#41115=CARTESIAN_POINT('Ctrl Pts',(0.559818648725685,-1.06658584519538,
58.6136642085613));
#41116=CARTESIAN_POINT('Ctrl Pts',(0.731331453109135,-0.95716069200813,
58.6215893303269));
#41117=CARTESIAN_POINT('Ctrl Pts',(0.866298174752611,-0.813420192750661,
58.6295144520927));
#41118=CARTESIAN_POINT('Ctrl Pts',(1.00126489639609,-0.669679693493192,
58.6374395738584));
#41119=CARTESIAN_POINT('Ctrl Pts',(1.09968553529959,-0.491623848165508,
58.6453646956241));
#41120=CARTESIAN_POINT('Ctrl Pts',(1.14960823337849,-0.300875135733428,
58.6532898173898));
#41121=CARTESIAN_POINT('Ctrl Pts',(1.1995309314574,-0.110126423301345,58.6612149391555));
#41122=CARTESIAN_POINT('Ctrl Pts',(1.20095568871171,0.0933151562351321,
58.6691400609212));
#41123=CARTESIAN_POINT('Ctrl Pts',(1.15370948760467,0.284744369154499,58.677065182687));
#41124=CARTESIAN_POINT('Ctrl Pts',(1.10646328649763,0.476173582073863,58.6849903044527));
#41125=CARTESIAN_POINT('Ctrl Pts',(1.01054612702925,0.655590428376123,58.6929154262184));
#41126=CARTESIAN_POINT('Ctrl Pts',(0.877605853499431,0.801207153898268,
58.7008405479841));
#41127=CARTESIAN_POINT('Ctrl Pts',(0.744665579969613,0.946823879420414,
58.7087656697499));
#41128=CARTESIAN_POINT('Ctrl Pts',(0.574702192378362,1.05864048416245,58.7166907915156));
#41129=CARTESIAN_POINT('Ctrl Pts',(0.38835544993374,1.12307835081128,58.7246159132813));
#41130=CARTESIAN_POINT('Ctrl Pts',(0.202008707489123,1.18751621746011,58.732541035047));
#41131=CARTESIAN_POINT('Ctrl Pts',(-0.000721389808862383,1.20457534601574,
58.7404661568127));
#41132=CARTESIAN_POINT('Ctrl Pts',(-0.195216008152784,1.17218413558413,
58.7483912785784));
#41133=CARTESIAN_POINT('Ctrl Pts',(-0.389710626496712,1.13979292515252,
58.7563164003441));
#41134=CARTESIAN_POINT('Ctrl Pts',(-0.575969765886575,1.05795137573367,
58.7642415221098));
#41135=CARTESIAN_POINT('Ctrl Pts',(-0.731374768023134,0.936598038783625,
58.7721666438756));
#41136=CARTESIAN_POINT('Ctrl Pts',(-0.886779770159693,0.815244701833581,
58.7800917656413));
#41137=CARTESIAN_POINT('Ctrl Pts',(-1.01133063504295,0.654379577352344,
58.788016887407));
#41138=CARTESIAN_POINT('Ctrl Pts',(-1.08990234135637,0.473537563304248,
58.7959420091728));
#41139=CARTESIAN_POINT('Ctrl Pts',(-1.15457591560756,0.324683733191172,
58.8024652982168));
#41140=CARTESIAN_POINT('Ctrl Pts',(-1.18809774503898,0.16229518462225,58.8089885872608));
#41141=CARTESIAN_POINT('Ctrl Pts',(-1.1882605894663,-2.81773776290431E-5,
58.8155118763048));
#41142=CARTESIAN_POINT('Origin',(0.,0.,57.95));
#41143=CARTESIAN_POINT('',(-1.18814215656827,1.71474778534464E-5,59.1580381236952));
#41144=CARTESIAN_POINT('',(-1.18813194074363,1.05284942013778E-5,59.1155118763048));
#41145=CARTESIAN_POINT('',(-1.188225,-1.45515594291686E-16,57.95));
#41146=CARTESIAN_POINT('Ctrl Pts',(-1.18814215656827,1.71474778534464E-5,
59.1580381236952));
#41147=CARTESIAN_POINT('Ctrl Pts',(-1.18818264834069,0.0790378129302419,
59.1548634294919));
#41148=CARTESIAN_POINT('Ctrl Pts',(-1.18041668547805,0.15805062590395,59.1516887352886));
#41149=CARTESIAN_POINT('Ctrl Pts',(-1.16476568243126,0.235469396674217,
59.1485140410854));
#41150=CARTESIAN_POINT('Ctrl Pts',(-1.12569542968893,0.428733108396165,
59.1405889193196));
#41151=CARTESIAN_POINT('Ctrl Pts',(-1.03748779648867,0.61206319183124,59.1326637975539));
#41152=CARTESIAN_POINT('Ctrl Pts',(-0.910854409230566,0.763196682988669,
59.1247386757882));
#41153=CARTESIAN_POINT('Ctrl Pts',(-0.78422102197246,0.914330174146098,
59.1168135540225));
#41154=CARTESIAN_POINT('Ctrl Pts',(-0.619161880656503,1.03326707302588,
59.1088884322568));
#41155=CARTESIAN_POINT('Ctrl Pts',(-0.43572118997955,1.10556409870368,59.100963310491));
#41156=CARTESIAN_POINT('Ctrl Pts',(-0.252280499302597,1.17786112438148,
59.0930381887253));
#41157=CARTESIAN_POINT('Ctrl Pts',(-0.0504582592646509,1.20351827685729,
59.0851130669596));
#41158=CARTESIAN_POINT('Ctrl Pts',(0.145236943336567,1.17941984129059,59.0771879451939));
#41159=CARTESIAN_POINT('Ctrl Pts',(0.340932145937779,1.15532140572389,59.0692628234282));
#41160=CARTESIAN_POINT('Ctrl Pts',(0.53050031110226,1.08146738211468,59.0613377016625));
#41161=CARTESIAN_POINT('Ctrl Pts',(0.690920944016633,0.966826344727343,
59.0534125798967));
#41162=CARTESIAN_POINT('Ctrl Pts',(0.851341576931016,0.852185307340005,
59.045487458131));
#41163=CARTESIAN_POINT('Ctrl Pts',(0.982614677595285,0.696757256174546,
59.0375623363653));
#41164=CARTESIAN_POINT('Ctrl Pts',(1.06879889989599,0.519416830032286,59.0296372145996));
#41165=CARTESIAN_POINT('Ctrl Pts',(1.1549831221967,0.342076403890031,59.0217120928339));
#41166=CARTESIAN_POINT('Ctrl Pts',(1.19607846613384,0.142823602770977,59.0137869710682));
#41167=CARTESIAN_POINT('Ctrl Pts',(1.18709445690308,-0.0541450102008245,
59.0058618493024));
#41168=CARTESIAN_POINT('Ctrl Pts',(1.17811044767232,-0.251113623172624,
58.9979367275367));
#41169=CARTESIAN_POINT('Ctrl Pts',(1.11904708527366,-0.445798047997178,
58.990011605771));
#41170=CARTESIAN_POINT('Ctrl Pts',(1.01707681781609,-0.614556489186126,
58.9820864840053));
#41171=CARTESIAN_POINT('Ctrl Pts',(0.915106550358513,-0.783314930375073,
58.9741613622396));
#41172=CARTESIAN_POINT('Ctrl Pts',(0.770229377842034,-0.926147387928421,
58.9662362404738));
#41173=CARTESIAN_POINT('Ctrl Pts',(0.600038677274853,-1.02570878787008,
58.9583111187081));
#41174=CARTESIAN_POINT('Ctrl Pts',(0.429847976707667,-1.12527018781175,
58.9503859969424));
#41175=CARTESIAN_POINT('Ctrl Pts',(0.234343748089779,-1.18156053014173,
58.9424608751767));
#41176=CARTESIAN_POINT('Ctrl Pts',(0.0372673410142875,-1.18774411260734,
58.934535753411));
#41177=CARTESIAN_POINT('Ctrl Pts',(-0.159809066061204,-1.19392769507295,
58.9266106316453));
#41178=CARTESIAN_POINT('Ctrl Pts',(-0.358457651594298,-1.1500045176742,
58.9186855098796));
#41179=CARTESIAN_POINT('Ctrl Pts',(-0.534555226287983,-1.06130845741842,
58.9107603881138));
#41180=CARTESIAN_POINT('Ctrl Pts',(-0.710652800981668,-0.97261239716265,
58.9028352663481));
#41181=CARTESIAN_POINT('Ctrl Pts',(-0.864199364835943,-0.839143454049854,
58.8949101445824));
#41182=CARTESIAN_POINT('Ctrl Pts',(-0.976548760286572,-0.677109629618743,
58.8869850228167));
#41183=CARTESIAN_POINT('Ctrl Pts',(-1.0888981557372,-0.515075805187633,
58.8790599010509));
#41184=CARTESIAN_POINT('Ctrl Pts',(-1.16005038278419,-0.324477099438208,
58.8711347792852));
#41185=CARTESIAN_POINT('Ctrl Pts',(-1.18136496388598,-0.128459152427356,
58.8632096575195));
#41186=CARTESIAN_POINT('Ctrl Pts',(-1.18600123658848,-0.085822018130073,
58.8614858129114));
#41187=CARTESIAN_POINT('Ctrl Pts',(-1.18827951981344,-0.0429284809945659,
58.8597619683033));
#41188=CARTESIAN_POINT('Ctrl Pts',(-1.18823546047583,-3.02886631483035E-5,
58.8580381236952));
#41189=CARTESIAN_POINT('Ctrl Pts',(-1.1882605894663,-2.81773776290431E-5,
58.8155118763048));
#41190=CARTESIAN_POINT('Ctrl Pts',(-1.1882955841822,-0.0349109180948725,
58.8169137090265));
#41191=CARTESIAN_POINT('Ctrl Pts',(-1.1867900424793,-0.069790648460224,
58.8183155417482));
#41192=CARTESIAN_POINT('Ctrl Pts',(-1.18372205960733,-0.10453240240814,
58.8197173744699));
#41193=CARTESIAN_POINT('Ctrl Pts',(-1.16637752380126,-0.300941450457477,
58.8276424962356));
#41194=CARTESIAN_POINT('Ctrl Pts',(-1.09909590444552,-0.492940642941198,
58.8355676180013));
#41195=CARTESIAN_POINT('Ctrl Pts',(-0.990047646024145,-0.657214269592707,
58.843492739767));
#41196=CARTESIAN_POINT('Ctrl Pts',(-0.880999387602772,-0.821487896244211,
58.8514178615328));
#41197=CARTESIAN_POINT('Ctrl Pts',(-0.730184490115758,-0.958035957063507,
58.8593429832985));
#41198=CARTESIAN_POINT('Ctrl Pts',(-0.555917387119857,-1.05027653322925,
58.8672681050642));
#41199=CARTESIAN_POINT('Ctrl Pts',(-0.381650284123952,-1.142517109395,58.8751932268299));
#41200=CARTESIAN_POINT('Ctrl Pts',(-0.183930975619157,-1.1904502009072,
58.8831183485956));
#41201=CARTESIAN_POINT('Ctrl Pts',(0.0132301972489506,-1.1882549808164,
58.8910434703614));
#41202=CARTESIAN_POINT('Ctrl Pts',(0.210391370117058,-1.1860597607256,58.8989685921271));
#41203=CARTESIAN_POINT('Ctrl Pts',(0.406994407348479,-1.13373622903181,
58.9068937138928));
#41204=CARTESIAN_POINT('Ctrl Pts',(0.579164523876036,-1.03763837238109,
58.9148188356585));
#41205=CARTESIAN_POINT('Ctrl Pts',(0.751334640403598,-0.941540515730364,
58.9227439574242));
#41206=CARTESIAN_POINT('Ctrl Pts',(0.899071836227295,-0.801668334122712,
58.93066907919));
#41207=CARTESIAN_POINT('Ctrl Pts',(1.00443542311368,-0.635007415979277,
58.9385942009557));
#41208=CARTESIAN_POINT('Ctrl Pts',(1.10979901000005,-0.468346497835848,
58.9465193227214));
#41209=CARTESIAN_POINT('Ctrl Pts',(1.17278898794912,-0.274896843156645,
58.9544444444871));
#41210=CARTESIAN_POINT('Ctrl Pts',(1.18575607439587,-0.0781503012631315,
58.9623695662528));
#41211=CARTESIAN_POINT('Ctrl Pts',(1.19872316084263,0.11859624063038,58.9702946880185));
#41212=CARTESIAN_POINT('Ctrl Pts',(1.16166735578707,0.318639669738194,58.9782198097842));
#41213=CARTESIAN_POINT('Ctrl Pts',(1.07908858656325,0.497687411839151,58.98614493155));
#41214=CARTESIAN_POINT('Ctrl Pts',(0.996509817339424,0.676735153940114,
58.9940700533157));
#41215=CARTESIAN_POINT('Ctrl Pts',(0.868408083947323,0.834787209034219,
59.0019951750814));
#41216=CARTESIAN_POINT('Ctrl Pts',(0.710339612753224,0.952650288462575,
59.0099202968471));
#41217=CARTESIAN_POINT('Ctrl Pts',(0.552271141559124,1.07051336789093,59.0178454186129));
#41218=CARTESIAN_POINT('Ctrl Pts',(0.364235932563025,1.14818747165354,59.0257705403786));
#41219=CARTESIAN_POINT('Ctrl Pts',(0.169068323743945,1.17624012831591,59.0336956621443));
#41220=CARTESIAN_POINT('Ctrl Pts',(-0.0260992850751359,1.20429278497829,
59.04162078391));
#41221=CARTESIAN_POINT('Ctrl Pts',(-0.228399293717199,1.18272399454044,
59.0495459056757));
#41222=CARTESIAN_POINT('Ctrl Pts',(-0.41326509683661,1.11415299545927,59.0574710274414));
#41223=CARTESIAN_POINT('Ctrl Pts',(-0.598130899956021,1.04558199637809,
59.0653961492071));
#41224=CARTESIAN_POINT('Ctrl Pts',(-0.765562497552781,0.930008788653607,
59.0733212709729));
#41225=CARTESIAN_POINT('Ctrl Pts',(-0.895227582138825,0.781468178323405,
59.0812463927386));
#41226=CARTESIAN_POINT('Ctrl Pts',(-1.02489266672487,0.632927567993202,
59.0891715145043));
#41227=CARTESIAN_POINT('Ctrl Pts',(-1.1167912383002,0.451419555057285,59.09709663627));
#41228=CARTESIAN_POINT('Ctrl Pts',(-1.15976345582045,0.258985837639138,
59.1050217580358));
#41229=CARTESIAN_POINT('Ctrl Pts',(-1.17872357014204,0.174080624640588,
59.1085184641254));
#41230=CARTESIAN_POINT('Ctrl Pts',(-1.18815903006735,0.0870484687860079,
59.1120151702151));
#41231=CARTESIAN_POINT('Ctrl Pts',(-1.18813194074363,1.05284942013778E-5,
59.1155118763048));
#41232=CARTESIAN_POINT('Origin',(0.,0.,57.95));
#41233=CARTESIAN_POINT('',(-1.18832756091501,3.87725375256866E-6,59.4580381236952));
#41234=CARTESIAN_POINT('',(-1.18831870923562,1.19544632238963E-5,59.4155118763048));
#41235=CARTESIAN_POINT('',(-1.188225,-1.45515594291686E-16,57.95));
#41236=CARTESIAN_POINT('Ctrl Pts',(-1.18832756091501,3.87725375256866E-6,
59.4580381236952));
#41237=CARTESIAN_POINT('Ctrl Pts',(-1.18832824821205,0.00368882683057432,
59.4578900124462));
#41238=CARTESIAN_POINT('Ctrl Pts',(-1.18831146503093,0.00737377012193548,
59.4577419011973));
#41239=CARTESIAN_POINT('Ctrl Pts',(-1.18827717308989,0.0110585504702445,
59.4575937899484));
#41240=CARTESIAN_POINT('Ctrl Pts',(-1.18644228336852,0.208223405601848,
59.4496686681827));
#41241=CARTESIAN_POINT('Ctrl Pts',(-1.13447814598937,0.404921739252035,
59.4417435464169));
#41242=CARTESIAN_POINT('Ctrl Pts',(-1.03869510378624,0.577267193901848,
59.4338184246512));
#41243=CARTESIAN_POINT('Ctrl Pts',(-0.942912061583119,0.749612648551651,
59.4258933028855));
#41244=CARTESIAN_POINT('Ctrl Pts',(-0.803310114556024,0.897605224201085,
59.4179681811198));
#41245=CARTESIAN_POINT('Ctrl Pts',(-0.636842034887918,1.00327322017851,
59.4100430593541));
#41246=CARTESIAN_POINT('Ctrl Pts',(-0.470373955219807,1.10894121615594,
59.4021179375883));
#41247=CARTESIAN_POINT('Ctrl Pts',(-0.277039742910682,1.17228463246137,
59.3941928158226));
#41248=CARTESIAN_POINT('Ctrl Pts',(-0.0803172283162318,1.18561126621479,
59.3862676940569));
#41249=CARTESIAN_POINT('Ctrl Pts',(0.116405286278219,1.19893789996821,59.3783425722912));
#41250=CARTESIAN_POINT('Ctrl Pts',(0.316516103157997,1.16224775116963,59.3704174505255));
#41251=CARTESIAN_POINT('Ctrl Pts',(0.49571446474428,1.07999634313522,59.3624923287597));
#41252=CARTESIAN_POINT('Ctrl Pts',(0.674912826330568,0.997744935100801,
59.354567206994));
#41253=CARTESIAN_POINT('Ctrl Pts',(0.833198732623362,0.869932267830549,
59.3466420852283));
#41254=CARTESIAN_POINT('Ctrl Pts',(0.951350496902659,0.712079464512692,
59.3387169634626));
#41255=CARTESIAN_POINT('Ctrl Pts',(1.06950226118195,0.554226661194839,59.3307918416969));
#41256=CARTESIAN_POINT('Ctrl Pts',(1.14751988344775,0.366333721829396,59.3228667199312));
#41257=CARTESIAN_POINT('Ctrl Pts',(1.17592917657546,0.171217707668849,59.3149415981654));
#41258=CARTESIAN_POINT('Ctrl Pts',(1.20433846970317,-0.0238983064916926,
59.3070164763997));
#41259=CARTESIAN_POINT('Ctrl Pts',(1.18313943369279,-0.226237395447325,
59.299091354634));
#41260=CARTESIAN_POINT('Ctrl Pts',(1.1149064053193,-0.411228208075728,59.2911662328683));
#41261=CARTESIAN_POINT('Ctrl Pts',(1.04667337694581,-0.596219020704137,
59.2832411111026));
#41262=CARTESIAN_POINT('Ctrl Pts',(0.931406356209218,-0.76386155700532,
59.2753159893369));
#41263=CARTESIAN_POINT('Ctrl Pts',(0.783102966869399,-0.893797893832923,
59.2673908675711));
#41264=CARTESIAN_POINT('Ctrl Pts',(0.634799577529581,-1.02373423066053,
59.2594657458054));
#41265=CARTESIAN_POINT('Ctrl Pts',(0.453459819586538,-1.11596436801455,
59.2515406240397));
#41266=CARTESIAN_POINT('Ctrl Pts',(0.26110495886651,-1.15928820066236,59.243615502274));
#41267=CARTESIAN_POINT('Ctrl Pts',(0.0687500981464874,-1.20261203331017,
59.2356903805083));
#41268=CARTESIAN_POINT('Ctrl Pts',(-0.134619865350523,-1.19702956125176,
59.2277652587426));
#41269=CARTESIAN_POINT('Ctrl Pts',(-0.324308394704534,-1.14321870036482,
59.2198401369768));
#41270=CARTESIAN_POINT('Ctrl Pts',(-0.513996924058551,-1.08940783947788,
59.2119150152111));
#41271=CARTESIAN_POINT('Ctrl Pts',(-0.690004019269572,-0.987368589762404,
59.2039898934454));
#41272=CARTESIAN_POINT('Ctrl Pts',(-0.830955994418717,-0.849492240741074,
59.1960647716797));
#41273=CARTESIAN_POINT('Ctrl Pts',(-0.971907969567863,-0.711615891719744,
59.1881396499139));
#41274=CARTESIAN_POINT('Ctrl Pts',(-1.07780482465514,-0.537902443392555,
59.1802145281482));
#41275=CARTESIAN_POINT('Ctrl Pts',(-1.13578681605657,-0.349447049224552,
59.1722894063825));
#41276=CARTESIAN_POINT('Ctrl Pts',(-1.17054202338604,-0.236484280296531,
59.1675389788201));
#41277=CARTESIAN_POINT('Ctrl Pts',(-1.18808156703762,-0.118224775407469,
59.1627885512576));
#41278=CARTESIAN_POINT('Ctrl Pts',(-1.18814215656827,1.71474778534464E-5,
59.1580381236952));
#41279=CARTESIAN_POINT('Ctrl Pts',(-1.18813194074363,1.05284942013778E-5,
59.1155118763048));
#41280=CARTESIAN_POINT('Ctrl Pts',(-1.18809763337471,-0.110218975876756,
59.1199402919808));
#41281=CARTESIAN_POINT('Ctrl Pts',(-1.17288630091938,-0.220457757932465,
59.1243687076569));
#41282=CARTESIAN_POINT('Ctrl Pts',(-1.14262409572745,-0.326397171276419,
59.1287971233329));
#41283=CARTESIAN_POINT('Ctrl Pts',(-1.08846665464904,-0.51598704087343,
59.1367222450986));
#41284=CARTESIAN_POINT('Ctrl Pts',(-0.986105909027061,-0.691807358167079,
59.1446473668643));
#41285=CARTESIAN_POINT('Ctrl Pts',(-0.847972189722383,-0.83250711889548,
59.1525724886301));
#41286=CARTESIAN_POINT('Ctrl Pts',(-0.709838470417701,-0.973206879623886,
59.1604976103958));
#41287=CARTESIAN_POINT('Ctrl Pts',(-0.535931777430326,-1.07878608378704,
59.1684227321615));
#41288=CARTESIAN_POINT('Ctrl Pts',(-0.347370731180798,-1.13642356217792,
59.1763478539272));
#41289=CARTESIAN_POINT('Ctrl Pts',(-0.158809684931281,-1.19406104056879,
59.1842729756929));
#41290=CARTESIAN_POINT('Ctrl Pts',(0.0444057145803972,-1.2037567931874,
59.1921980974586));
#41291=CARTESIAN_POINT('Ctrl Pts',(0.237597700143673,-1.16433340175427,
59.2001232192244));
#41292=CARTESIAN_POINT('Ctrl Pts',(0.430789685706959,-1.12491001032114,
59.2080483409901));
#41293=CARTESIAN_POINT('Ctrl Pts',(0.613958257321854,-1.03636747483627,
59.2159734627558));
#41294=CARTESIAN_POINT('Ctrl Pts',(0.764860064428019,-0.909458091061591,
59.2238985845215));
#41295=CARTESIAN_POINT('Ctrl Pts',(0.915761871534184,-0.782548707286909,
59.2318237062872));
#41296=CARTESIAN_POINT('Ctrl Pts',(1.03439691413161,-0.617272475222414,
59.239748828053));
#41297=CARTESIAN_POINT('Ctrl Pts',(1.10635856766692,-0.433699962306019,
59.2476739498187));
#41298=CARTESIAN_POINT('Ctrl Pts',(1.17832022120222,-0.250127449389618,
59.2555990715844));
#41299=CARTESIAN_POINT('Ctrl Pts',(1.20360848567539,-0.0482586556213197,
59.2635241933501));
#41300=CARTESIAN_POINT('Ctrl Pts',(1.17915244271448,0.147392178878999,59.2714493151158));
#41301=CARTESIAN_POINT('Ctrl Pts',(1.15469639975357,0.343043013379306,59.2793744368816));
#41302=CARTESIAN_POINT('Ctrl Pts',(1.08049604935858,0.532475888611629,59.2872995586473));
#41303=CARTESIAN_POINT('Ctrl Pts',(0.965562022507184,0.692686738898676,
59.295224680413));
#41304=CARTESIAN_POINT('Ctrl Pts',(0.850627995655786,0.852897589185722,
59.3031498021787));
#41305=CARTESIAN_POINT('Ctrl Pts',(0.694960292347977,0.983886414527489,
59.3110749239444));
#41306=CARTESIAN_POINT('Ctrl Pts',(0.51746265390297,1.06974639021121,59.3190000457101));
#41307=CARTESIAN_POINT('Ctrl Pts',(0.339965015457963,1.15560636589492,59.3269251674758));
#41308=CARTESIAN_POINT('Ctrl Pts',(0.140637441875762,1.19633749192059,59.3348502892416));
#41309=CARTESIAN_POINT('Ctrl Pts',(-0.0563144236134591,1.18699352283291,
59.3427754110073));
#41310=CARTESIAN_POINT('Ctrl Pts',(-0.253266289102692,1.17764955374524,
59.350700532773));
#41311=CARTESIAN_POINT('Ctrl Pts',(-0.447842446498957,1.11823048954422,
59.3586256545387));
#41312=CARTESIAN_POINT('Ctrl Pts',(-0.616414247931142,1.01595197352132,
59.3665507763045));
#41313=CARTESIAN_POINT('Ctrl Pts',(-0.784986049363317,0.913673457498427,
59.3744758980702));
#41314=CARTESIAN_POINT('Ctrl Pts',(-0.927553494831426,0.768535489653664,
59.3824010198359));
#41315=CARTESIAN_POINT('Ctrl Pts',(-1.02680369250096,0.598163117067689,
59.3903261416016));
#41316=CARTESIAN_POINT('Ctrl Pts',(-1.12605389017049,0.427790744481714,
59.3982512633673));
#41317=CARTESIAN_POINT('Ctrl Pts',(-1.18198684004144,0.23218396715453,59.406176385133));
#41318=CARTESIAN_POINT('Ctrl Pts',(-1.18781024034888,0.0350965878354738,
59.4141015068987));
#41319=CARTESIAN_POINT('Ctrl Pts',(-1.18815568806463,0.0234052423339456,
59.4145716300341));
#41320=CARTESIAN_POINT('Ctrl Pts',(-1.18832480348564,0.0117086866888603,
59.4150417531695));
#41321=CARTESIAN_POINT('Ctrl Pts',(-1.18831870923562,1.19544632238963E-5,
59.4155118763048));
#41322=CARTESIAN_POINT('Origin',(0.,0.,57.95));
#41323=CARTESIAN_POINT('',(-1.18815715028295,-2.22996587661006E-5,59.7580381236952));
#41324=CARTESIAN_POINT('',(-1.1881744462934,-2.6792430042513E-5,59.7155118763048));
#41325=CARTESIAN_POINT('',(-1.188225,-1.45515594291686E-16,57.95));
#41326=CARTESIAN_POINT('Ctrl Pts',(-1.18815715028295,-2.22996587661006E-5,
59.7580381236952));
#41327=CARTESIAN_POINT('Ctrl Pts',(-1.18807148486871,0.125588696935144,
59.7529914736348));
#41328=CARTESIAN_POINT('Ctrl Pts',(-1.16823594397195,0.25122604577743,59.7479448235745));
#41329=CARTESIAN_POINT('Ctrl Pts',(-1.12908604691359,0.370524885226803,
59.7428981735142));
#41330=CARTESIAN_POINT('Ctrl Pts',(-1.06760611515802,0.557868532566024,
59.7349730517485));
#41331=CARTESIAN_POINT('Ctrl Pts',(-0.958495617630607,0.729580968281685,
59.7270479299828));
#41332=CARTESIAN_POINT('Ctrl Pts',(-0.815002291341349,0.864810140128416,
59.7191228082171));
#41333=CARTESIAN_POINT('Ctrl Pts',(-0.671508965052082,1.00003931197515,
59.7111976864513));
#41334=CARTESIAN_POINT('Ctrl Pts',(-0.493632810000966,1.09878521995296,
59.7032725646856));
#41335=CARTESIAN_POINT('Ctrl Pts',(-0.302975525170295,1.14905644757922,
59.6953474429199));
#41336=CARTESIAN_POINT('Ctrl Pts',(-0.11231824033963,1.19932767520548,59.6874223211542));
#41337=CARTESIAN_POINT('Ctrl Pts',(0.0911201742705878,1.2011242224802,59.6794971993885));
#41338=CARTESIAN_POINT('Ctrl Pts',(0.282635353985177,1.15422794809806,59.6715720776228));
#41339=CARTESIAN_POINT('Ctrl Pts',(0.474150533699762,1.10733167371592,59.663646955857));
#41340=CARTESIAN_POINT('Ctrl Pts',(0.653742478518715,1.01174257767693,59.6557218340913));
#41341=CARTESIAN_POINT('Ctrl Pts',(0.799601946393605,0.879068653271273,
59.6477967123256));
#41342=CARTESIAN_POINT('Ctrl Pts',(0.9454614142685,0.746394728865611,59.6398715905599));
#41343=CARTESIAN_POINT('Ctrl Pts',(1.05758840519933,0.576635976093282,59.6319464687942));
#41344=CARTESIAN_POINT('Ctrl Pts',(1.12236671392606,0.390407309550219,59.6240213470285));
#41345=CARTESIAN_POINT('Ctrl Pts',(1.18714502265279,0.204178643007155,59.6160962252628));
#41346=CARTESIAN_POINT('Ctrl Pts',(1.20457464917542,0.0014800626933443,
59.608171103497));
#41347=CARTESIAN_POINT('Ctrl Pts',(1.17253895226116,-0.193073427482673,
59.6002459817313));
#41348=CARTESIAN_POINT('Ctrl Pts',(1.1405032553469,-0.387626917658684,59.5923208599656));
#41349=CARTESIAN_POINT('Ctrl Pts',(1.05900223499575,-0.574035317696915,
59.5843957381999));
#41350=CARTESIAN_POINT('Ctrl Pts',(0.937933112448952,-0.729661842412061,
59.5764706164341));
#41351=CARTESIAN_POINT('Ctrl Pts',(0.816863989902144,-0.885288367127217,
59.5685454946684));
#41352=CARTESIAN_POINT('Ctrl Pts',(0.656226765159698,-1.01013301651927,
59.5606203729027));
#41353=CARTESIAN_POINT('Ctrl Pts',(0.47552865042574,-1.08903509366436,59.552695251137));
#41354=CARTESIAN_POINT('Ctrl Pts',(0.294830535691792,-1.16793717080945,
59.5447701293713));
#41355=CARTESIAN_POINT('Ctrl Pts',(0.0940715309663313,-1.20089667570757,
59.5368450076055));
#41356=CARTESIAN_POINT('Ctrl Pts',(-0.102368887697813,-1.18391112112818,
59.5289198858398));
#41357=CARTESIAN_POINT('Ctrl Pts',(-0.298809306361958,-1.16692556654879,
59.5209947640741));
#41358=CARTESIAN_POINT('Ctrl Pts',(-0.4909311389648,-1.09999495249189,59.5130696423084));
#41359=CARTESIAN_POINT('Ctrl Pts',(-0.655403784494695,-0.991247098705512,
59.5051445205427));
#41360=CARTESIAN_POINT('Ctrl Pts',(-0.819876430024596,-0.882499244919128,
59.497219398777));
#41361=CARTESIAN_POINT('Ctrl Pts',(-0.956699888481545,-0.731934151403257,
59.4892942770112));
#41362=CARTESIAN_POINT('Ctrl Pts',(-1.04925879667821,-0.557835916338813,
59.4813691552455));
#41363=CARTESIAN_POINT('Ctrl Pts',(-1.14008788722682,-0.38699137349458,
59.4735921447287));
#41364=CARTESIAN_POINT('Ctrl Pts',(-1.18829147239159,-0.193485083363211,
59.465815134212));
#41365=CARTESIAN_POINT('Ctrl Pts',(-1.18832756091501,3.87725375256866E-6,
59.4580381236952));
#41366=CARTESIAN_POINT('Ctrl Pts',(-1.18831870923562,1.19544632238963E-5,
59.4155118763048));
#41367=CARTESIAN_POINT('Ctrl Pts',(-1.18822206939351,-0.185469499572606,
59.4229668749352));
#41368=CARTESIAN_POINT('Ctrl Pts',(-1.14406690366381,-0.370995356858145,
59.4304218735655));
#41369=CARTESIAN_POINT('Ctrl Pts',(-1.06032974762535,-0.536493955094488,
59.4378768721959));
#41370=CARTESIAN_POINT('Ctrl Pts',(-0.97131200385046,-0.712429137394463,
59.4458019939616));
#41371=CARTESIAN_POINT('Ctrl Pts',(-0.837562665556747,-0.865731520683477,
59.4537271157273));
#41372=CARTESIAN_POINT('Ctrl Pts',(-0.67532378448248,-0.977784599832173,
59.4616522374931));
#41373=CARTESIAN_POINT('Ctrl Pts',(-0.513084903408217,-1.08983767898087,
59.4695773592588));
#41374=CARTESIAN_POINT('Ctrl Pts',(-0.322356479553399,-1.16064145398924,
59.4775024810245));
#41375=CARTESIAN_POINT('Ctrl Pts',(-0.126299905510072,-1.18159776210965,
59.4854276027902));
#41376=CARTESIAN_POINT('Ctrl Pts',(0.0697566685332563,-1.20255407023006,
59.4933527245559));
#41377=CARTESIAN_POINT('Ctrl Pts',(0.271141392765097,-1.17366291146249,
59.5012778463217));
#41378=CARTESIAN_POINT('Ctrl Pts',(0.453398810824565,-1.09843272706388,
59.5092029680874));
#41379=CARTESIAN_POINT('Ctrl Pts',(0.635656228884028,-1.02320254266526,
59.5171280898531));
#41380=CARTESIAN_POINT('Ctrl Pts',(0.798786340771123,-0.901633332635603,
59.5250532116188));
#41381=CARTESIAN_POINT('Ctrl Pts',(0.922979196271283,-0.748488036544175,
59.5329783333845));
#41382=CARTESIAN_POINT('Ctrl Pts',(1.04717205177145,-0.595342740452742,
59.5409034551503));
#41383=CARTESIAN_POINT('Ctrl Pts',(1.13242765088467,-0.410621358299555,
59.548828576916));
#41384=CARTESIAN_POINT('Ctrl Pts',(1.16839285212588,-0.216755808551492,
59.5567536986817));
#41385=CARTESIAN_POINT('Ctrl Pts',(1.20435805336708,-0.0228902588034223,
59.5646788204474));
#41386=CARTESIAN_POINT('Ctrl Pts',(1.19103285673626,0.180119458539511,59.5726039422131));
#41387=CARTESIAN_POINT('Ctrl Pts',(1.13003542701731,0.367620553647926,59.5805290639788));
#41388=CARTESIAN_POINT('Ctrl Pts',(1.06903799729836,0.555121648756329,59.5884541857445));
#41389=CARTESIAN_POINT('Ctrl Pts',(0.960368334491289,0.72711412163022,59.5963793075103));
#41390=CARTESIAN_POINT('Ctrl Pts',(0.817222903323089,0.862711807917861,
59.604304429276));
#41391=CARTESIAN_POINT('Ctrl Pts',(0.674077472154888,0.998309494205502,
59.6122295510417));
#41392=CARTESIAN_POINT('Ctrl Pts',(0.496456272625558,1.0975123939069,59.6201546728074));
#41393=CARTESIAN_POINT('Ctrl Pts',(0.305928999608111,1.14827365419266,59.6280797945732));
#41394=CARTESIAN_POINT('Ctrl Pts',(0.115401726590658,1.19903491447843,59.6360049163389));
#41395=CARTESIAN_POINT('Ctrl Pts',(-0.0880316199149155,1.20135453534858,
59.6439300381046));
#41396=CARTESIAN_POINT('Ctrl Pts',(-0.279666801176563,1.15495082957736,
59.6518551598703));
#41397=CARTESIAN_POINT('Ctrl Pts',(-0.47130198243821,1.10854712380614,59.659780281636));
#41398=CARTESIAN_POINT('Ctrl Pts',(-0.651138998455935,1.01342009139355,
59.6677054034017));
#41399=CARTESIAN_POINT('Ctrl Pts',(-0.797339081473339,0.881121627627638,
59.6756305251674));
#41400=CARTESIAN_POINT('Ctrl Pts',(-0.943539164490747,0.748823163861718,
59.6835556469331));
#41401=CARTESIAN_POINT('Ctrl Pts',(-1.05610231450784,0.579353268742461,
59.6914807686989));
#41402=CARTESIAN_POINT('Ctrl Pts',(-1.12135923406337,0.393291770773819,
59.6994058904646));
#41403=CARTESIAN_POINT('Ctrl Pts',(-1.16556579026982,0.267249381340982,
59.7047745524113));
#41404=CARTESIAN_POINT('Ctrl Pts',(-1.18806340877614,0.133593067292119,
59.7101432143581));
#41405=CARTESIAN_POINT('Ctrl Pts',(-1.1881744462934,-2.6792430042513E-5,
59.7155118763048));
#41406=CARTESIAN_POINT('Origin',(0.,0.,55.5071980324285));
#41407=CARTESIAN_POINT('',(-1.01641695750709,-1.90763918373965E-5,59.8571980324285));
#41408=CARTESIAN_POINT('',(-1.016475,-7.2179708060976E-14,59.861775));
#41409=CARTESIAN_POINT('',(-1.016475,-7.2179708060976E-14,55.5071980324285));
#41410=CARTESIAN_POINT('',(-1.01180833082817,-0.0972899136175108,59.861775));
#41411=CARTESIAN_POINT('Ctrl Pts',(-1.01641695750709,-1.90763918375067E-5,
59.8571980324285));
#41412=CARTESIAN_POINT('Ctrl Pts',(-1.01643911175058,-0.0325037918279691,
59.8587236882857));
#41413=CARTESIAN_POINT('Ctrl Pts',(-1.01491718827352,-0.0649864470020175,
59.8602493441428));
#41414=CARTESIAN_POINT('Ctrl Pts',(-1.01184089351567,-0.0973166075163148,
59.861775));
#41415=CARTESIAN_POINT('Origin',(0.,0.,59.861775));
#41416=CARTESIAN_POINT('Origin',(0.,0.,55.5071980324285));
#41417=CARTESIAN_POINT('',(-1.01656273641868,3.31682248127331E-6,59.5571980324285));
#41418=CARTESIAN_POINT('',(-1.01643175349457,-2.29197629572075E-5,59.6163519675715));
#41419=CARTESIAN_POINT('',(-1.016475,-7.2179708060976E-14,55.5071980324285));
#41420=CARTESIAN_POINT('Ctrl Pts',(-1.01656273641868,3.31682248125081E-6,
59.5571980324285));
#41421=CARTESIAN_POINT('Ctrl Pts',(-1.01653186425065,-0.165518104830062,
59.5649750429453));
#41422=CARTESIAN_POINT('Ctrl Pts',(-0.933274376543597,-0.499743194453076,
59.5806771752278));
#41423=CARTESIAN_POINT('Ctrl Pts',(-0.584322219507429,-0.883741777366003,
59.604304429276));
#41424=CARTESIAN_POINT('Ctrl Pts',(-0.0912665108790651,-1.05551049774341,
59.6280797945731));
#41425=CARTESIAN_POINT('Ctrl Pts',(0.423955377218644,-0.970924212970794,
59.6518551598703));
#41426=CARTESIAN_POINT('Ctrl Pts',(0.836209932593474,-0.65052664940127,
59.6756305251674));
#41427=CARTESIAN_POINT('Ctrl Pts',(1.04537170665504,-0.172133722736198,
59.6994058904646));
#41428=CARTESIAN_POINT('Ctrl Pts',(1.00064083593713,0.348065833975191,59.7231812557618));
#41429=CARTESIAN_POINT('Ctrl Pts',(0.712881489585019,0.783729605291864,
59.7469566210589));
#41430=CARTESIAN_POINT('Ctrl Pts',(0.251982109139772,1.02904659423647,59.7707319863561));
#41431=CARTESIAN_POINT('Ctrl Pts',(-0.270116136119136,1.02443598919684,
59.7945073516532));
#41432=CARTESIAN_POINT('Ctrl Pts',(-0.726612165168123,0.7710174527789,59.8182827169504));
#41433=CARTESIAN_POINT('Ctrl Pts',(-0.97272844382277,0.383692432411846,
59.8391796105421));
#41434=CARTESIAN_POINT('Ctrl Pts',(-1.01634367445722,0.107435688288931,
59.8521513823682));
#41435=CARTESIAN_POINT('Ctrl Pts',(-1.01641695750709,-1.90763918375067E-5,
59.8571980324285));
#41436=CARTESIAN_POINT('',(-0.421648628688828,0.924896675066913,59.861775));
#41437=CARTESIAN_POINT('Origin',(0.,0.,59.861775));
#41438=CARTESIAN_POINT('Ctrl Pts',(-1.01643175349457,-2.29197629572769E-5,
59.6163519675715));
#41439=CARTESIAN_POINT('Ctrl Pts',(-1.01647698496138,-0.0544533717263767,
59.6189084273905));
#41440=CARTESIAN_POINT('Ctrl Pts',(-0.998858358818543,-0.277591283531375,
59.6293900089752));
#41441=CARTESIAN_POINT('Ctrl Pts',(-0.837879849628336,-0.648374486381346,
59.6477967123256));
#41442=CARTESIAN_POINT('Ctrl Pts',(-0.426450165346835,-0.969830983982369,
59.6715720776227));
#41443=CARTESIAN_POINT('Ctrl Pts',(0.0885519692748135,-1.0557416239719,
59.6953474429199));
#41444=CARTESIAN_POINT('Ctrl Pts',(0.582048910852398,-0.885241334592178,
59.7191228082171));
#41445=CARTESIAN_POINT('Ctrl Pts',(0.93417826195316,-0.499739406633171,
59.7428981735142));
#41446=CARTESIAN_POINT('Ctrl Pts',(1.05942882546267,0.00713467400835743,
59.7666735388114));
#41447=CARTESIAN_POINT('Ctrl Pts',(0.927356096326115,0.51227749022626,59.7904489041085));
#41448=CARTESIAN_POINT('Ctrl Pts',(0.570091202696139,0.892995264566529,
59.8142242694056));
#41449=CARTESIAN_POINT('Ctrl Pts',(0.0742928706965789,1.05682828433461,
59.8379996347028));
#41450=CARTESIAN_POINT('Ctrl Pts',(-0.268131168947707,0.994883332089929,
59.8538498782343));
#41451=CARTESIAN_POINT('Ctrl Pts',(-0.421648628688828,0.924896675066913,
59.861775));
#41452=CARTESIAN_POINT('Origin',(0.,0.,55.5071980324285));
#41453=CARTESIAN_POINT('',(-1.01640413103388,1.46689242105851E-5,59.2571980324285));
#41454=CARTESIAN_POINT('',(-1.01655516419051,1.02265252880131E-5,59.3163519675715));
#41455=CARTESIAN_POINT('',(-1.016475,-7.2179708060976E-14,55.5071980324285));
#41456=CARTESIAN_POINT('Ctrl Pts',(-1.01640413103388,1.466892421053E-5,
59.2571980324285));
#41457=CARTESIAN_POINT('Ctrl Pts',(-1.01635229931583,-0.101136172511406,
59.2619484599909));
#41458=CARTESIAN_POINT('Ctrl Pts',(-0.97631632561138,-0.371076743491578,
59.2746240093191));
#41459=CARTESIAN_POINT('Ctrl Pts',(-0.740834982929712,-0.75736088781519,
59.295224680413));
#41460=CARTESIAN_POINT('Ctrl Pts',(-0.289135652993162,-1.01923135768715,
59.3190000457102));
#41461=CARTESIAN_POINT('Ctrl Pts',(0.232786921381965,-1.0335580465354,59.3427754110073));
#41462=CARTESIAN_POINT('Ctrl Pts',(0.698171837004391,-0.796861388410206,
59.3665507763045));
#41463=CARTESIAN_POINT('Ctrl Pts',(0.993989661666965,-0.36662861157061,
59.3903261416016));
#41464=CARTESIAN_POINT('Ctrl Pts',(1.04839423183335,0.152648357301901,59.4141015068988));
#41465=CARTESIAN_POINT('Ctrl Pts',(0.848172146135856,0.634851161168593,
59.4378768721959));
#41466=CARTESIAN_POINT('Ctrl Pts',(0.441951943904046,0.962865756797002,
59.4616522374931));
#41467=CARTESIAN_POINT('Ctrl Pts',(-0.0716064543484882,1.05702625417764,
59.4854276027902));
#41468=CARTESIAN_POINT('Ctrl Pts',(-0.567773577890534,0.894463610514046,
59.5092029680874));
#41469=CARTESIAN_POINT('Ctrl Pts',(-0.926043827475508,0.514659903303883,
59.5329783333845));
#41470=CARTESIAN_POINT('Ctrl Pts',(-1.01578073897235,0.174981389455853,
59.5489766881649));
#41471=CARTESIAN_POINT('Ctrl Pts',(-1.01656332437151,0.00315563151131057,
59.5570499211796));
#41472=CARTESIAN_POINT('Ctrl Pts',(-1.01656273641868,3.31682248125081E-6,
59.5571980324285));
#41473=CARTESIAN_POINT('Ctrl Pts',(-1.01655516419051,1.02265252880044E-5,
59.3163519675715));
#41474=CARTESIAN_POINT('Ctrl Pts',(-1.01647249299314,-0.158661120223924,
59.3238069662019));
#41475=CARTESIAN_POINT('Ctrl Pts',(-0.938544820984173,-0.486088226810543,
59.339187086598));
#41476=CARTESIAN_POINT('Ctrl Pts',(-0.602081804228732,-0.871739348642251,
59.3624923287598));
#41477=CARTESIAN_POINT('Ctrl Pts',(-0.112602098016971,-1.05344803311272,
59.3862676940569));
#41478=CARTESIAN_POINT('Ctrl Pts',(0.404225617853905,-0.979302629822281,
59.4100430593541));
#41479=CARTESIAN_POINT('Ctrl Pts',(0.822877844024298,-0.667311055587846,
59.4338184246512));
#41480=CARTESIAN_POINT('Ctrl Pts',(1.04167525640482,-0.193247641021974,
59.4575937899483));
#41481=CARTESIAN_POINT('Ctrl Pts',(1.00747787145168,0.327750408428632,59.4813691552455));
#41482=CARTESIAN_POINT('Ctrl Pts',(0.728591308296158,0.769146732015046,
59.5051445205427));
#41483=CARTESIAN_POINT('Ctrl Pts',(0.272749589451039,1.02373807828526,59.5289198858398));
#41484=CARTESIAN_POINT('Ctrl Pts',(-0.24933564917612,1.02969108371093,59.552695251137));
#41485=CARTESIAN_POINT('Ctrl Pts',(-0.710863972995126,0.785559920997844,
59.5764706164341));
#41486=CARTESIAN_POINT('Ctrl Pts',(-0.968680817552861,0.397402752328119,
59.5976895219123));
#41487=CARTESIAN_POINT('Ctrl Pts',(-1.01633676570997,0.114283080288451,
59.6109833056248));
#41488=CARTESIAN_POINT('Ctrl Pts',(-1.01643175349457,-2.29197629572769E-5,
59.6163519675715));
#41489=CARTESIAN_POINT('Origin',(0.,0.,55.5071980324285));
#41490=CARTESIAN_POINT('',(-1.01648394848381,-2.59106389257236E-5,58.9571980324285));
#41491=CARTESIAN_POINT('',(-1.01639539183857,9.00667040512615E-6,59.0163519675715));
#41492=CARTESIAN_POINT('',(-1.016475,-7.2179708060976E-14,55.5071980324285));
#41493=CARTESIAN_POINT('Ctrl Pts',(-1.01648394848381,-2.59106389257809E-5,
58.9571980324285));
#41494=CARTESIAN_POINT('Ctrl Pts',(-1.01652163933797,-0.0367234553380025,
58.9589218770366));
#41495=CARTESIAN_POINT('Ctrl Pts',(-1.00561255230259,-0.242110267978689,
58.9685708434104));
#41496=CARTESIAN_POINT('Ctrl Pts',(-0.870637541598082,-0.603673966214107,
58.98614493155));
#41497=CARTESIAN_POINT('Ctrl Pts',(-0.476580245647126,-0.946204658508691,
59.0099202968471));
#41498=CARTESIAN_POINT('Ctrl Pts',(0.0332255259359154,-1.05892778353904,
59.0336956621443));
#41499=CARTESIAN_POINT('Ctrl Pts',(0.534961714244608,-0.914465937373881,
59.0574710274415));
#41500=CARTESIAN_POINT('Ctrl Pts',(0.906770144298739,-0.547905002471288,
59.0812463927386));
#41501=CARTESIAN_POINT('Ctrl Pts',(1.05834858599332,-0.0482727340283605,
59.1050217580358));
#41502=CARTESIAN_POINT('Ctrl Pts',(0.952882727939887,0.463083678311449,
59.1287971233329));
#41503=CARTESIAN_POINT('Ctrl Pts',(0.615987379842406,0.861969566863883,
59.15257248863));
#41504=CARTESIAN_POINT('Ctrl Pts',(0.129485326732331,1.05150631785341,59.1763478539272));
#41505=CARTESIAN_POINT('Ctrl Pts',(-0.388465216580355,0.985660571308298,
59.2001232192243));
#41506=CARTESIAN_POINT('Ctrl Pts',(-0.812068046017044,0.680424481454538,
59.2238985845215));
#41507=CARTESIAN_POINT('Ctrl Pts',(-0.99321101668419,0.303938289486403,
59.2429235222562));
#41508=CARTESIAN_POINT('Ctrl Pts',(-1.01643876999062,0.0676134241395438,
59.2540233382252));
#41509=CARTESIAN_POINT('Ctrl Pts',(-1.01640413103388,1.466892421053E-5,
59.2571980324285));
#41510=CARTESIAN_POINT('Ctrl Pts',(-1.01639539183857,9.00667040507064E-6,
59.0163519675715));
#41511=CARTESIAN_POINT('Ctrl Pts',(-1.01636604337103,-0.0942875579157628,
59.0207803832475));
#41512=CARTESIAN_POINT('Ctrl Pts',(-0.980065909154692,-0.357360013679804,
59.0331339206893));
#41513=CARTESIAN_POINT('Ctrl Pts',(-0.756005693342733,-0.742217880800317,
59.0534125798968));
#41514=CARTESIAN_POINT('Ctrl Pts',(-0.3096967726728,-1.01317318358827,59.0771879451939));
#41515=CARTESIAN_POINT('Ctrl Pts',(0.211829133326388,-1.03805607229115,
59.1009633104911));
#41516=CARTESIAN_POINT('Ctrl Pts',(0.681907461502236,-0.810823164995865,
59.1247386757882));
#41517=CARTESIAN_POINT('Ctrl Pts',(0.986368876446939,-0.386663200373609,
59.1485140410854));
#41518=CARTESIAN_POINT('Ctrl Pts',(1.0512679198866,0.131406817036291,59.1722894063825));
#41519=CARTESIAN_POINT('Ctrl Pts',(0.860842366221901,0.617561666122401,
59.1960647716797));
#41520=CARTESIAN_POINT('Ctrl Pts',(0.461341441599518,0.953727458558869,
59.2198401369768));
#41521=CARTESIAN_POINT('Ctrl Pts',(-0.0502068645469796,1.05825859868873,
59.243615502274));
#41522=CARTESIAN_POINT('Ctrl Pts',(-0.549561278709315,0.905767294557619,
59.2673908675711));
#41523=CARTESIAN_POINT('Ctrl Pts',(-0.91544209454521,0.533289567195347,
59.2911662328683));
#41524=CARTESIAN_POINT('Ctrl Pts',(-1.01397691023297,0.188697018515519,
59.3074865995351));
#41525=CARTESIAN_POINT('Ctrl Pts',(-1.01656037755733,0.0100162741080625,
59.3158818444361));
#41526=CARTESIAN_POINT('Ctrl Pts',(-1.01655516419051,1.02265252880044E-5,
59.3163519675715));
#41527=CARTESIAN_POINT('Origin',(0.,0.,55.5071980324285));
#41528=CARTESIAN_POINT('',(-1.01651187699763,2.32118305695883E-5,58.6571980324285));
#41529=CARTESIAN_POINT('',(-1.01650544524628,-2.41045256057504E-5,58.7163519675715));
#41530=CARTESIAN_POINT('',(-1.016475,-7.2179708060976E-14,55.5071980324285));
#41531=CARTESIAN_POINT('Ctrl Pts',(-1.01651187699763,2.32118305695597E-5,
58.6571980324285));
#41532=CARTESIAN_POINT('Ctrl Pts',(-1.01637337542594,-0.140944227048892,
58.663820415848));
#41533=CARTESIAN_POINT('Ctrl Pts',(-0.951395035985954,-0.450733549321653,
58.6783679210332));
#41534=CARTESIAN_POINT('Ctrl Pts',(-0.646842124418696,-0.839063318470144,
58.7008405479841));
#41535=CARTESIAN_POINT('Ctrl Pts',(-0.167533788876386,-1.04611873891511,
58.7246159132813));
#41536=CARTESIAN_POINT('Ctrl Pts',(0.352463981145058,-0.999100159303358,
58.7483912785784));
#41537=CARTESIAN_POINT('Ctrl Pts',(0.786857765467602,-0.709427123281846,
58.7721666438756));
#41538=CARTESIAN_POINT('Ctrl Pts',(1.03014504102483,-0.247453391119582,
58.7959420091728));
#41539=CARTESIAN_POINT('Ctrl Pts',(1.0232378965077,0.274620089350941,58.8197173744699));
#41540=CARTESIAN_POINT('Ctrl Pts',(0.767813890850171,0.729995763920686,
58.8434927397671));
#41541=CARTESIAN_POINT('Ctrl Pts',(0.325908619452451,1.00807517482141,58.8672681050642));
#41542=CARTESIAN_POINT('Ctrl Pts',(-0.195151057192915,1.04132034033774,
58.8910434703614));
#41543=CARTESIAN_POINT('Ctrl Pts',(-0.66881381045679,0.821656907271453,
58.9148188356585));
#41544=CARTESIAN_POINT('Ctrl Pts',(-0.95747415469737,0.432831070855505,
58.9368703563476));
#41545=CARTESIAN_POINT('Ctrl Pts',(-1.01634836118557,0.131988103044408,
58.9509967552709));
#41546=CARTESIAN_POINT('Ctrl Pts',(-1.01648394848381,-2.59106389257809E-5,
58.9571980324285));
#41547=CARTESIAN_POINT('Ctrl Pts',(-1.01650544524628,-2.41045256058059E-5,
58.7163519675715));
#41548=CARTESIAN_POINT('Ctrl Pts',(-1.01653538170935,-0.0298647776898298,
58.7177538002932));
#41549=CARTESIAN_POINT('Ctrl Pts',(-1.00796629632303,-0.228389592496974,
58.7270807547806));
#41550=CARTESIAN_POINT('Ctrl Pts',(-0.882672410895779,-0.585936349776809,
58.7443328310337));
#41551=CARTESIAN_POINT('Ctrl Pts',(-0.495625581575281,-0.936369197397321,
58.7681081963309));
#41552=CARTESIAN_POINT('Ctrl Pts',(0.0117953213153582,-1.05938324573377,
58.7918835616281));
#41553=CARTESIAN_POINT('Ctrl Pts',(0.516351459091809,-0.925101703403523,
58.8156589269252));
#41554=CARTESIAN_POINT('Ctrl Pts',(0.895499767177114,-0.566137931896525,
58.8394342922223));
#41555=CARTESIAN_POINT('Ctrl Pts',(1.05715535724409,-0.0696745405184991,
58.8632096575195));
#41556=CARTESIAN_POINT('Ctrl Pts',(0.962056450613156,0.443710915777326,
58.8869850228166));
#41557=CARTESIAN_POINT('Ctrl Pts',(0.633300004359957,0.84933096930703,58.9107603881138));
#41558=CARTESIAN_POINT('Ctrl Pts',(0.150732083980457,1.04867145942151,58.934535753411));
#41559=CARTESIAN_POINT('Ctrl Pts',(-0.368444590347487,0.993317962582985,
58.9583111187081));
#41560=CARTESIAN_POINT('Ctrl Pts',(-0.798136020423016,0.696714348818546,
58.9820864840053));
#41561=CARTESIAN_POINT('Ctrl Pts',(-0.990052970920145,0.31766096707036,
59.0014334336264));
#41562=CARTESIAN_POINT('Ctrl Pts',(-1.01641856558121,0.0744661931108326,
59.0128552614818));
#41563=CARTESIAN_POINT('Ctrl Pts',(-1.01639539183857,9.00667040507064E-6,
59.0163519675715));
#41564=CARTESIAN_POINT('Origin',(0.,0.,55.5071980324285));
#41565=CARTESIAN_POINT('',(-1.0163935740239,-7.14493009090905E-6,58.3571980324285));
#41566=CARTESIAN_POINT('',(-1.01649061196631,2.55351377537877E-5,58.4163519675715));
#41567=CARTESIAN_POINT('',(-1.016475,-7.2179708060976E-14,55.5071980324285));
#41568=CARTESIAN_POINT('Ctrl Pts',(-1.0163935740239,-7.14493009100481E-6,
58.3571980324285));
#41569=CARTESIAN_POINT('Ctrl Pts',(-1.01641243716347,-0.0765747908146764,
58.3607938328937));
#41570=CARTESIAN_POINT('Ctrl Pts',(-0.989051004929182,-0.321883779780578,
58.3723147551245));
#41571=CARTESIAN_POINT('Ctrl Pts',(-0.793782635482674,-0.701670231612259,
58.3917607991211));
#41572=CARTESIAN_POINT('Ctrl Pts',(-0.362252808929985,-0.995592732369494,
58.4155361644183));
#41573=CARTESIAN_POINT('Ctrl Pts',(0.157258445325715,-1.04771263603068,
58.4393115297154));
#41574=CARTESIAN_POINT('Ctrl Pts',(0.63857586865163,-0.845371425055543,
58.4630868950126));
#41575=CARTESIAN_POINT('Ctrl Pts',(0.964800452845084,-0.437712317069721,
58.4868622603097));
#41576=CARTESIAN_POINT('Ctrl Pts',(1.0567010533528,0.0762552959977839,58.5106376256069));
#41577=CARTESIAN_POINT('Ctrl Pts',(0.891957495313147,0.571702556299444,
58.534412990904));
#41578=CARTESIAN_POINT('Ctrl Pts',(0.51058154146171,0.928298699688416,58.5581883562012));
#41579=CARTESIAN_POINT('Ctrl Pts',(0.00519911514345259,1.059436149811,58.5819637214983));
#41580=CARTESIAN_POINT('Ctrl Pts',(-0.501446035884838,0.93326516029476,
58.6057390867955));
#41581=CARTESIAN_POINT('Ctrl Pts',(-0.886303482123542,0.580429258308285,
58.6295144520927));
#41582=CARTESIAN_POINT('Ctrl Pts',(-1.00866188976917,0.224167479511998,
58.6466674339703));
#41583=CARTESIAN_POINT('Ctrl Pts',(-1.01653912267294,0.0277539662379626,
58.6558952940823));
#41584=CARTESIAN_POINT('Ctrl Pts',(-1.01651187699763,2.32118305695597E-5,
58.6571980324285));
#41585=CARTESIAN_POINT('Ctrl Pts',(-1.01649061196631,2.55351377537773E-5,
58.4163519675715));
#41586=CARTESIAN_POINT('Ctrl Pts',(-1.01635293586417,-0.134095487665188,
58.4226523391046));
#41587=CARTESIAN_POINT('Ctrl Pts',(-0.956068712269705,-0.437044966876974,
58.4368778324033));
#41588=CARTESIAN_POINT('Ctrl Pts',(-0.66368501246902,-0.825805179912512,
58.4590284474679));
#41589=CARTESIAN_POINT('Ctrl Pts',(-0.188663761430564,-1.0425152162291,
58.482803812765));
#41590=CARTESIAN_POINT('Ctrl Pts',(0.33217882398349,-1.00602645086662,58.5065791780622));
#41591=CARTESIAN_POINT('Ctrl Pts',(0.772344140743365,-0.725201019859825,
58.5303545433593));
#41592=CARTESIAN_POINT('Ctrl Pts',(1.02492791636524,-0.268243839074722,
58.5541299086565));
#41593=CARTESIAN_POINT('Ctrl Pts',(1.02858437064807,0.253862528556006,58.5779052739536));
#41594=CARTESIAN_POINT('Ctrl Pts',(0.782425449558309,0.714312541419944,
58.6016806392508));
#41595=CARTESIAN_POINT('Ctrl Pts',(0.346236509580231,1.00127532196696,58.625456004548));
#41596=CARTESIAN_POINT('Ctrl Pts',(-0.174043931374068,1.04505535781517,
58.6492313698451));
#41597=CARTESIAN_POINT('Ctrl Pts',(-0.652053799988115,0.83501966016819,
58.6730067351423));
#41598=CARTESIAN_POINT('Ctrl Pts',(-0.952850717014485,0.44652188822276,
58.6953802677177));
#41599=CARTESIAN_POINT('Ctrl Pts',(-1.01636613889499,0.13883649796031,58.7098286785275));
#41600=CARTESIAN_POINT('Ctrl Pts',(-1.01650544524628,-2.41045256058059E-5,
58.7163519675715));
#41601=CARTESIAN_POINT('Origin',(0.,0.,55.5071980324285));
#41602=CARTESIAN_POINT('',(-1.0165515244855,-1.2203389089734E-5,58.0571980324285));
#41603=CARTESIAN_POINT('',(-1.01640099228082,-1.30015508006398E-5,58.1163519675715));
#41604=CARTESIAN_POINT('',(-1.016475,-7.2179708060976E-14,55.5071980324285));
#41605=CARTESIAN_POINT('Ctrl Pts',(-1.0165515244855,-1.22033890897957E-5,
58.0571980324285));
#41606=CARTESIAN_POINT('Ctrl Pts',(-1.01655885755325,-0.0121274903681481,
58.0577672499393));
#41607=CARTESIAN_POINT('Ctrl Pts',(-1.01339368204511,-0.192918087923177,
58.0662615892159));
#41608=CARTESIAN_POINT('Ctrl Pts',(-0.912103957994839,-0.538978994149835,
58.0826810502581));
#41609=CARTESIAN_POINT('Ctrl Pts',(-0.543911098024301,-0.909171438052593,
58.1064564155553));
#41610=CARTESIAN_POINT('Ctrl Pts',(-0.0436169160818455,-1.0585506841697,
58.1302317808524));
#41611=CARTESIAN_POINT('Ctrl Pts',(0.467270637269431,-0.950836546347711,
58.1540071461496));
#41612=CARTESIAN_POINT('Ctrl Pts',(0.864670767536001,-0.612189880750512,
58.1777825114467));
#41613=CARTESIAN_POINT('Ctrl Pts',(1.05206571151958,-0.124858820150662,
58.2015578767439));
#41614=CARTESIAN_POINT('Ctrl Pts',(0.983942296348724,0.392797077102948,
58.2253332420411));
#41615=CARTESIAN_POINT('Ctrl Pts',(0.676845860469362,0.815053168505043,
58.2491086073382));
#41616=CARTESIAN_POINT('Ctrl Pts',(0.205361837603814,1.03935484892341,58.2728839726354));
#41617=CARTESIAN_POINT('Ctrl Pts',(-0.315999031548909,1.01122529556216,
58.2966593379325));
#41618=CARTESIAN_POINT('Ctrl Pts',(-0.760612266830792,0.737496417531059,
58.3204347032296));
#41619=CARTESIAN_POINT('Ctrl Pts',(-0.981188751078297,0.353138397649337,
58.3406142680616));
#41620=CARTESIAN_POINT('Ctrl Pts',(-1.01637086292167,0.09217982247098,58.3528687111279));
#41621=CARTESIAN_POINT('Ctrl Pts',(-1.0163935740239,-7.14493009100481E-6,
58.3571980324285));
#41622=CARTESIAN_POINT('Ctrl Pts',(-1.01640099228083,-1.3001550800619E-5,
58.1163519675715));
#41623=CARTESIAN_POINT('Ctrl Pts',(-1.01643252806871,-0.0697223898558531,
58.1196257561502));
#41624=CARTESIAN_POINT('Ctrl Pts',(-0.992255076331624,-0.308161297059955,
58.1308246664947));
#41625=CARTESIAN_POINT('Ctrl Pts',(-0.807815818999105,-0.685467427031471,
58.1499486986049));
#41626=CARTESIAN_POINT('Ctrl Pts',(-0.382320725410081,-0.988060146887956,
58.173724063902));
#41627=CARTESIAN_POINT('Ctrl Pts',(0.136029751029905,-1.05067973130782,
58.1974994291992));
#41628=CARTESIAN_POINT('Ctrl Pts',(0.62134227328246,-0.858117573749964,
58.2212747944964));
#41629=CARTESIAN_POINT('Ctrl Pts',(0.955747531469626,-0.457141823765944,
58.2450501597935));
#41630=CARTESIAN_POINT('Ctrl Pts',(1.05802751617526,0.0548613339460823,
58.2688255250907));
#41631=CARTESIAN_POINT('Ctrl Pts',(0.903341180323916,0.553540154710871,
58.2926008903878));
#41632=CARTESIAN_POINT('Ctrl Pts',(0.5292576588922,0.917779015586153,58.316376255685));
#41633=CARTESIAN_POINT('Ctrl Pts',(0.0266317402610465,1.05911413046801,
58.3401516209821));
#41634=CARTESIAN_POINT('Ctrl Pts',(-0.482462309113668,0.94321901551604,
58.3639269862793));
#41635=CARTESIAN_POINT('Ctrl Pts',(-0.874379288435858,0.598241465380611,
58.3877023515764));
#41636=CARTESIAN_POINT('Ctrl Pts',(-1.00635212941563,0.237887822759668,
58.4051773453405));
#41637=CARTESIAN_POINT('Ctrl Pts',(-1.01652611610726,0.0346128863531156,
58.4147272173389));
#41638=CARTESIAN_POINT('Ctrl Pts',(-1.01649061196631,2.55351377537773E-5,
58.4163519675715));
#41639=CARTESIAN_POINT('Origin',(0.,0.,55.5071980324285));
#41640=CARTESIAN_POINT('',(-1.01643729572907,2.38158822067048E-5,57.7571980324285));
#41641=CARTESIAN_POINT('',(-1.01656116828543,-5.50351341488398E-6,57.8163519675715));
#41642=CARTESIAN_POINT('',(-1.016475,-7.2179708060976E-14,55.5071980324285));
#41643=CARTESIAN_POINT('Ctrl Pts',(-1.01643729572907,2.38158822067069E-5,
57.7571980324285));
#41644=CARTESIAN_POINT('Ctrl Pts',(-1.01633594492437,-0.116390217672064,
57.7626657887507));
#41645=CARTESIAN_POINT('Ctrl Pts',(-0.967402991324987,-0.401621088357726,
57.7760586668386));
#41646=CARTESIAN_POINT('Ctrl Pts',(-0.705959114011145,-0.789970705576619,
57.7973766666922));
#41647=CARTESIAN_POINT('Ctrl Pts',(-0.242919704987064,-1.03122354669277,
57.8211520319894));
#41648=CARTESIAN_POINT('Ctrl Pts',(0.2791183423777,-1.02202002782379,57.8449273972865));
#41649=CARTESIAN_POINT('Ctrl Pts',(0.73336607961892,-0.764595435239446,
57.8687027625837));
#41650=CARTESIAN_POINT('Ctrl Pts',(1.00949899449501,-0.321471252895473,
57.8924781278809));
#41651=CARTESIAN_POINT('Ctrl Pts',(1.04045185662625,0.199729618153172,57.916253493178));
#41652=CARTESIAN_POINT('Ctrl Pts',(0.818707051422304,0.672421556968558,
57.9400288584752));
#41653=CARTESIAN_POINT('Ctrl Pts',(0.398120405716357,0.981800452677053,
57.9638042237723));
#41654=CARTESIAN_POINT('Ctrl Pts',(-0.11915893864965,1.05272652368244,57.9875795890695));
#41655=CARTESIAN_POINT('Ctrl Pts',(-0.607497793701196,0.867973742098689,
58.0113549543666));
#41656=CARTESIAN_POINT('Ctrl Pts',(-0.940132720180615,0.481883868106556,
58.034561102153));
#41657=CARTESIAN_POINT('Ctrl Pts',(-1.01645676045732,0.156551657251636,
58.0498421281736));
#41658=CARTESIAN_POINT('Ctrl Pts',(-1.0165515244855,-1.22033890897957E-5,
58.0571980324285));
#41659=CARTESIAN_POINT('Ctrl Pts',(-1.01656116828543,-5.50351341484581E-6,
57.8163519675715));
#41660=CARTESIAN_POINT('Ctrl Pts',(-1.01656274467139,-0.00526690962334575,
57.8165991731959));
#41661=CARTESIAN_POINT('Ctrl Pts',(-1.01524049810908,-0.179202016646892,
57.824771500586));
#41662=CARTESIAN_POINT('Ctrl Pts',(-0.922821481937435,-0.520415702512074,
57.8408689497419));
#41663=CARTESIAN_POINT('Ctrl Pts',(-0.562193425992196,-0.897981371030322,
57.864644315039));
#41664=CARTESIAN_POINT('Ctrl Pts',(-0.0650237641719233,-1.05745160694911,
57.8884196803362));
#41665=CARTESIAN_POINT('Ctrl Pts',(0.447938414546611,-0.960095395114365,
57.9121950456334));
#41666=CARTESIAN_POINT('Ctrl Pts',(0.852108445175959,-0.629557931096218,
57.9359704109305));
#41667=CARTESIAN_POINT('Ctrl Pts',(1.04932433848386,-0.146117841524369,
57.9597457762276));
#41668=CARTESIAN_POINT('Ctrl Pts',(0.991687678140017,0.372810327072094,
57.9835211415248));
#41669=CARTESIAN_POINT('Ctrl Pts',(0.693196852949359,0.80119293182569,58.007296506822));
#41670=CARTESIAN_POINT('Ctrl Pts',(0.226347226119961,1.03498740290602,58.0310718721191));
#41671=CARTESIAN_POINT('Ctrl Pts',(-0.295476031333513,1.01741137493825,
58.0548472374163));
#41672=CARTESIAN_POINT('Ctrl Pts',(-0.745536137617694,0.752733590623157,
58.0786226027134));
#41673=CARTESIAN_POINT('Ctrl Pts',(-0.977486684416592,0.366855908733197,
58.0991241794318));
#41674=CARTESIAN_POINT('Ctrl Pts',(-1.01635618686555,0.0990286999729323,
58.1117006343845));
#41675=CARTESIAN_POINT('Ctrl Pts',(-1.01640099228083,-1.3001550800619E-5,
58.1163519675715));
#41676=CARTESIAN_POINT('Origin',(0.,0.,55.5071980324285));
#41677=CARTESIAN_POINT('',(-1.01643822360686,-2.39497420581337E-5,57.4571980324285));
#41678=CARTESIAN_POINT('',(-1.0164203332823,2.04341709851841E-5,57.5163519675715));
#41679=CARTESIAN_POINT('',(-1.016475,-7.2179708060976E-14,55.5071980324285));
#41680=CARTESIAN_POINT('Ctrl Pts',(-1.01643822360686,-2.39497420582019E-5,
57.4571980324285));
#41681=CARTESIAN_POINT('Ctrl Pts',(-1.01648379076976,-0.0519988508214108,
57.4596392057963));
#41682=CARTESIAN_POINT('Ctrl Pts',(-0.999851515608375,-0.272678234287765,
57.4700055009299));
#41683=CARTESIAN_POINT('Ctrl Pts',(-0.842554347220154,-0.642288220587176,
57.4882969178293));
#41684=CARTESIAN_POINT('Ctrl Pts',(-0.433464221124387,-0.966716481358237,
57.5120722831264));
#41685=CARTESIAN_POINT('Ctrl Pts',(0.0809026622319955,-1.05635540684393,
57.5358476484236));
#41686=CARTESIAN_POINT('Ctrl Pts',(0.575620473027226,-0.889434121987983,
57.5596230137207));
#41687=CARTESIAN_POINT('Ctrl Pts',(0.930535610706933,-0.506493300578492,
57.5833983790179));
#41688=CARTESIAN_POINT('Ctrl Pts',(1.05944876982279,-0.000538930044200919,
57.607173744315));
#41689=CARTESIAN_POINT('Ctrl Pts',(0.931050424239669,0.505546332048563,
57.6309491096122));
#41690=CARTESIAN_POINT('Ctrl Pts',(0.576525065783793,0.888848038107536,
57.6547244749094));
#41691=CARTESIAN_POINT('Ctrl Pts',(0.0819773330527327,1.05627255156526,
57.6784998402065));
#41692=CARTESIAN_POINT('Ctrl Pts',(-0.432480480769399,0.967156977991728,
57.7022752055036));
#41693=CARTESIAN_POINT('Ctrl Pts',(-0.841900461305519,0.643145084392453,
57.7260505708008));
#41694=CARTESIAN_POINT('Ctrl Pts',(-0.999713158006665,0.273368272745295,
57.7443581797758));
#41695=CARTESIAN_POINT('Ctrl Pts',(-1.01648284566773,0.0523435986850332,
57.754740666985));
#41696=CARTESIAN_POINT('Ctrl Pts',(-1.01643729572907,2.38158822067069E-5,
57.7571980324285));
#41697=CARTESIAN_POINT('Ctrl Pts',(-1.0164203332823,2.04341709851633E-5,
57.5163519675715));
#41698=CARTESIAN_POINT('Ctrl Pts',(-1.01634044576945,-0.109542886279426,
57.5214977120073));
#41699=CARTESIAN_POINT('Ctrl Pts',(-0.971500612426874,-0.387911922967112,
57.5345685782088));
#41700=CARTESIAN_POINT('Ctrl Pts',(-0.721796698973036,-0.775526605796326,
57.555564566176));
#41701=CARTESIAN_POINT('Ctrl Pts',(-0.263732900340999,-1.02609792331145,
57.5793399314732));
#41702=CARTESIAN_POINT('Ctrl Pts',(0.258384499898145,-1.02745775638647,
57.6031152967703));
#41703=CARTESIAN_POINT('Ctrl Pts',(0.717747280609244,-0.779275838278319,
57.6268906620675));
#41704=CARTESIAN_POINT('Ctrl Pts',(1.00278862358054,-0.341828856833032,
57.6506660273646));
#41705=CARTESIAN_POINT('Ctrl Pts',(1.04427968174507,0.178639125727723,57.6744413926618));
#41706=CARTESIAN_POINT('Ctrl Pts',(0.832143397191218,0.655720487294243,
57.6982167579589));
#41707=CARTESIAN_POINT('Ctrl Pts',(0.417901946483455,0.973545044706037,
57.7219921232561));
#41708=CARTESIAN_POINT('Ctrl Pts',(-0.0978366051027944,1.05492179314312,
57.7457674885532));
#41709=CARTESIAN_POINT('Ctrl Pts',(-0.589813286563081,0.880086517303837,
57.7695428538504));
#41710=CARTESIAN_POINT('Ctrl Pts',(-0.934914336585201,0.495542314056757,
57.7930710135232));
#41711=CARTESIAN_POINT('Ctrl Pts',(-1.01651220759037,0.163407586277906,
57.8086740514302));
#41712=CARTESIAN_POINT('Ctrl Pts',(-1.01656116828543,-5.50351341484581E-6,
57.8163519675715));
#41713=CARTESIAN_POINT('Origin',(0.,0.,55.5071980324285));
#41714=CARTESIAN_POINT('',(-1.01655087939569,1.25177289053898E-5,57.1571980324285));
#41715=CARTESIAN_POINT('',(-1.01645785338958,-2.58202779849781E-5,57.2163519675715));
#41716=CARTESIAN_POINT('',(-1.016475,-7.2179708060976E-14,55.5071980324285));
#41717=CARTESIAN_POINT('Ctrl Pts',(-1.01655087939569,1.25177289053684E-5,
57.1571980324285));
#41718=CARTESIAN_POINT('Ctrl Pts',(-1.01645429891022,-0.156206996899727,
57.1645377446077));
#41719=CARTESIAN_POINT('Ctrl Pts',(-0.940390670028725,-0.481196778392105,
57.1798025785527));
#41720=CARTESIAN_POINT('Ctrl Pts',(-0.608380536643186,-0.867355238041698,
57.2029925342634));
#41721=CARTESIAN_POINT('Ctrl Pts',(-0.120229897725971,-1.05260474919004,
57.2267678995606));
#41722=CARTESIAN_POINT('Ctrl Pts',(0.397121337553111,-0.982204983485956,
57.2505432648577));
#41723=CARTESIAN_POINT('Ctrl Pts',(0.818022520857566,-0.673254143466235,
57.2743186301549));
#41724=CARTESIAN_POINT('Ctrl Pts',(1.04024811765422,-0.200788047556321,
57.298093995452));
#41725=CARTESIAN_POINT('Ctrl Pts',(1.00982552981173,0.320444044514911,57.3218693607492));
#41726=CARTESIAN_POINT('Ctrl Pts',(0.734143582611297,0.763848929065998,
57.3456447260463));
#41727=CARTESIAN_POINT('Ctrl Pts',(0.280157978558803,1.02173553005387,57.3694200913435));
#41728=CARTESIAN_POINT('Ctrl Pts',(-0.241870435179003,1.03147015415423,
57.3931954566406));
#41729=CARTESIAN_POINT('Ctrl Pts',(-0.705155049885808,0.79068852397462,
57.4169708219378));
#41730=CARTESIAN_POINT('Ctrl Pts',(-0.967192769783646,0.402310326406248,
57.4383050138671));
#41731=CARTESIAN_POINT('Ctrl Pts',(-1.01633585973001,0.116734523561822,
57.4517140840306));
#41732=CARTESIAN_POINT('Ctrl Pts',(-1.01643822360686,-2.39497420582019E-5,
57.4571980324285));
#41733=CARTESIAN_POINT('Ctrl Pts',(-1.01645785338958,-2.58202779849365E-5,
57.2163519675715));
#41734=CARTESIAN_POINT('Ctrl Pts',(-1.01650184768103,-0.0451422806476026,
57.218471129053));
#41735=CARTESIAN_POINT('Ctrl Pts',(-1.00252655417846,-0.2589557093226,57.2285154123001));
#41736=CARTESIAN_POINT('Ctrl Pts',(-0.855376177906754,-0.62511085834112,
57.246484817313));
#41737=CARTESIAN_POINT('Ctrl Pts',(-0.452933360879266,-0.957749112006351,
57.2702601826102));
#41738=CARTESIAN_POINT('Ctrl Pts',(0.0595147418551541,-1.0577759623135,
57.2940355479073));
#41739=CARTESIAN_POINT('Ctrl Pts',(0.557508320487304,-0.900897587705596,
57.3178109132045));
#41740=CARTESIAN_POINT('Ctrl Pts',(0.920098178889751,-0.525215510195677,
57.3415862785016));
#41741=CARTESIAN_POINT('Ctrl Pts',(1.0592210291418,-0.0219727642805258,
57.3653616437988));
#41742=CARTESIAN_POINT('Ctrl Pts',(0.941087686758059,0.486606572888925,
57.3891370090959));
#41743=CARTESIAN_POINT('Ctrl Pts',(0.594389551407591,0.877002310215783,
57.4129123743931));
#41744=CARTESIAN_POINT('Ctrl Pts',(0.103330240503893,1.05439786245219,57.4366877396903));
#41745=CARTESIAN_POINT('Ctrl Pts',(-0.412825196255343,0.975708639032718,
57.4604631049874));
#41746=CARTESIAN_POINT('Ctrl Pts',(-0.828716537711619,0.660046127986225,
57.4842384702846));
#41747=CARTESIAN_POINT('Ctrl Pts',(-0.996884749609738,0.287091239458341,
57.5028680911459));
#41748=CARTESIAN_POINT('Ctrl Pts',(-1.01646348302378,0.0591990064556959,
57.5135725902416));
#41749=CARTESIAN_POINT('Ctrl Pts',(-1.0164203332823,2.04341709851633E-5,
57.5163519675715));
#41750=CARTESIAN_POINT('Origin',(0.,0.,55.5071980324285));
#41751=CARTESIAN_POINT('',(-1.01639331761686,6.83678408873587E-6,56.8571980324285));
#41752=CARTESIAN_POINT('',(-1.01653552617529,1.81671041117951E-5,56.9163519675715));
#41753=CARTESIAN_POINT('',(-1.016475,-7.2179708060976E-14,55.5071980324285));
#41754=CARTESIAN_POINT('Ctrl Pts',(-1.01639331761686,6.83678408874844E-6,
56.8571980324285));
#41755=CARTESIAN_POINT('Ctrl Pts',(-1.01637167394885,-0.0918354088346601,
56.8615111616534));
#41756=CARTESIAN_POINT('Ctrl Pts',(-0.981370841868257,-0.352448563742444,
56.873749412644));
#41757=CARTESIAN_POINT('Ctrl Pts',(-0.761362185779602,-0.736722205712254,
56.8939127854004));
#41758=CARTESIAN_POINT('Ctrl Pts',(-0.317027666320693,-1.01090328177916,
56.9176881506975));
#41759=CARTESIAN_POINT('Ctrl Pts',(0.204304314625503,-1.03956324163084,
56.9414635159947));
#41760=CARTESIAN_POINT('Ctrl Pts',(0.676016293066456,-0.815741354740158,
56.9652388812919));
#41761=CARTESIAN_POINT('Ctrl Pts',(0.98354216404791,-0.393797915007909,
56.989014246589));
#41762=CARTESIAN_POINT('Ctrl Pts',(1.05219219565452,0.123788407083776,57.0127896118862));
#41763=CARTESIAN_POINT('Ctrl Pts',(0.865293148524952,0.611309866958155,
57.0365649771833));
#41764=CARTESIAN_POINT('Ctrl Pts',(0.468237755572337,0.950360663422683,
57.0603403424805));
#41765=CARTESIAN_POINT('Ctrl Pts',(-0.0425399473918753,1.05859451122728,
57.0841157077776));
#41766=CARTESIAN_POINT('Ctrl Pts',(-0.54298584556759,0.90972433068368,57.1078910730748));
#41767=CARTESIAN_POINT('Ctrl Pts',(-0.911555140614478,0.539906669660545,
57.1316664383719));
#41768=CARTESIAN_POINT('Ctrl Pts',(-1.01329712113469,0.193607825789528,
57.1481020914898));
#41769=CARTESIAN_POINT('Ctrl Pts',(-1.01655858257814,0.0124724615555045,
57.156612622842));
#41770=CARTESIAN_POINT('Ctrl Pts',(-1.01655087939569,1.25177289053684E-5,
57.1571980324285));
#41771=CARTESIAN_POINT('Ctrl Pts',(-1.01653552617529,1.81671041117881E-5,
56.9163519675715));
#41772=CARTESIAN_POINT('Ctrl Pts',(-1.01641141768326,-0.14935414160094,
56.9233696678643));
#41773=CARTESIAN_POINT('Ctrl Pts',(-0.94543258794415,-0.46752734399196,
56.9383124899229));
#41774=CARTESIAN_POINT('Ctrl Pts',(-0.62580367676965,-0.854869433941773,
56.9611804337472));
#41775=CARTESIAN_POINT('Ctrl Pts',(-0.141500771893025,-1.04995691459222,
56.9849557990443));
#41776=CARTESIAN_POINT('Ctrl Pts',(0.377168850439841,-0.990038205931583,
57.0087311643415));
#41777=CARTESIAN_POINT('Ctrl Pts',(0.804234341269022,-0.689665944693458,
57.0325065296386));
#41778=CARTESIAN_POINT('Ctrl Pts',(1.0359730221788,-0.221792444109516,57.0562818949358));
#41779=CARTESIAN_POINT('Ctrl Pts',(1.01610182372747,0.29994845351169,57.0800572602329));
#41780=CARTESIAN_POINT('Ctrl Pts',(0.749446923564514,0.748839969356621,
57.1038326255301));
#41781=CARTESIAN_POINT('Ctrl Pts',(0.300771598169799,1.0158584727612,57.1276079908272));
#41782=CARTESIAN_POINT('Ctrl Pts',(-0.220953028616557,1.03615237783422,
57.1513833561244));
#41783=CARTESIAN_POINT('Ctrl Pts',(-0.689014129727543,0.804792842899423,
57.1751587214215));
#41784=CARTESIAN_POINT('Ctrl Pts',(-0.962928490231453,0.416014631120328,
57.1968149252373));
#41785=CARTESIAN_POINT('Ctrl Pts',(-1.01633732028666,0.123581738355737,
57.2105460072872));
#41786=CARTESIAN_POINT('Ctrl Pts',(-1.01645785338958,-2.58202779849365E-5,
57.2163519675715));
#41787=CARTESIAN_POINT('Origin',(0.,0.,55.5071980324285));
#41788=CARTESIAN_POINT('',(-1.0165129144013,-2.30512370967894E-5,56.5571980324285));
#41789=CARTESIAN_POINT('',(-1.01639061276947,5.63170237111166E-7,56.6163519675715));
#41790=CARTESIAN_POINT('',(-1.016475,-7.2179708060976E-14,55.5071980324285));
#41791=CARTESIAN_POINT('Ctrl Pts',(-1.0165129144013,-2.30512370968383E-5,
56.5571980324285));
#41792=CARTESIAN_POINT('Ctrl Pts',(-1.01653971143184,-0.0274090521408874,
56.5584845786991));
#41793=CARTESIAN_POINT('Ctrl Pts',(-1.00877426909957,-0.223477594555612,
56.5676962467354));
#41794=CARTESIAN_POINT('Ctrl Pts',(-0.886893539358715,-0.579527252302758,
56.5848330365374));
#41795=CARTESIAN_POINT('Ctrl Pts',(-0.502395259761104,-0.932754517168359,
56.6086084018346));
#41796=CARTESIAN_POINT('Ctrl Pts',(0.00412126548291853,-1.05944089098629,
56.6323837671317));
#41797=CARTESIAN_POINT('Ctrl Pts',(0.509636846599777,-0.928817673665269,
56.6561591324289));
#41798=CARTESIAN_POINT('Ctrl Pts',(0.89137539612891,-0.572609718307843,
56.679934497726));
#41799=CARTESIAN_POINT('Ctrl Pts',(1.05662292602311,-0.0773303208768799,
56.7037098630232));
#41800=CARTESIAN_POINT('Ctrl Pts',(0.965245272389302,0.436730523841399,
56.7274852283203));
#41801=CARTESIAN_POINT('Ctrl Pts',(0.639435600411005,0.844721314547941,
56.7512605936175));
#41802=CARTESIAN_POINT('Ctrl Pts',(0.158324283665738,1.04755210253542,56.7750359589146));
#41803=CARTESIAN_POINT('Ctrl Pts',(-0.361239727368135,0.995960765138673,
56.7988113242118));
#41804=CARTESIAN_POINT('Ctrl Pts',(-0.793068360860628,0.702477445421887,
56.8225866895089));
#41805=CARTESIAN_POINT('Ctrl Pts',(-0.988885930748487,0.322573781877596,
56.8420489255812));
#41806=CARTESIAN_POINT('Ctrl Pts',(-1.01641144291832,0.0769193262567779,
56.8535860398877));
#41807=CARTESIAN_POINT('Ctrl Pts',(-1.01639331761686,6.83678408874844E-6,
56.8571980324285));
#41808=CARTESIAN_POINT('Ctrl Pts',(-1.01639061276947,5.63170237152799E-7,
56.6163519675715));
#41809=CARTESIAN_POINT('Ctrl Pts',(-1.01638896833711,-0.0849855231432444,
56.62034308491));
#41810=CARTESIAN_POINT('Ctrl Pts',(-0.984911757328215,-0.338728827146233,
56.6322593240142));
#41811=CARTESIAN_POINT('Ctrl Pts',(-0.776111149103991,-0.721168132395479,
56.6521006848841));
#41812=CARTESIAN_POINT('Ctrl Pts',(-0.337414590176968,-1.00428252264095,
56.6758760501813));
#41813=CARTESIAN_POINT('Ctrl Pts',(0.18323086366488,-1.043483800328,56.6996514154785));
#41814=CARTESIAN_POINT('Ctrl Pts',(0.659374487328757,-0.82925103340682,
56.7234267807756));
#41815=CARTESIAN_POINT('Ctrl Pts',(0.975373848875025,-0.41361557741103,
56.7472021460728));
#41816=CARTESIAN_POINT('Ctrl Pts',(1.05448123428539,0.102475936132846,56.77097751137));
#41817=CARTESIAN_POINT('Ctrl Pts',(0.877483595272346,0.593678811289621,
56.7947528766671));
#41818=CARTESIAN_POINT('Ctrl Pts',(0.48736888002166,0.940693130480272,56.8185282419642));
#41819=CARTESIAN_POINT('Ctrl Pts',(-0.02111457889448,1.0592384837724,56.8423036072614));
#41820=CARTESIAN_POINT('Ctrl Pts',(-0.524469876618518,0.920523405170176,
56.8660789725585));
#41821=CARTESIAN_POINT('Ctrl Pts',(-0.900445600203663,0.558238042433696,
56.8898543378557));
#41822=CARTESIAN_POINT('Ctrl Pts',(-1.01130302005036,0.207325373739056,
56.90661200286));
#41823=CARTESIAN_POINT('Ctrl Pts',(-1.01655157398383,0.0193327053028336,
56.9154445460986));
#41824=CARTESIAN_POINT('Ctrl Pts',(-1.01653552617529,1.81671041117881E-5,
56.9163519675715));
#41825=CARTESIAN_POINT('Origin',(0.,0.,55.5071980324285));
#41826=CARTESIAN_POINT('',(-1.01648283811887,2.60095369413545E-5,56.2571980324285));
#41827=CARTESIAN_POINT('',(-1.01653237544382,-1.90345246380841E-5,56.3163519675715));
#41828=CARTESIAN_POINT('',(-1.016475,-7.2179708060976E-14,55.5071980324285));
#41829=CARTESIAN_POINT('Ctrl Pts',(-1.01648283811887,2.60095369413633E-5,
56.2571980324285));
#41830=CARTESIAN_POINT('Ctrl Pts',(-1.01634766438916,-0.131643710346183,
56.2633831175105));
#41831=CARTESIAN_POINT('Ctrl Pts',(-0.957702373223059,-0.432142526414999,
56.2774933243581));
#41832=CARTESIAN_POINT('Ctrl Pts',(-0.669649384741906,-0.820976009905639,
56.2995286529715));
#41833=CARTESIAN_POINT('Ctrl Pts',(-0.196210379601176,-1.04112127560369,
56.3233040182687));
#41834=CARTESIAN_POINT('Ctrl Pts',(0.324882860612091,-1.00840621766713,
56.3470793835659));
#41835=CARTESIAN_POINT('Ctrl Pts',(0.767070810376454,-0.730776546609132,
56.370854748863));
#41836=CARTESIAN_POINT('Ctrl Pts',(1.02295797523586,-0.275660965237961,
56.3946301141602));
#41837=CARTESIAN_POINT('Ctrl Pts',(1.03039626118959,0.246405215445278,56.4184054794573));
#41838=CARTESIAN_POINT('Ctrl Pts',(0.787579113904559,0.708626224754583,
56.4421808447545));
#41839=CARTESIAN_POINT('Ctrl Pts',(0.353480261128564,0.998741052994776,
56.4659562100516));
#41840=CARTESIAN_POINT('Ctrl Pts',(-0.166469404010035,1.04628864277636,
56.4897315753488));
#41841=CARTESIAN_POINT('Ctrl Pts',(-0.645988145161798,0.839720967104466,
56.5135069406459));
#41842=CARTESIAN_POINT('Ctrl Pts',(-0.951155699582826,0.451421666720772,
56.5359957596725));
#41843=CARTESIAN_POINT('Ctrl Pts',(-1.01637464179167,0.141288644010153,
56.5505594569333));
#41844=CARTESIAN_POINT('Ctrl Pts',(-1.0165129144013,-2.30512370968383E-5,
56.5571980324285));
#41845=CARTESIAN_POINT('Ctrl Pts',(-1.01653237544382,-1.90345246380841E-5,
56.3163519675715));
#41846=CARTESIAN_POINT('Ctrl Pts',(-1.01655003026065,-0.0205494097757443,
56.3173165019557));
#41847=CARTESIAN_POINT('Ctrl Pts',(-1.01093463056855,-0.209758496430707,
56.3262061581056));
#41848=CARTESIAN_POINT('Ctrl Pts',(-0.898436564193858,-0.561465699584117,
56.3430209360212));
#41849=CARTESIAN_POINT('Ctrl Pts',(-0.521163199217816,-0.922399539433787,
56.3667963013183));
#41850=CARTESIAN_POINT('Ctrl Pts',(-0.0173133632032956,-1.05930743344434,
56.3905716666155));
#41851=CARTESIAN_POINT('Ctrl Pts',(0.49074142153069,-0.938938149241069,
56.4143470319126));
#41852=CARTESIAN_POINT('Ctrl Pts',(0.879608363221454,-0.590526136845567,
56.4381223972097));
#41853=CARTESIAN_POINT('Ctrl Pts',(1.05484217994403,-0.0986912679291979,
56.4618977625069));
#41854=CARTESIAN_POINT('Ctrl Pts',(0.973883308267136,0.417113045610174,
56.4856731278041));
#41855=CARTESIAN_POINT('Ctrl Pts',(0.656394472537722,0.831611861009717,
56.5094484931012));
#41856=CARTESIAN_POINT('Ctrl Pts',(0.179485139828959,1.0441346060376,56.5332238583984));
#41857=CARTESIAN_POINT('Ctrl Pts',(-0.341016287857761,1.00306524332296,
56.5569992236956));
#41858=CARTESIAN_POINT('Ctrl Pts',(-0.778694065497443,0.718378412332483,
56.5807745889927));
#41859=CARTESIAN_POINT('Ctrl Pts',(-0.985523871362989,0.336295280666352,
56.6005588369514));
#41860=CARTESIAN_POINT('Ctrl Pts',(-1.01639223367,0.0837704981166061,56.6124179631443));
#41861=CARTESIAN_POINT('Ctrl Pts',(-1.01639061276947,5.63170237152799E-7,
56.6163519675715));
#41862=CARTESIAN_POINT('Origin',(1.39932914042665E-16,0.,59.861775));
#41863=CARTESIAN_POINT('',(0.672748867539255,-0.97943229058963,59.861775));
#41864=CARTESIAN_POINT('Ctrl Pts',(-1.01184089351566,-0.0973166075163435,
59.861775));
#41865=CARTESIAN_POINT('Ctrl Pts',(-1.0114437912448,-0.126338627735325,
59.861775));
#41866=CARTESIAN_POINT('Ctrl Pts',(-1.0097970940642,-0.15529997051701,59.861775));
#41867=CARTESIAN_POINT('Ctrl Pts',(-1.00689935402508,-0.184119087090023,
59.861775));
#41868=CARTESIAN_POINT('Ctrl Pts',(-1.00255508251114,-0.227324504241121,
59.861775));
#41869=CARTESIAN_POINT('Ctrl Pts',(-0.99540135320563,-0.270210478356502,
59.861775));
#41870=CARTESIAN_POINT('Ctrl Pts',(-0.98556589048639,-0.312540257335641,
59.861775));
#41871=CARTESIAN_POINT('Ctrl Pts',(-0.981595087308391,-0.329629765546126,
59.861775));
#41872=CARTESIAN_POINT('Ctrl Pts',(-0.977186645817288,-0.346628644562582,
59.861775));
#41873=CARTESIAN_POINT('Ctrl Pts',(-0.97234684431464,-0.363521208153442,
59.861775));
#41874=CARTESIAN_POINT('Ctrl Pts',(-0.969416300323676,-0.3737498096149,
59.861775));
#41875=CARTESIAN_POINT('Ctrl Pts',(-0.966329907396498,-0.383931170219947,
59.861775));
#41876=CARTESIAN_POINT('Ctrl Pts',(-0.963090796052553,-0.394058609457477,
59.861775));
#41877=CARTESIAN_POINT('Ctrl Pts',(-0.949182573622318,-0.43754420245124,
59.861775));
#41878=CARTESIAN_POINT('Ctrl Pts',(-0.93245720400045,-0.480055494132926,
59.861775));
#41879=CARTESIAN_POINT('Ctrl Pts',(-0.91305514527965,-0.5213247168299,59.861775));
#41880=CARTESIAN_POINT('Ctrl Pts',(-0.900416920921426,-0.548206899954864,
59.861775));
#41881=CARTESIAN_POINT('Ctrl Pts',(-0.886641870555354,-0.574562125052264,
59.861775));
#41882=CARTESIAN_POINT('Ctrl Pts',(-0.87175731975576,-0.600313985396109,
59.861775));
#41883=CARTESIAN_POINT('Ctrl Pts',(-0.864826659378796,-0.612304767013991,
59.861775));
#41884=CARTESIAN_POINT('Ctrl Pts',(-0.857652040875426,-0.624169497956551,
59.861775));
#41885=CARTESIAN_POINT('Ctrl Pts',(-0.85025378976052,-0.635872550479802,
59.861775));
#41886=CARTESIAN_POINT('Ctrl Pts',(-0.843281093125467,-0.646902432229058,
59.861775));
#41887=CARTESIAN_POINT('Ctrl Pts',(-0.836107645721068,-0.657792743080534,
59.861775));
#41888=CARTESIAN_POINT('Ctrl Pts',(-0.828736935305739,-0.668537604860453,
59.861775));
#41889=CARTESIAN_POINT('Ctrl Pts',(-0.802624452178946,-0.7066038164083,
59.861775));
#41890=CARTESIAN_POINT('Ctrl Pts',(-0.774040170525397,-0.742845924874012,
59.861775));
#41891=CARTESIAN_POINT('Ctrl Pts',(-0.743254711167329,-0.777114570540984,
59.861775));
#41892=CARTESIAN_POINT('Ctrl Pts',(-0.7121921018527,-0.811691723985851,
59.861775));
#41893=CARTESIAN_POINT('Ctrl Pts',(-0.678887800198998,-0.844260574715302,
59.861775));
#41894=CARTESIAN_POINT('Ctrl Pts',(-0.643572524360008,-0.874642276826878,
59.861775));
#41895=CARTESIAN_POINT('Ctrl Pts',(-0.623233617211618,-0.892139821545903,
59.861775));
#41896=CARTESIAN_POINT('Ctrl Pts',(-0.602226877710127,-0.908911380096442,
59.861775));
#41897=CARTESIAN_POINT('Ctrl Pts',(-0.580590775824314,-0.924917292668666,
59.861775));
#41898=CARTESIAN_POINT('Ctrl Pts',(-0.573562898026258,-0.930116362177473,
59.861775));
#41899=CARTESIAN_POINT('Ctrl Pts',(-0.566476752841383,-0.935228569208567,
59.861775));
#41900=CARTESIAN_POINT('Ctrl Pts',(-0.559334318108606,-0.940252829215512,
59.861775));
#41901=CARTESIAN_POINT('Ctrl Pts',(-0.520393486038798,-0.967645290263513,
59.861775));
#41902=CARTESIAN_POINT('Ctrl Pts',(-0.479780846242934,-0.992427501112665,
59.861775));
#41903=CARTESIAN_POINT('Ctrl Pts',(-0.437755592288797,-1.01443282934249,
59.861775));
#41904=CARTESIAN_POINT('Ctrl Pts',(-0.433388015774203,-1.01671978648681,
59.861775));
#41905=CARTESIAN_POINT('Ctrl Pts',(-0.429005145199489,-1.01897672231071,
59.861775));
#41906=CARTESIAN_POINT('Ctrl Pts',(-0.424607247138309,-1.02120342891482,
59.861775));
#41907=CARTESIAN_POINT('Ctrl Pts',(-0.382868534019858,-1.04233622163878,
59.861775));
#41908=CARTESIAN_POINT('Ctrl Pts',(-0.339778626521477,-1.06074970180182,
59.861775));
#41909=CARTESIAN_POINT('Ctrl Pts',(-0.29562133015478,-1.07641531260368,
59.861775));
#41910=CARTESIAN_POINT('Ctrl Pts',(-0.274591715400399,-1.08387595415473,
59.861775));
#41911=CARTESIAN_POINT('Ctrl Pts',(-0.253319595741797,-1.09071274018422,
59.861775));
#41912=CARTESIAN_POINT('Ctrl Pts',(-0.231833867236195,-1.09691905016394,
59.861775));
#41913=CARTESIAN_POINT('Ctrl Pts',(-0.220247415251091,-1.10026588164634,
59.861775));
#41914=CARTESIAN_POINT('Ctrl Pts',(-0.208598829633676,-1.10342932737445,
59.861775));
#41915=CARTESIAN_POINT('Ctrl Pts',(-0.19689255768268,-1.10640805572873,
59.861775));
#41916=CARTESIAN_POINT('Ctrl Pts',(-0.187496090203694,-1.10879904102506,
59.861775));
#41917=CARTESIAN_POINT('Ctrl Pts',(-0.178069361414857,-1.11106918282397,
59.861775));
#41918=CARTESIAN_POINT('Ctrl Pts',(-0.168622313084257,-1.11321671711805,
59.861775));
#41919=CARTESIAN_POINT('Ctrl Pts',(-0.121098578018619,-1.12401996986586,
59.861775));
#41920=CARTESIAN_POINT('Ctrl Pts',(-0.073005361777424,-1.13173889035925,
59.861775));
#41921=CARTESIAN_POINT('Ctrl Pts',(-0.0246593521685011,-1.13636033806869,
59.861775));
#41922=CARTESIAN_POINT('Ctrl Pts',(0.0230683985636239,-1.14092268573879,
59.861775));
#41923=CARTESIAN_POINT('Ctrl Pts',(0.0710436278401751,-1.1424664914666,
59.861775));
#41924=CARTESIAN_POINT('Ctrl Pts',(0.118980208527935,-1.14093288136104,
59.861775));
#41925=CARTESIAN_POINT('Ctrl Pts',(0.14321229178875,-1.14015763691861,59.861775));
#41926=CARTESIAN_POINT('Ctrl Pts',(0.167434691953048,-1.13859524577042,
59.861775));
#41927=CARTESIAN_POINT('Ctrl Pts',(0.191613851491352,-1.13625725196546,
59.861775));
#41928=CARTESIAN_POINT('Ctrl Pts',(0.207199962167851,-1.13475015945684,
59.861775));
#41929=CARTESIAN_POINT('Ctrl Pts',(0.222768107495521,-1.132920720623,59.861775));
#41930=CARTESIAN_POINT('Ctrl Pts',(0.238309236150123,-1.13077131215,59.861775));
#41931=CARTESIAN_POINT('Ctrl Pts',(0.247294863295863,-1.12952855922314,
59.861775));
#41932=CARTESIAN_POINT('Ctrl Pts',(0.256270239073691,-1.12817889864578,
59.861775));
#41933=CARTESIAN_POINT('Ctrl Pts',(0.265221037989145,-1.12672513730018,
59.861775));
#41934=CARTESIAN_POINT('Ctrl Pts',(0.313867380575837,-1.11882414732982,
59.861775));
#41935=CARTESIAN_POINT('Ctrl Pts',(0.361886766975759,-1.10783931741569,
59.861775));
#41936=CARTESIAN_POINT('Ctrl Pts',(0.409003407702753,-1.0939199257479,59.861775));
#41937=CARTESIAN_POINT('Ctrl Pts',(0.456548635540028,-1.07987391911436,
59.861775));
#41938=CARTESIAN_POINT('Ctrl Pts',(0.503175704622686,-1.06283956339786,
59.861775));
#41939=CARTESIAN_POINT('Ctrl Pts',(0.548601290212343,-1.04291756028592,
59.861775));
#41940=CARTESIAN_POINT('Ctrl Pts',(0.591117300761962,-1.02427159054261,
59.861775));
#41941=CARTESIAN_POINT('Ctrl Pts',(0.632581562956363,-1.0030954173452,59.861775));
#41942=CARTESIAN_POINT('Ctrl Pts',(0.672748867539255,-0.97943229058963,
59.861775));
#41943=CARTESIAN_POINT('',(-1.188225,-1.45515594291687E-16,59.861775));
#41944=CARTESIAN_POINT('Origin',(0.,0.,59.861775));
#41945=CARTESIAN_POINT('',(1.18460912750413,-0.0928893956975266,59.861775));
#41946=CARTESIAN_POINT('Origin',(0.,0.,59.861775));
#41947=CARTESIAN_POINT('Ctrl Pts',(1.18463057630127,-0.0928773270330193,
59.861775));
#41948=CARTESIAN_POINT('Ctrl Pts',(1.18495917433816,-0.0591973510751312,
59.861775));
#41949=CARTESIAN_POINT('Ctrl Pts',(1.18384723794147,-0.0255569108469606,
59.861775));
#41950=CARTESIAN_POINT('Ctrl Pts',(1.18127296688008,0.00795555060754574,
59.861775));
#41951=CARTESIAN_POINT('Ctrl Pts',(1.17757694805885,0.0560711861906696,
59.861775));
#41952=CARTESIAN_POINT('Ctrl Pts',(1.17086819176842,0.103924041630274,59.861775));
#41953=CARTESIAN_POINT('Ctrl Pts',(1.16122381979749,0.151244181532205,59.861775));
#41954=CARTESIAN_POINT('Ctrl Pts',(1.15737804746034,0.170113474999273,59.861775));
#41955=CARTESIAN_POINT('Ctrl Pts',(1.15306501652236,0.188897877747367,59.861775));
#41956=CARTESIAN_POINT('Ctrl Pts',(1.14828781990542,0.207579342678793,59.861775));
#41957=CARTESIAN_POINT('Ctrl Pts',(1.14557847714315,0.218174362281078,59.861775));
#41958=CARTESIAN_POINT('Ctrl Pts',(1.14272017734302,0.228734422458591,59.861775));
#41959=CARTESIAN_POINT('Ctrl Pts',(1.1397169789668,0.239245168892212,59.861775));
#41960=CARTESIAN_POINT('Ctrl Pts',(1.12618741947878,0.286596609364257,59.861775));
#41961=CARTESIAN_POINT('Ctrl Pts',(1.10970488146276,0.333012630300466,59.861775));
#41962=CARTESIAN_POINT('Ctrl Pts',(1.09035192020453,0.378202802308839,59.861775));
#41963=CARTESIAN_POINT('Ctrl Pts',(1.07747056795985,0.408281430373587,59.861775));
#41964=CARTESIAN_POINT('Ctrl Pts',(1.06331654234041,0.437816614433228,59.861775));
#41965=CARTESIAN_POINT('Ctrl Pts',(1.04790356112901,0.466715221191892,59.861775));
#41966=CARTESIAN_POINT('Ctrl Pts',(1.04254300086328,0.476766016751856,59.861775));
#41967=CARTESIAN_POINT('Ctrl Pts',(1.03703008545209,0.486739745783998,59.861775));
#41968=CARTESIAN_POINT('Ctrl Pts',(1.03136517466139,0.496632265600078,59.861775));
#41969=CARTESIAN_POINT('Ctrl Pts',(1.02625122763606,0.505562648470277,59.861775));
#41970=CARTESIAN_POINT('Ctrl Pts',(1.02101800912316,0.514418756608124,59.861775));
#41971=CARTESIAN_POINT('Ctrl Pts',(1.01566821899752,0.523194987724883,59.861775));
#41972=CARTESIAN_POINT('Ctrl Pts',(1.00990493839165,0.532649542277472,59.861775));
#41973=CARTESIAN_POINT('Ctrl Pts',(1.00400570856243,0.54201255557472,59.861775));
#41974=CARTESIAN_POINT('Ctrl Pts',(0.997971579640927,0.551280810079599,
59.861775));
#41975=CARTESIAN_POINT('Ctrl Pts',(0.971594934033771,0.591794605467841,
59.861775));
#41976=CARTESIAN_POINT('Ctrl Pts',(0.942643848491387,0.630500527183138,
59.861775));
#41977=CARTESIAN_POINT('Ctrl Pts',(0.911348678913813,0.667203480005342,
59.861775));
#41978=CARTESIAN_POINT('Ctrl Pts',(0.880279653768076,0.703641210797284,
59.861775));
#41979=CARTESIAN_POINT('Ctrl Pts',(0.846899360884351,0.738105471913161,
59.861775));
#41980=CARTESIAN_POINT('Ctrl Pts',(0.811401841668893,0.770365388497151,
59.861775));
#41981=CARTESIAN_POINT('Ctrl Pts',(0.792170102127397,0.787843069391074,
59.861775));
#41982=CARTESIAN_POINT('Ctrl Pts',(0.77231644980281,0.804672975392104,59.861775));
#41983=CARTESIAN_POINT('Ctrl Pts',(0.751869309712643,0.820812397933032,
59.861775));
#41984=CARTESIAN_POINT('Ctrl Pts',(0.744749793833871,0.826432004124786,
59.861775));
#41985=CARTESIAN_POINT('Ctrl Pts',(0.737558154141825,0.831967832124177,
59.861775));
#41986=CARTESIAN_POINT('Ctrl Pts',(0.730307446536889,0.83740945949028,59.861775));
#41987=CARTESIAN_POINT('Ctrl Pts',(0.692551663872584,0.865745024978379,
59.861775));
#41988=CARTESIAN_POINT('Ctrl Pts',(0.653119323526253,0.891591843549213,
59.861775));
#41989=CARTESIAN_POINT('Ctrl Pts',(0.612212142191562,0.914751484082298,
59.861775));
#41990=CARTESIAN_POINT('Ctrl Pts',(0.605291188285646,0.918669788873226,
59.861775));
#41991=CARTESIAN_POINT('Ctrl Pts',(0.59832796009732,0.922511069601298,59.861775));
#41992=CARTESIAN_POINT('Ctrl Pts',(0.591323369627692,0.926274231416198,
59.861775));
#41993=CARTESIAN_POINT('Ctrl Pts',(0.551834952455115,0.947489076777823,
59.861775));
#41994=CARTESIAN_POINT('Ctrl Pts',(0.511032589468169,0.966224558513573,
59.861775));
#41995=CARTESIAN_POINT('Ctrl Pts',(0.469164126081047,0.982399610517108,
59.861775));
#41996=CARTESIAN_POINT('Ctrl Pts',(0.449995116427187,0.989805177928087,
59.861775));
#41997=CARTESIAN_POINT('Ctrl Pts',(0.430602536035571,0.996673459296994,
59.861775));
#41998=CARTESIAN_POINT('Ctrl Pts',(0.41101004444375,1.00299367986045,59.861775));
#41999=CARTESIAN_POINT('Ctrl Pts',(0.396644935535153,1.00762763140739,59.861775));
#42000=CARTESIAN_POINT('Ctrl Pts',(0.382172358715336,1.01196692045316,59.861775));
#42001=CARTESIAN_POINT('Ctrl Pts',(0.367601731133845,1.01600663591634,59.861775));
#42002=CARTESIAN_POINT('Ctrl Pts',(0.359081682696219,1.01836882458859,59.861775));
#42003=CARTESIAN_POINT('Ctrl Pts',(0.350536793205264,1.0206261443741,59.861775));
#42004=CARTESIAN_POINT('Ctrl Pts',(0.341971425877663,1.02277764435025,59.861775));
#42005=CARTESIAN_POINT('Ctrl Pts',(0.297265461380135,1.03400715475785,59.861775));
#42006=CARTESIAN_POINT('Ctrl Pts',(0.251980969497039,1.04236390172438,59.861775));
#42007=CARTESIAN_POINT('Ctrl Pts',(0.206392409752112,1.04777705832953,59.861775));
#42008=CARTESIAN_POINT('Ctrl Pts',(0.162531617113603,1.05298506096674,59.861775));
#42009=CARTESIAN_POINT('Ctrl Pts',(0.118388411378249,1.05546820201981,59.861775));
#42010=CARTESIAN_POINT('Ctrl Pts',(0.0742092780586676,1.05511789517874,
59.861775));
#42011=CARTESIAN_POINT('Ctrl Pts',(0.0525758589890548,1.05494635866078,
59.861775));
#42012=CARTESIAN_POINT('Ctrl Pts',(0.0309339423407732,1.05409468861183,
59.861775));
#42013=CARTESIAN_POINT('Ctrl Pts',(0.00931474303316654,1.05256641039276,
59.861775));
#42014=CARTESIAN_POINT('Ctrl Pts',(-0.00776915395261585,1.0513587362653,
59.861775));
#42015=CARTESIAN_POINT('Ctrl Pts',(-0.0248388516191337,1.04972850975678,
59.861775));
#42016=CARTESIAN_POINT('Ctrl Pts',(-0.0418783779732828,1.04767648714608,
59.861775));
#42017=CARTESIAN_POINT('Ctrl Pts',(-0.0506706059106654,1.04661766366994,
59.861775));
#42018=CARTESIAN_POINT('Ctrl Pts',(-0.0594452838937768,1.04544765251369,
59.861775));
#42019=CARTESIAN_POINT('Ctrl Pts',(-0.0681982225184759,1.04416754258846,
59.861775));
#42020=CARTESIAN_POINT('Ctrl Pts',(-0.112958009502046,1.03762146132072,
59.861775));
#42021=CARTESIAN_POINT('Ctrl Pts',(-0.157169095981507,1.02819814056938,
59.861775));
#42022=CARTESIAN_POINT('Ctrl Pts',(-0.200557341352607,1.01597710620675,
59.861775));
#42023=CARTESIAN_POINT('Ctrl Pts',(-0.243177930293229,1.00397229528288,
59.861775));
#42024=CARTESIAN_POINT('Ctrl Pts',(-0.285005500695438,0.989267371338,59.861775));
#42025=CARTESIAN_POINT('Ctrl Pts',(-0.325758763954662,0.97189347978409,
59.861775));
#42026=CARTESIAN_POINT('Ctrl Pts',(-0.358468307116102,0.957948779158524,
59.861775));
#42027=CARTESIAN_POINT('Ctrl Pts',(-0.390485567095365,0.942283809933677,
59.861775));
#42028=CARTESIAN_POINT('Ctrl Pts',(-0.421648628688828,0.924896675066913,
59.861775));
#42029=CARTESIAN_POINT('Ctrl Pts',(-0.437855924241139,0.917335061595237,
55.9626150912667));
#42030=CARTESIAN_POINT('Ctrl Pts',(-0.59011828195518,0.844658263165578,
55.9705402130324));
#42031=CARTESIAN_POINT('Ctrl Pts',(-0.857585956829971,0.622054483027012,
55.9863904565638));
#42032=CARTESIAN_POINT('Ctrl Pts',(-1.05057757445303,0.136862273787097,
56.010165821861));
#42033=CARTESIAN_POINT('Ctrl Pts',(-0.988364686858664,-0.381513829574367,
56.0339411871581));
#42034=CARTESIAN_POINT('Ctrl Pts',(-0.686123743003436,-0.807263618083567,
56.0577165524553));
#42035=CARTESIAN_POINT('Ctrl Pts',(-0.217232371214364,-1.03693712275359,
56.0814919177525));
#42036=CARTESIAN_POINT('Ctrl Pts',(0.304414618904077,-1.01477332192588,
56.1052672830496));
#42037=CARTESIAN_POINT('Ctrl Pts',(0.752129524692829,-0.746145432160931,
56.1290426483468));
#42038=CARTESIAN_POINT('Ctrl Pts',(1.01717154895307,-0.296300389836015,
56.1528180136439));
#42039=CARTESIAN_POINT('Ctrl Pts',(1.03517049480264,0.225508677645759,56.1765933789411));
#42040=CARTESIAN_POINT('Ctrl Pts',(0.801754274033107,0.69254746844306,56.2003687442382));
#42041=CARTESIAN_POINT('Ctrl Pts',(0.373613677358384,0.991385317760177,
56.2241441095354));
#42042=CARTESIAN_POINT('Ctrl Pts',(-0.14526763822163,1.04944237138876,56.2479194748325));
#42043=CARTESIAN_POINT('Ctrl Pts',(-0.628867346267627,0.852618234981034,
56.2716948401297));
#42044=CARTESIAN_POINT('Ctrl Pts',(-0.959732162422036,0.448716132860876,
56.2954702054268));
#42045=CARTESIAN_POINT('Ctrl Pts',(-1.0575039415156,-0.0641669975384679,
56.319245570724));
#42046=CARTESIAN_POINT('Ctrl Pts',(-0.898436564193858,-0.561465699584117,
56.3430209360212));
#42047=CARTESIAN_POINT('Ctrl Pts',(-0.521163199217816,-0.922399539433787,
56.3667963013183));
#42048=CARTESIAN_POINT('Ctrl Pts',(-0.0173133632032956,-1.05930743344434,
56.3905716666155));
#42049=CARTESIAN_POINT('Ctrl Pts',(0.49074142153069,-0.938938149241069,
56.4143470319126));
#42050=CARTESIAN_POINT('Ctrl Pts',(0.879608363221454,-0.590526136845567,
56.4381223972097));
#42051=CARTESIAN_POINT('Ctrl Pts',(1.05484217994403,-0.0986912679291979,
56.4618977625069));
#42052=CARTESIAN_POINT('Ctrl Pts',(0.973883308267136,0.417113045610174,
56.4856731278041));
#42053=CARTESIAN_POINT('Ctrl Pts',(0.656394472537722,0.831611861009717,
56.5094484931012));
#42054=CARTESIAN_POINT('Ctrl Pts',(0.179485139828959,1.0441346060376,56.5332238583984));
#42055=CARTESIAN_POINT('Ctrl Pts',(-0.341016287857761,1.00306524332296,
56.5569992236956));
#42056=CARTESIAN_POINT('Ctrl Pts',(-0.778694065497443,0.718378412332483,
56.5807745889927));
#42057=CARTESIAN_POINT('Ctrl Pts',(-1.02724807670217,0.259216858745684,
56.6045499542899));
#42058=CARTESIAN_POINT('Ctrl Pts',(-1.02631126225859,-0.262901471862694,
56.628325319587));
#42059=CARTESIAN_POINT('Ctrl Pts',(-0.776111149103991,-0.721168132395479,
56.6521006848841));
#42060=CARTESIAN_POINT('Ctrl Pts',(-0.337414590176968,-1.00428252264095,
56.6758760501813));
#42061=CARTESIAN_POINT('Ctrl Pts',(0.18323086366488,-1.043483800328,56.6996514154785));
#42062=CARTESIAN_POINT('Ctrl Pts',(0.659374487328757,-0.82925103340682,
56.7234267807756));
#42063=CARTESIAN_POINT('Ctrl Pts',(0.975373848875025,-0.41361557741103,
56.7472021460728));
#42064=CARTESIAN_POINT('Ctrl Pts',(1.05448123428539,0.102475936132846,56.77097751137));
#42065=CARTESIAN_POINT('Ctrl Pts',(0.877483595272346,0.593678811289621,
56.7947528766671));
#42066=CARTESIAN_POINT('Ctrl Pts',(0.48736888002166,0.940693130480272,56.8185282419642));
#42067=CARTESIAN_POINT('Ctrl Pts',(-0.02111457889448,1.0592384837724,56.8423036072614));
#42068=CARTESIAN_POINT('Ctrl Pts',(-0.524469876618518,0.920523405170176,
56.8660789725585));
#42069=CARTESIAN_POINT('Ctrl Pts',(-0.900445600203663,0.558238042433696,
56.8898543378557));
#42070=CARTESIAN_POINT('Ctrl Pts',(-1.05772739644889,0.0603717297067289,
56.9136297031529));
#42071=CARTESIAN_POINT('Ctrl Pts',(-0.958115763116474,-0.452157246335915,
56.93740506845));
#42072=CARTESIAN_POINT('Ctrl Pts',(-0.62580367676965,-0.854869433941773,
56.9611804337472));
#42073=CARTESIAN_POINT('Ctrl Pts',(-0.141500771893025,-1.04995691459222,
56.9849557990443));
#42074=CARTESIAN_POINT('Ctrl Pts',(0.377168850439841,-0.990038205931583,
57.0087311643415));
#42075=CARTESIAN_POINT('Ctrl Pts',(0.804234341269022,-0.689665944693458,
57.0325065296386));
#42076=CARTESIAN_POINT('Ctrl Pts',(1.0359730221788,-0.221792444109516,57.0562818949358));
#42077=CARTESIAN_POINT('Ctrl Pts',(1.01610182372747,0.29994845351169,57.0800572602329));
#42078=CARTESIAN_POINT('Ctrl Pts',(0.749446923564514,0.748839969356621,
57.1038326255301));
#42079=CARTESIAN_POINT('Ctrl Pts',(0.300771598169799,1.0158584727612,57.1276079908272));
#42080=CARTESIAN_POINT('Ctrl Pts',(-0.220953028616557,1.03615237783422,
57.1513833561244));
#42081=CARTESIAN_POINT('Ctrl Pts',(-0.689014129727543,0.804792842899423,
57.1751587214215));
#42082=CARTESIAN_POINT('Ctrl Pts',(-0.989732299751159,0.377970853076824,
57.1989340867187));
#42083=CARTESIAN_POINT('Ctrl Pts',(-1.05007121355009,-0.140650053038654,
57.2227094520158));
#42084=CARTESIAN_POINT('Ctrl Pts',(-0.855376177906754,-0.62511085834112,
57.246484817313));
#42085=CARTESIAN_POINT('Ctrl Pts',(-0.452933360879266,-0.957749112006351,
57.2702601826102));
#42086=CARTESIAN_POINT('Ctrl Pts',(0.0595147418551541,-1.0577759623135,
57.2940355479073));
#42087=CARTESIAN_POINT('Ctrl Pts',(0.557508320487304,-0.900897587705596,
57.3178109132045));
#42088=CARTESIAN_POINT('Ctrl Pts',(0.920098178889751,-0.525215510195677,
57.3415862785016));
#42089=CARTESIAN_POINT('Ctrl Pts',(1.0592210291418,-0.0219727642805258,
57.3653616437988));
#42090=CARTESIAN_POINT('Ctrl Pts',(0.941087686758059,0.486606572888925,
57.3891370090959));
#42091=CARTESIAN_POINT('Ctrl Pts',(0.594389551407591,0.877002310215783,
57.4129123743931));
#42092=CARTESIAN_POINT('Ctrl Pts',(0.103330240503893,1.05439786245219,57.4366877396903));
#42093=CARTESIAN_POINT('Ctrl Pts',(-0.412825196255343,0.975708639032718,
57.4604631049874));
#42094=CARTESIAN_POINT('Ctrl Pts',(-0.828716537711619,0.660046127986225,
57.4842384702846));
#42095=CARTESIAN_POINT('Ctrl Pts',(-1.04333500466809,0.18407623143842,57.5080138355817));
#42096=CARTESIAN_POINT('Ctrl Pts',(-1.00455556546515,-0.336600812297502,
57.5317892008789));
#42097=CARTESIAN_POINT('Ctrl Pts',(-0.721796698973036,-0.775526605796326,
57.555564566176));
#42098=CARTESIAN_POINT('Ctrl Pts',(-0.263732900340999,-1.02609792331145,
57.5793399314732));
#42099=CARTESIAN_POINT('Ctrl Pts',(0.258384499898145,-1.02745775638647,
57.6031152967703));
#42100=CARTESIAN_POINT('Ctrl Pts',(0.717747280609244,-0.779275838278319,
57.6268906620675));
#42101=CARTESIAN_POINT('Ctrl Pts',(1.00278862358054,-0.341828856833032,
57.6506660273646));
#42102=CARTESIAN_POINT('Ctrl Pts',(1.04427968174507,0.178639125727723,57.6744413926618));
#42103=CARTESIAN_POINT('Ctrl Pts',(0.832143397191218,0.655720487294243,
57.6982167579589));
#42104=CARTESIAN_POINT('Ctrl Pts',(0.417901946483455,0.973545044706037,
57.7219921232561));
#42105=CARTESIAN_POINT('Ctrl Pts',(-0.0978366051027944,1.05492179314312,
57.7457674885532));
#42106=CARTESIAN_POINT('Ctrl Pts',(-0.589813286563081,0.880086517303837,
57.7695428538504));
#42107=CARTESIAN_POINT('Ctrl Pts',(-0.93854024365738,0.491501985735445,
57.7933182191476));
#42108=CARTESIAN_POINT('Ctrl Pts',(-1.05932111294186,-0.0164551092965639,
57.8170935844447));
#42109=CARTESIAN_POINT('Ctrl Pts',(-0.922821481937435,-0.520415702512074,
57.8408689497419));
#42110=CARTESIAN_POINT('Ctrl Pts',(-0.562193425992196,-0.897981371030322,
57.864644315039));
#42111=CARTESIAN_POINT('Ctrl Pts',(-0.0650237641719233,-1.05745160694911,
57.8884196803362));
#42112=CARTESIAN_POINT('Ctrl Pts',(0.447938414546611,-0.960095395114365,
57.9121950456334));
#42113=CARTESIAN_POINT('Ctrl Pts',(0.852108445175959,-0.629557931096218,
57.9359704109305));
#42114=CARTESIAN_POINT('Ctrl Pts',(1.04932433848386,-0.146117841524369,
57.9597457762276));
#42115=CARTESIAN_POINT('Ctrl Pts',(0.991687678140017,0.372810327072094,
57.9835211415248));
#42116=CARTESIAN_POINT('Ctrl Pts',(0.693196852949359,0.80119293182569,58.007296506822));
#42117=CARTESIAN_POINT('Ctrl Pts',(0.226347226119961,1.03498740290602,58.0310718721191));
#42118=CARTESIAN_POINT('Ctrl Pts',(-0.295476031333513,1.01741137493825,
58.0548472374163));
#42119=CARTESIAN_POINT('Ctrl Pts',(-0.745536137617694,0.752733590623157,
58.0786226027134));
#42120=CARTESIAN_POINT('Ctrl Pts',(-1.01452564299876,0.305237138376526,
58.1023979680106));
#42121=CARTESIAN_POINT('Ctrl Pts',(-1.03711425841572,-0.216393174423657,
58.1261733333077));
#42122=CARTESIAN_POINT('Ctrl Pts',(-0.807815818999105,-0.685467427031471,
58.1499486986049));
#42123=CARTESIAN_POINT('Ctrl Pts',(-0.382320725410081,-0.988060146887956,
58.173724063902));
#42124=CARTESIAN_POINT('Ctrl Pts',(0.136029751029905,-1.05067973130782,
58.1974994291992));
#42125=CARTESIAN_POINT('Ctrl Pts',(0.62134227328246,-0.858117573749964,
58.2212747944964));
#42126=CARTESIAN_POINT('Ctrl Pts',(0.955747531469626,-0.457141823765944,
58.2450501597935));
#42127=CARTESIAN_POINT('Ctrl Pts',(1.05802751617526,0.0548613339460823,
58.2688255250907));
#42128=CARTESIAN_POINT('Ctrl Pts',(0.903341180323916,0.553540154710871,
58.2926008903878));
#42129=CARTESIAN_POINT('Ctrl Pts',(0.5292576588922,0.917779015586153,58.316376255685));
#42130=CARTESIAN_POINT('Ctrl Pts',(0.0266317402610465,1.05911413046801,
58.3401516209821));
#42131=CARTESIAN_POINT('Ctrl Pts',(-0.482462309113668,0.94321901551604,
58.3639269862793));
#42132=CARTESIAN_POINT('Ctrl Pts',(-0.874379288435858,0.598241465380611,
58.3877023515764));
#42133=CARTESIAN_POINT('Ctrl Pts',(-1.05393314384533,0.107967213776402,
58.4114777168736));
#42134=CARTESIAN_POINT('Ctrl Pts',(-0.977515091202718,-0.408529359308828,
58.4352530821707));
#42135=CARTESIAN_POINT('Ctrl Pts',(-0.66368501246902,-0.825805179912512,
58.4590284474679));
#42136=CARTESIAN_POINT('Ctrl Pts',(-0.188663761430564,-1.0425152162291,
58.482803812765));
#42137=CARTESIAN_POINT('Ctrl Pts',(0.33217882398349,-1.00602645086662,58.5065791780622));
#42138=CARTESIAN_POINT('Ctrl Pts',(0.772344140743365,-0.725201019859825,
58.5303545433593));
#42139=CARTESIAN_POINT('Ctrl Pts',(1.02492791636524,-0.268243839074722,
58.5541299086565));
#42140=CARTESIAN_POINT('Ctrl Pts',(1.02858437064807,0.253862528556006,58.5779052739536));
#42141=CARTESIAN_POINT('Ctrl Pts',(0.782425449558309,0.714312541419944,
58.6016806392508));
#42142=CARTESIAN_POINT('Ctrl Pts',(0.346236509580231,1.00127532196696,58.625456004548));
#42143=CARTESIAN_POINT('Ctrl Pts',(-0.174043931374068,1.04505535781517,
58.6492313698451));
#42144=CARTESIAN_POINT('Ctrl Pts',(-0.652053799988115,0.83501966016819,
58.6730067351423));
#42145=CARTESIAN_POINT('Ctrl Pts',(-0.97169740380609,0.422180229739439,
58.6967821004394));
#42146=CARTESIAN_POINT('Ctrl Pts',(-1.05534194074397,-0.0931953810716716,
58.7205574657366));
#42147=CARTESIAN_POINT('Ctrl Pts',(-0.882672410895779,-0.585936349776809,
58.7443328310337));
#42148=CARTESIAN_POINT('Ctrl Pts',(-0.495625581575281,-0.936369197397321,
58.7681081963309));
#42149=CARTESIAN_POINT('Ctrl Pts',(0.0117953213153582,-1.05938324573377,
58.7918835616281));
#42150=CARTESIAN_POINT('Ctrl Pts',(0.516351459091809,-0.925101703403523,
58.8156589269252));
#42151=CARTESIAN_POINT('Ctrl Pts',(0.895499767177114,-0.566137931896525,
58.8394342922223));
#42152=CARTESIAN_POINT('Ctrl Pts',(1.05715535724409,-0.0696745405184991,
58.8632096575195));
#42153=CARTESIAN_POINT('Ctrl Pts',(0.962056450613156,0.443710915777326,
58.8869850228166));
#42154=CARTESIAN_POINT('Ctrl Pts',(0.633300004359957,0.84933096930703,58.9107603881138));
#42155=CARTESIAN_POINT('Ctrl Pts',(0.150732083980457,1.04867145942151,58.934535753411));
#42156=CARTESIAN_POINT('Ctrl Pts',(-0.368444590347487,0.993317962582985,
58.9583111187081));
#42157=CARTESIAN_POINT('Ctrl Pts',(-0.798136020423016,0.696714348818546,
58.9820864840053));
#42158=CARTESIAN_POINT('Ctrl Pts',(-1.03398175807884,0.230897628629093,
59.0058618493024));
#42159=CARTESIAN_POINT('Ctrl Pts',(-1.01870124066612,-0.290997892108609,
59.0296372145996));
#42160=CARTESIAN_POINT('Ctrl Pts',(-0.756005693342733,-0.742217880800317,
59.0534125798968));
#42161=CARTESIAN_POINT('Ctrl Pts',(-0.3096967726728,-1.01317318358827,59.0771879451939));
#42162=CARTESIAN_POINT('Ctrl Pts',(0.211829133326388,-1.03805607229115,
59.1009633104911));
#42163=CARTESIAN_POINT('Ctrl Pts',(0.681907461502236,-0.810823164995865,
59.1247386757882));
#42164=CARTESIAN_POINT('Ctrl Pts',(0.986368876446939,-0.386663200373609,
59.1485140410854));
#42165=CARTESIAN_POINT('Ctrl Pts',(1.0512679198866,0.131406817036291,59.1722894063825));
#42166=CARTESIAN_POINT('Ctrl Pts',(0.860842366221901,0.617561666122401,
59.1960647716797));
#42167=CARTESIAN_POINT('Ctrl Pts',(0.461341441599518,0.953727458558869,
59.2198401369768));
#42168=CARTESIAN_POINT('Ctrl Pts',(-0.0502068645469796,1.05825859868873,
59.243615502274));
#42169=CARTESIAN_POINT('Ctrl Pts',(-0.549561278709315,0.905767294557619,
59.2673908675711));
#42170=CARTESIAN_POINT('Ctrl Pts',(-0.91544209454521,0.533289567195347,
59.2911662328683));
#42171=CARTESIAN_POINT('Ctrl Pts',(-1.05898673942326,0.0312902009549694,
59.3149415981654));
#42172=CARTESIAN_POINT('Ctrl Pts',(-0.945332094305355,-0.478308710369975,
59.3387169634626));
#42173=CARTESIAN_POINT('Ctrl Pts',(-0.602081804228732,-0.871739348642251,
59.3624923287598));
#42174=CARTESIAN_POINT('Ctrl Pts',(-0.112602098016971,-1.05344803311272,
59.3862676940569));
#42175=CARTESIAN_POINT('Ctrl Pts',(0.404225617853905,-0.979302629822281,
59.4100430593541));
#42176=CARTESIAN_POINT('Ctrl Pts',(0.822877844024298,-0.667311055587846,
59.4338184246512));
#42177=CARTESIAN_POINT('Ctrl Pts',(1.04167525640482,-0.193247641021974,
59.4575937899483));
#42178=CARTESIAN_POINT('Ctrl Pts',(1.00747787145168,0.327750408428632,59.4813691552455));
#42179=CARTESIAN_POINT('Ctrl Pts',(0.728591308296158,0.769146732015046,
59.5051445205427));
#42180=CARTESIAN_POINT('Ctrl Pts',(0.272749589451039,1.02373807828526,59.5289198858398));
#42181=CARTESIAN_POINT('Ctrl Pts',(-0.24933564917612,1.02969108371093,59.552695251137));
#42182=CARTESIAN_POINT('Ctrl Pts',(-0.710863972995126,0.785559920997844,
59.5764706164341));
#42183=CARTESIAN_POINT('Ctrl Pts',(-0.999742664943908,0.350637465297931,
59.6002459817313));
#42184=CARTESIAN_POINT('Ctrl Pts',(-1.04581077501601,-0.169445374199638,
59.6240213470285));
#42185=CARTESIAN_POINT('Ctrl Pts',(-0.837879849628336,-0.648374486381346,
59.6477967123256));
#42186=CARTESIAN_POINT('Ctrl Pts',(-0.426450165346835,-0.969830983982369,
59.6715720776227));
#42187=CARTESIAN_POINT('Ctrl Pts',(0.0885519692748135,-1.0557416239719,
59.6953474429199));
#42188=CARTESIAN_POINT('Ctrl Pts',(0.582048910852398,-0.885241334592178,
59.7191228082171));
#42189=CARTESIAN_POINT('Ctrl Pts',(0.93417826195316,-0.499739406633171,
59.7428981735142));
#42190=CARTESIAN_POINT('Ctrl Pts',(1.05942882546267,0.00713467400835743,
59.7666735388114));
#42191=CARTESIAN_POINT('Ctrl Pts',(0.927356096326115,0.51227749022626,59.7904489041085));
#42192=CARTESIAN_POINT('Ctrl Pts',(0.570091202696139,0.892995264566529,
59.8142242694056));
#42193=CARTESIAN_POINT('Ctrl Pts',(0.0742928706965789,1.05682828433461,
59.8379996347028));
#42194=CARTESIAN_POINT('Ctrl Pts',(-0.268131168947707,0.994883332089929,
59.8538498782343));
#42195=CARTESIAN_POINT('Ctrl Pts',(-0.421648628688828,0.924896675066913,
59.861775));
#42196=CARTESIAN_POINT('Ctrl Pts',(-0.462516886549903,0.969001292713887,
55.9956683941778));
#42197=CARTESIAN_POINT('Ctrl Pts',(-0.623354979013081,0.892231184847107,
56.0035935159435));
#42198=CARTESIAN_POINT('Ctrl Pts',(-0.905886993282922,0.657089893788024,
56.0194437594749));
#42199=CARTESIAN_POINT('Ctrl Pts',(-1.10974830284028,0.144570643569252,
56.0432191247721));
#42200=CARTESIAN_POINT('Ctrl Pts',(-1.04403145517334,-0.403001487158792,
56.0669944900692));
#42201=CARTESIAN_POINT('Ctrl Pts',(-0.72476766861592,-0.85273039506803,
56.0907698553664));
#42202=CARTESIAN_POINT('Ctrl Pts',(-0.22946735313918,-1.09533959234472,
56.1145452206636));
#42203=CARTESIAN_POINT('Ctrl Pts',(0.321559887535626,-1.07192747985427,
56.1383205859607));
#42204=CARTESIAN_POINT('Ctrl Pts',(0.79449103411378,-0.788169904962737,
56.1620959512579));
#42205=CARTESIAN_POINT('Ctrl Pts',(1.07446078004833,-0.312988648099244,
56.185871316555));
#42206=CARTESIAN_POINT('Ctrl Pts',(1.09347346420912,0.238209798475307,56.2096466818521));
#42207=CARTESIAN_POINT('Ctrl Pts',(0.846910753226789,0.731553191720428,
56.2334220471493));
#42208=CARTESIAN_POINT('Ctrl Pts',(0.39465638183097,1.04722221433094,56.2571974124465));
#42209=CARTESIAN_POINT('Ctrl Pts',(-0.153449415725439,1.10854916276288,
56.2809727777436));
#42210=CARTESIAN_POINT('Ctrl Pts',(-0.664286471749138,0.900639478939484,
56.3047481430408));
#42211=CARTESIAN_POINT('Ctrl Pts',(-1.01378628701798,0.473988764855061,
56.328523508338));
#42212=CARTESIAN_POINT('Ctrl Pts',(-1.11706477739624,-0.0677810171740453,
56.3522988736351));
#42213=CARTESIAN_POINT('Ctrl Pts',(-0.949038392374679,-0.593088623218428,
56.3760742389323));
#42214=CARTESIAN_POINT('Ctrl Pts',(-0.550516201657841,-0.974351012546832,
56.3998496042294));
#42215=CARTESIAN_POINT('Ctrl Pts',(-0.0182884880645982,-1.11896984576603,
56.4236249695266));
#42216=CARTESIAN_POINT('Ctrl Pts',(0.518381005763089,-0.991821111482199,
56.4474003348237));
#42217=CARTESIAN_POINT('Ctrl Pts',(0.929149747706489,-0.623785805144751,
56.4711757001208));
#42218=CARTESIAN_POINT('Ctrl Pts',(1.11425309984053,-0.104249766750074,
56.494951065418));
#42219=CARTESIAN_POINT('Ctrl Pts',(1.02873445502263,0.44060572556903,56.5187264307152));
#42220=CARTESIAN_POINT('Ctrl Pts',(0.693363983399069,0.878449982009057,
56.5425017960123));
#42221=CARTESIAN_POINT('Ctrl Pts',(0.189594118657963,1.10294245295529,56.5662771613095));
#42222=CARTESIAN_POINT('Ctrl Pts',(-0.360223039110721,1.05955997775346,
56.5900525266066));
#42223=CARTESIAN_POINT('Ctrl Pts',(-0.822551745469627,0.758838988447034,
56.6138278919038));
#42224=CARTESIAN_POINT('Ctrl Pts',(-1.08510483893557,0.273816494903183,
56.637603257201));
#42225=CARTESIAN_POINT('Ctrl Pts',(-1.08411526114131,-0.277708633144708,
56.6613786224981));
#42226=CARTESIAN_POINT('Ctrl Pts',(-0.819823353817542,-0.761785831384277,
56.6851539877952));
#42227=CARTESIAN_POINT('Ctrl Pts',(-0.356418486276366,-1.06084581679102,
56.7089293530924));
#42228=CARTESIAN_POINT('Ctrl Pts',(0.193550809502023,-1.10225499250565,
56.7327047183896));
#42229=CARTESIAN_POINT('Ctrl Pts',(0.696511838861817,-0.875956187653155,
56.7564800836867));
#42230=CARTESIAN_POINT('Ctrl Pts',(1.03030894599802,-0.436911272638936,
56.7802554489839));
#42231=CARTESIAN_POINT('Ctrl Pts',(1.11387182496675,0.108247595390182,56.804030814281));
#42232=CARTESIAN_POINT('Ctrl Pts',(0.926905308378269,0.62711604481364,56.8278061795782));
#42233=CARTESIAN_POINT('Ctrl Pts',(0.514818515655831,0.99367493693886,56.8515815448753));
#42234=CARTESIAN_POINT('Ctrl Pts',(-0.0223037961813828,1.11889701270422,
56.8753569101725));
#42235=CARTESIAN_POINT('Ctrl Pts',(-0.554009118052303,0.972369210473793,
56.8991322754696));
#42236=CARTESIAN_POINT('Ctrl Pts',(-0.951160581498487,0.589679177660173,
56.9229076407668));
#42237=CARTESIAN_POINT('Ctrl Pts',(-1.11730081777918,0.0637719919126017,
56.946683006064));
#42238=CARTESIAN_POINT('Ctrl Pts',(-1.01207884871958,-0.47762368904501,
56.9704583713611));
#42239=CARTESIAN_POINT('Ctrl Pts',(-0.66105024997122,-0.903017470138595,
56.9942337366583));
#42240=CARTESIAN_POINT('Ctrl Pts',(-0.149470391599245,-1.10909268611676,
57.0180091019554));
#42241=CARTESIAN_POINT('Ctrl Pts',(0.398411789703155,-1.04579923034397,
57.0417844672526));
#42242=CARTESIAN_POINT('Ctrl Pts',(0.849530503041471,-0.728509374520757,
57.0655598325497));
#42243=CARTESIAN_POINT('Ctrl Pts',(1.0943211916072,-0.234284258886341,57.0893351978469));
#42244=CARTESIAN_POINT('Ctrl Pts',(1.07333080565855,0.316842178358381,57.113110563144));
#42245=CARTESIAN_POINT('Ctrl Pts',(0.791657343273874,0.791016204134322,
57.1368859284412));
#42246=CARTESIAN_POINT('Ctrl Pts',(0.317711684246903,1.07307374865641,57.1606612937383));
#42247=CARTESIAN_POINT('Ctrl Pts',(-0.233397565755486,1.09451064894862,
57.1844366590355));
#42248=CARTESIAN_POINT('Ctrl Pts',(-0.727820847971375,0.850120460652928,
57.2082120243326));
#42249=CARTESIAN_POINT('Ctrl Pts',(-1.04547609488705,0.399258962807661,
57.2319873896298));
#42250=CARTESIAN_POINT('Ctrl Pts',(-1.10921342263122,-0.148571758478,57.255762754927));
#42251=CARTESIAN_POINT('Ctrl Pts',(-0.903552754984561,-0.660318410558366,
57.2795381202241));
#42252=CARTESIAN_POINT('Ctrl Pts',(-0.478443515984253,-1.01169154705135,
57.3033134855213));
#42253=CARTESIAN_POINT('Ctrl Pts',(0.0628667367111055,-1.11735211897495,
57.3270888508185));
#42254=CARTESIAN_POINT('Ctrl Pts',(0.588908356246074,-0.951638025882776,
57.3508642161155));
#42255=CARTESIAN_POINT('Ctrl Pts',(0.971920034559035,-0.554796747273525,
57.3746395814127));
#42256=CARTESIAN_POINT('Ctrl Pts',(1.11887857499228,-0.0232103163649987,
57.3984149467099));
#42257=CARTESIAN_POINT('Ctrl Pts',(0.994091715452223,0.514013273789476,
57.4221903120071));
#42258=CARTESIAN_POINT('Ctrl Pts',(0.627866815303003,0.926396916339742,
57.4459656773042));
#42259=CARTESIAN_POINT('Ctrl Pts',(0.10915001597191,1.11378375745737,57.4697410426014));
#42260=CARTESIAN_POINT('Ctrl Pts',(-0.436076375561883,1.03066259223828,
57.4935164078985));
#42261=CARTESIAN_POINT('Ctrl Pts',(-0.875391588041422,0.697221307727207,
57.5172917731957));
#42262=CARTESIAN_POINT('Ctrl Pts',(-1.10209781636267,0.194443790158363,
57.5410671384928));
#42263=CARTESIAN_POINT('Ctrl Pts',(-1.0611342379587,-0.355558874723069,
57.56484250379));
#42264=CARTESIAN_POINT('Ctrl Pts',(-0.762449800147398,-0.819205887807036,
57.5886178690872));
#42265=CARTESIAN_POINT('Ctrl Pts',(-0.278586889415522,-1.08388990649803,
57.6123932343843));
#42266=CARTESIAN_POINT('Ctrl Pts',(0.272937255862792,-1.08532632821866,
57.6361685996814));
#42267=CARTESIAN_POINT('Ctrl Pts',(0.758172310063855,-0.823166284911474,
57.6599439649786));
#42268=CARTESIAN_POINT('Ctrl Pts',(1.05926777820804,-0.361081373671809,
57.6837193302757));
#42269=CARTESIAN_POINT('Ctrl Pts',(1.10309569963031,0.188700455271399,57.7074946955729));
#42270=CARTESIAN_POINT('Ctrl Pts',(0.879011455421081,0.692652037895677,
57.7312700608701));
#42271=CARTESIAN_POINT('Ctrl Pts',(0.441439058991073,1.02837713974961,57.7550454261672));
#42272=CARTESIAN_POINT('Ctrl Pts',(-0.103346967524035,1.11433719702167,
57.7788207914643));
#42273=CARTESIAN_POINT('Ctrl Pts',(-0.623032805641989,0.929654832427817,
57.8025961567615));
#42274=CARTESIAN_POINT('Ctrl Pts',(-0.991400795023013,0.519184406536112,
57.8263715220587));
#42275=CARTESIAN_POINT('Ctrl Pts',(-1.11898429572149,-0.0173818955010686,
57.8501468873558));
#42276=CARTESIAN_POINT('Ctrl Pts',(-0.97479671973563,-0.549726604372732,
57.873922252653));
#42277=CARTESIAN_POINT('Ctrl Pts',(-0.59385733670132,-0.948557561779218,
57.8976976179501));
#42278=CARTESIAN_POINT('Ctrl Pts',(-0.0686860386979539,-1.1170094952374,
57.9214729832473));
#42279=CARTESIAN_POINT('Ctrl Pts',(0.473167243817168,-1.01416997773597,
57.9452483485444));
#42280=CARTESIAN_POINT('Ctrl Pts',(0.900100976705333,-0.665015951761027,
57.9690237138416));
#42281=CARTESIAN_POINT('Ctrl Pts',(1.10842448199767,-0.154347504258106,
57.9927990791387));
#42282=CARTESIAN_POINT('Ctrl Pts',(1.04754160428037,0.393807785174727,58.0165744444359));
#42283=CARTESIAN_POINT('Ctrl Pts',(0.73223915092162,0.84631779505107,58.040349809733));
#42284=CARTESIAN_POINT('Ctrl Pts',(0.239095575755094,1.09328006019357,58.0641251750302));
#42285=CARTESIAN_POINT('Ctrl Pts',(-0.31211786000007,1.07471411353508,58.0879005403274));
#42286=CARTESIAN_POINT('Ctrl Pts',(-0.787526293675256,0.795129122301928,
58.1116759056246));
#42287=CARTESIAN_POINT('Ctrl Pts',(-1.07166585113145,0.322428733026724,
58.1354512709217));
#42288=CARTESIAN_POINT('Ctrl Pts',(-1.09552670465818,-0.228580891028345,
58.1592266362188));
#42289=CARTESIAN_POINT('Ctrl Pts',(-0.853313697095174,-0.724074387554404,
58.1830020015159));
#42290=CARTESIAN_POINT('Ctrl Pts',(-0.403853829057226,-1.04370976287392,
58.2067773668132));
#42291=CARTESIAN_POINT('Ctrl Pts',(0.143691231387472,-1.10985621338301,
58.2305527321103));
#42292=CARTESIAN_POINT('Ctrl Pts',(0.656337570899634,-0.906448551980799,
58.2543280974075));
#42293=CARTESIAN_POINT('Ctrl Pts',(1.00957723330847,-0.482889008311166,
58.2781034627046));
#42294=CARTESIAN_POINT('Ctrl Pts',(1.11761784087684,0.0579512391266419,
58.3018788280018));
#42295=CARTESIAN_POINT('Ctrl Pts',(0.954219246753043,0.584716695065718,
58.3256541932989));
#42296=CARTESIAN_POINT('Ctrl Pts',(0.559066558246913,0.969470251122989,
58.3494295585961));
#42297=CARTESIAN_POINT('Ctrl Pts',(0.0281316956263525,1.11876565556139,
58.3732049238932));
#42298=CARTESIAN_POINT('Ctrl Pts',(-0.509635596402341,0.99634308510781,
58.3969802891904));
#42299=CARTESIAN_POINT('Ctrl Pts',(-0.923626160481851,0.631935677135001,
58.4207556544875));
#42300=CARTESIAN_POINT('Ctrl Pts',(-1.11329286492568,0.114048153286674,
58.4445310197847));
#42301=CARTESIAN_POINT('Ctrl Pts',(-1.03257078757632,-0.431538588085164,
58.4683063850818));
#42302=CARTESIAN_POINT('Ctrl Pts',(-0.701065141802112,-0.872316256476116,
58.492081750379));
#42303=CARTESIAN_POINT('Ctrl Pts',(-0.199289699443702,-1.10123185572256,
58.5158571156762));
#42304=CARTESIAN_POINT('Ctrl Pts',(0.350887830769737,-1.06268796670529,
58.5396324809733));
#42305=CARTESIAN_POINT('Ctrl Pts',(0.815844179659772,-0.766045859513509,
58.5634078462705));
#42306=CARTESIAN_POINT('Ctrl Pts',(1.08265400231119,-0.283351893662422,
58.5871832115676));
#42307=CARTESIAN_POINT('Ctrl Pts',(1.08651639575406,0.268160597627874,58.6109585768647));
#42308=CARTESIAN_POINT('Ctrl Pts',(0.826493288892493,0.754544119172755,
58.6347339421619));
#42309=CARTESIAN_POINT('Ctrl Pts',(0.365737274649193,1.05766924427947,58.6585093074591));
#42310=CARTESIAN_POINT('Ctrl Pts',(-0.183846449951664,1.10391506340057,
58.6822846727562));
#42311=CARTESIAN_POINT('Ctrl Pts',(-0.688778835084223,0.882049715550399,
58.7060600380533));
#42312=CARTESIAN_POINT('Ctrl Pts',(-1.02642543584613,0.445958304116661,
58.7298354033505));
#42313=CARTESIAN_POINT('Ctrl Pts',(-1.11478100821498,-0.098444340039033,
58.7536107686477));
#42314=CARTESIAN_POINT('Ctrl Pts',(-0.932386368960449,-0.618937511659511,
58.7773861339448));
#42315=CARTESIAN_POINT('Ctrl Pts',(-0.523540251926434,-0.989107470892482,
58.8011614992419));
#42316=CARTESIAN_POINT('Ctrl Pts',(0.0124596585054514,-1.11904992796231,
58.8249368645392));
#42317=CARTESIAN_POINT('Ctrl Pts',(0.545433454254506,-0.977205368048354,
58.8487122298363));
#42318=CARTESIAN_POINT('Ctrl Pts',(0.945936188801736,-0.598024005436041,
58.8724875951334));
#42319=CARTESIAN_POINT('Ctrl Pts',(1.11669656012879,-0.073598756504813,
58.8962629604306));
#42320=CARTESIAN_POINT('Ctrl Pts',(1.01624148398594,0.468701643466889,58.9200383257278));
#42321=CARTESIAN_POINT('Ctrl Pts',(0.668968786425046,0.897167067580795,
58.9438136910249));
#42322=CARTESIAN_POINT('Ctrl Pts',(0.15922163050928,1.10773483141972,58.9675890563221));
#42323=CARTESIAN_POINT('Ctrl Pts',(-0.389196161018078,1.04926370975618,
58.9913644216192));
#42324=CARTESIAN_POINT('Ctrl Pts',(-0.843088711998524,0.735954759522071,
59.0151397869164));
#42325=CARTESIAN_POINT('Ctrl Pts',(-1.0922177753444,0.243902266459851,59.0389151522135));
#42326=CARTESIAN_POINT('Ctrl Pts',(-1.07607662720109,-0.307387502598993,
59.0626905175107));
#42327=CARTESIAN_POINT('Ctrl Pts',(-0.798585516696848,-0.784021145687122,
59.0864658828079));
#42328=CARTESIAN_POINT('Ctrl Pts',(-0.327139543262851,-1.07023721837558,
59.110241248105));
#42329=CARTESIAN_POINT('Ctrl Pts',(0.223759793581615,-1.09652156346277,
59.1340166134021));
#42330=CARTESIAN_POINT('Ctrl Pts',(0.720313917313741,-0.856490423114379,
59.1577919786993));
#42331=CARTESIAN_POINT('Ctrl Pts',(1.04192323654097,-0.408440881301712,
59.1815673439965));
#42332=CARTESIAN_POINT('Ctrl Pts',(1.11047752997392,0.138807924073182,59.2053427092936));
#42333=CARTESIAN_POINT('Ctrl Pts',(0.909326810469135,0.652344032029584,
59.2291180745908));
#42334=CARTESIAN_POINT('Ctrl Pts',(0.487325157413065,1.00744338566233,59.2528934398879));
#42335=CARTESIAN_POINT('Ctrl Pts',(-0.0530346202668054,1.11786193844124,
59.2766688051851));
#42336=CARTESIAN_POINT('Ctrl Pts',(-0.580513720437941,0.956782004819481,
59.3004441704822));
#42337=CARTESIAN_POINT('Ctrl Pts',(-0.967001709796653,0.563325552066532,
59.3242195357794));
#42338=CARTESIAN_POINT('Ctrl Pts',(-1.11863108958631,0.0330525305790881,
59.3479949010765));
#42339=CARTESIAN_POINT('Ctrl Pts',(-0.99857517691829,-0.505248058281805,
59.3717702663737));
#42340=CARTESIAN_POINT('Ctrl Pts',(-0.635992311906835,-0.920837533752328,
59.3955456316709));
#42341=CARTESIAN_POINT('Ctrl Pts',(-0.118944083910845,-1.11278043174102,
59.419320996968));
#42342=CARTESIAN_POINT('Ctrl Pts',(0.426992450901576,-1.03445900411316,
59.4430963622652));
#42343=CARTESIAN_POINT('Ctrl Pts',(0.869224046902271,-0.704895411260545,
59.4668717275623));
#42344=CARTESIAN_POINT('Ctrl Pts',(1.10034458760252,-0.204131752730095,
59.4906470928595));
#42345=CARTESIAN_POINT('Ctrl Pts',(1.06422113433627,0.3462099975799,59.5144224581566));
#42346=CARTESIAN_POINT('Ctrl Pts',(0.769627096092177,0.812466686178068,
59.5381978234538));
#42347=CARTESIAN_POINT('Ctrl Pts',(0.288111417332764,1.0813971500596,59.5619731887509));
#42348=CARTESIAN_POINT('Ctrl Pts',(-0.263378754924248,1.08768544121352,
59.5857485540481));
#42349=CARTESIAN_POINT('Ctrl Pts',(-0.750901320154641,0.82980430032555,
59.6095239193452));
#42350=CARTESIAN_POINT('Ctrl Pts',(-1.05605026480425,0.370386101406355,
59.6332992846424));
#42351=CARTESIAN_POINT('Ctrl Pts',(-1.10471302727964,-0.178988892410047,
59.6570746499396));
#42352=CARTESIAN_POINT('Ctrl Pts',(-0.885070996868774,-0.684892294832443,
59.6808500152367));
#42353=CARTESIAN_POINT('Ctrl Pts',(-0.450468731436616,-1.02445389535057,
59.7046253805338));
#42354=CARTESIAN_POINT('Ctrl Pts',(0.0935394015687504,-1.11520320243905,
59.728400745831));
#42355=CARTESIAN_POINT('Ctrl Pts',(0.614831124036485,-0.935099979817495,
59.7521761111282));
#42356=CARTESIAN_POINT('Ctrl Pts',(0.986793137377364,-0.527885776223916,
59.7759514764253));
#42357=CARTESIAN_POINT('Ctrl Pts',(1.11909807483697,0.00753651378501131,
59.7997268417225));
#42358=CARTESIAN_POINT('Ctrl Pts',(0.979586733099938,0.541130030933556,
59.8235022070196));
#42359=CARTESIAN_POINT('Ctrl Pts',(0.602199932723299,0.943290627360923,
59.8472775723168));
#42360=CARTESIAN_POINT('Ctrl Pts',(0.07847720070704,1.11635106578832,59.8710529376139));
#42361=CARTESIAN_POINT('Ctrl Pts',(-0.283232877717969,1.05091724415087,
59.8869031811454));
#42362=CARTESIAN_POINT('Ctrl Pts',(-0.44539676218196,0.976988792086596,
59.8948283029111));
#42363=CARTESIAN_POINT('Ctrl Pts',(-0.487177848858668,1.02066752383254,
56.0287216970889));
#42364=CARTESIAN_POINT('Ctrl Pts',(-0.656591676070983,0.939804106528635,
56.0366468188546));
#42365=CARTESIAN_POINT('Ctrl Pts',(-0.954188029735873,0.692125304549036,
56.052497062386));
#42366=CARTESIAN_POINT('Ctrl Pts',(-1.16891903122754,0.152279013351406,
56.0762724276832));
#42367=CARTESIAN_POINT('Ctrl Pts',(-1.09969822348802,-0.424489144743217,
56.1000477929803));
#42368=CARTESIAN_POINT('Ctrl Pts',(-0.763411594228405,-0.898197172052492,
56.1238231582775));
#42369=CARTESIAN_POINT('Ctrl Pts',(-0.241702335063995,-1.15374206193584,
56.1475985235747));
#42370=CARTESIAN_POINT('Ctrl Pts',(0.338705156167176,-1.12908163778266,
56.1713738888718));
#42371=CARTESIAN_POINT('Ctrl Pts',(0.836852543534731,-0.830194377764544,
56.195149254169));
#42372=CARTESIAN_POINT('Ctrl Pts',(1.1317500111436,-0.329676906362474,56.2189246194661));
#42373=CARTESIAN_POINT('Ctrl Pts',(1.1517764336156,0.250910919304856,56.2426999847633));
#42374=CARTESIAN_POINT('Ctrl Pts',(0.892067232420471,0.770558914997795,
56.2664753500605));
#42375=CARTESIAN_POINT('Ctrl Pts',(0.415699086303556,1.10305911090171,56.2902507153576));
#42376=CARTESIAN_POINT('Ctrl Pts',(-0.161631193229248,1.167655954137,56.3140260806548));
#42377=CARTESIAN_POINT('Ctrl Pts',(-0.699705597230648,0.948660722897936,
56.3378014459519));
#42378=CARTESIAN_POINT('Ctrl Pts',(-1.06784041161392,0.499261396849246,
56.3615768112491));
#42379=CARTESIAN_POINT('Ctrl Pts',(-1.17662561327687,-0.0713950368096213,
56.3853521765462));
#42380=CARTESIAN_POINT('Ctrl Pts',(-0.999640220555501,-0.62471154685274,
56.4091275418434));
#42381=CARTESIAN_POINT('Ctrl Pts',(-0.579869204097866,-1.02630248565988,
56.4329029071405));
#42382=CARTESIAN_POINT('Ctrl Pts',(-0.0192636129259017,-1.17863225808771,
56.4566782724377));
#42383=CARTESIAN_POINT('Ctrl Pts',(0.546020589995489,-1.04470407372333,
56.4804536377348));
#42384=CARTESIAN_POINT('Ctrl Pts',(0.978691132191524,-0.657045473443933,
56.5042290030319));
#42385=CARTESIAN_POINT('Ctrl Pts',(1.17366401973703,-0.109808265570952,
56.5280043683291));
#42386=CARTESIAN_POINT('Ctrl Pts',(1.08358560177813,0.464098405527887,56.5517797336263));
#42387=CARTESIAN_POINT('Ctrl Pts',(0.730333494260416,0.925288103008396,
56.5755550989234));
#42388=CARTESIAN_POINT('Ctrl Pts',(0.199703097486968,1.16175029987297,56.5993304642206));
#42389=CARTESIAN_POINT('Ctrl Pts',(-0.379429790363681,1.11605471218396,
56.6231058295178));
#42390=CARTESIAN_POINT('Ctrl Pts',(-0.866409425441811,0.799299564561584,
56.6468811948149));
#42391=CARTESIAN_POINT('Ctrl Pts',(-1.14296160116897,0.288416131060683,
56.6706565601121));
#42392=CARTESIAN_POINT('Ctrl Pts',(-1.14191926002402,-0.292515794426723,
56.6944319254092));
#42393=CARTESIAN_POINT('Ctrl Pts',(-0.863535558531093,-0.802403530373075,
56.7182072907064));
#42394=CARTESIAN_POINT('Ctrl Pts',(-0.375422382375764,-1.11740911094109,
56.7419826560035));
#42395=CARTESIAN_POINT('Ctrl Pts',(0.203870755339166,-1.1610261846833,56.7657580213007));
#42396=CARTESIAN_POINT('Ctrl Pts',(0.733649190394879,-0.92266134189949,
56.7895333865978));
#42397=CARTESIAN_POINT('Ctrl Pts',(1.08524404312101,-0.460206967866842,
56.813308751895));
#42398=CARTESIAN_POINT('Ctrl Pts',(1.17326241564812,0.114019254647519,56.8370841171921));
#42399=CARTESIAN_POINT('Ctrl Pts',(0.976327021484194,0.660553278337659,
56.8608594824893));
#42400=CARTESIAN_POINT('Ctrl Pts',(0.542268151290001,1.04665674339745,56.8846348477864));
#42401=CARTESIAN_POINT('Ctrl Pts',(-0.0234930134682861,1.17855554163603,
56.9084102130836));
#42402=CARTESIAN_POINT('Ctrl Pts',(-0.583548359486088,1.02421501577741,
56.9321855783807));
#42403=CARTESIAN_POINT('Ctrl Pts',(-1.00187556279331,0.62112031288665,56.9559609436779));
#42404=CARTESIAN_POINT('Ctrl Pts',(-1.17687423910946,0.067172254118474,
56.979736308975));
#42405=CARTESIAN_POINT('Ctrl Pts',(-1.06604193432269,-0.503090131754104,
57.0035116742722));
#42406=CARTESIAN_POINT('Ctrl Pts',(-0.69629682317279,-0.951165506335416,
57.0272870395694));
#42407=CARTESIAN_POINT('Ctrl Pts',(-0.157440011305465,-1.1682284576413,
57.0510624048665));
#42408=CARTESIAN_POINT('Ctrl Pts',(0.419654728966468,-1.10156025475636,
57.0748377701637));
#42409=CARTESIAN_POINT('Ctrl Pts',(0.894826664813918,-0.767352804348056,
57.0986131354608));
#42410=CARTESIAN_POINT('Ctrl Pts',(1.1526693610356,-0.246776073663168,57.122388500758));
#42411=CARTESIAN_POINT('Ctrl Pts',(1.13055978758964,0.333735903205072,57.1461638660551));
#42412=CARTESIAN_POINT('Ctrl Pts',(0.833867762983234,0.833192438912023,
57.1699392313523));
#42413=CARTESIAN_POINT('Ctrl Pts',(0.334651770324009,1.13028902455161,57.1937145966494));
#42414=CARTESIAN_POINT('Ctrl Pts',(-0.245842102894417,1.15286892006302,
57.2174899619466));
#42415=CARTESIAN_POINT('Ctrl Pts',(-0.766627566215206,0.895448078406435,
57.2412653272437));
#42416=CARTESIAN_POINT('Ctrl Pts',(-1.10121989002294,0.420547072538497,
57.2650406925409));
#42417=CARTESIAN_POINT('Ctrl Pts',(-1.16835563171236,-0.156493463917345,
57.288816057838));
#42418=CARTESIAN_POINT('Ctrl Pts',(-0.951729332062369,-0.695525962775614,
57.3125914231352));
#42419=CARTESIAN_POINT('Ctrl Pts',(-0.50395367108924,-1.06563398209634,
57.3363667884324));
#42420=CARTESIAN_POINT('Ctrl Pts',(0.0662187315670568,-1.1769282756364,
57.3601421537296));
#42421=CARTESIAN_POINT('Ctrl Pts',(0.620308392004842,-1.00237846405995,
57.3839175190267));
#42422=CARTESIAN_POINT('Ctrl Pts',(1.02374189022832,-0.584377984351374,
57.4076928843239));
#42423=CARTESIAN_POINT('Ctrl Pts',(1.17853612084276,-0.0244478684494714,
57.431468249621));
#42424=CARTESIAN_POINT('Ctrl Pts',(1.04709574414639,0.541419974690026,57.4552436149181));
#42425=CARTESIAN_POINT('Ctrl Pts',(0.661344079198414,0.975791522463701,
57.4790189802153));
#42426=CARTESIAN_POINT('Ctrl Pts',(0.114969791439926,1.17316965246254,57.5027943455124));
#42427=CARTESIAN_POINT('Ctrl Pts',(-0.459327554868421,1.08561654544384,
57.5265697108096));
#42428=CARTESIAN_POINT('Ctrl Pts',(-0.922066638371227,0.734396487468189,
57.5503450761068));
#42429=CARTESIAN_POINT('Ctrl Pts',(-1.16086062805725,0.204811348878305,
57.5741204414039));
#42430=CARTESIAN_POINT('Ctrl Pts',(-1.11771291045225,-0.374516937148636,
57.5978958067011));
#42431=CARTESIAN_POINT('Ctrl Pts',(-0.80310290132176,-0.862885169817746,
57.6216711719983));
#42432=CARTESIAN_POINT('Ctrl Pts',(-0.293440878490046,-1.14168188968461,
57.6454465372954));
#42433=CARTESIAN_POINT('Ctrl Pts',(0.28749001182744,-1.14319490005085,57.6692219025925));
#42434=CARTESIAN_POINT('Ctrl Pts',(0.798597339518466,-0.867056731544629,
57.6929972678897));
#42435=CARTESIAN_POINT('Ctrl Pts',(1.11574693283554,-0.380333890510585,
57.7167726331868));
#42436=CARTESIAN_POINT('Ctrl Pts',(1.16191171751556,0.198761784815075,57.740547998484));
#42437=CARTESIAN_POINT('Ctrl Pts',(0.925879513650944,0.72958358849711,57.7643233637812));
#42438=CARTESIAN_POINT('Ctrl Pts',(0.464976171498692,1.08320923479319,57.7880987290783));
#42439=CARTESIAN_POINT('Ctrl Pts',(-0.108857329945276,1.17375260090021,
57.8118740943755));
#42440=CARTESIAN_POINT('Ctrl Pts',(-0.656252324720897,0.979223147551796,
57.8356494596726));
#42441=CARTESIAN_POINT('Ctrl Pts',(-1.04426134638865,0.54686682733678,57.8594248249698));
#42442=CARTESIAN_POINT('Ctrl Pts',(-1.17864747850111,-0.0183086817055737,
57.8832001902669));
#42443=CARTESIAN_POINT('Ctrl Pts',(-1.02677195753382,-0.579037506233389,
57.9069755555641));
#42444=CARTESIAN_POINT('Ctrl Pts',(-0.625521247410444,-0.999133752528114,
57.9307509208612));
#42445=CARTESIAN_POINT('Ctrl Pts',(-0.0723483132239842,-1.17656738352568,
57.9545262861584));
#42446=CARTESIAN_POINT('Ctrl Pts',(0.498396073087726,-1.06824456035758,
57.9783016514556));
#42447=CARTESIAN_POINT('Ctrl Pts',(0.948093508234708,-0.700473972425836,
58.0020770167527));
#42448=CARTESIAN_POINT('Ctrl Pts',(1.16752462551148,-0.162577166991841,
58.0258523820499));
#42449=CARTESIAN_POINT('Ctrl Pts',(1.10339553042073,0.414805243277359,58.049627747347));
#42450=CARTESIAN_POINT('Ctrl Pts',(0.771281448893881,0.89144265827645,58.0734031126442));
#42451=CARTESIAN_POINT('Ctrl Pts',(0.251843925390228,1.15157271748113,58.0971784779413));
#42452=CARTESIAN_POINT('Ctrl Pts',(-0.328759688666628,1.13201685213191,
58.1209538432385));
#42453=CARTESIAN_POINT('Ctrl Pts',(-0.829516449732817,0.837524653980699,
58.1447292085356));
#42454=CARTESIAN_POINT('Ctrl Pts',(-1.12880605926414,0.339620327676922,
58.1685045738328));
#42455=CARTESIAN_POINT('Ctrl Pts',(-1.15393915090063,-0.240768607633033,
58.1922799391299));
#42456=CARTESIAN_POINT('Ctrl Pts',(-0.898811575191243,-0.762681348077337,
58.2160553044271));
#42457=CARTESIAN_POINT('Ctrl Pts',(-0.42538693270437,-1.09935937885989,
58.2398306697243));
#42458=CARTESIAN_POINT('Ctrl Pts',(0.151352711745039,-1.16903269545819,
58.2636060350214));
#42459=CARTESIAN_POINT('Ctrl Pts',(0.691332868516809,-0.954779530211634,
58.2873814003186));
#42460=CARTESIAN_POINT('Ctrl Pts',(1.06340693514731,-0.508636192856387,
58.3111567656157));
#42461=CARTESIAN_POINT('Ctrl Pts',(1.17720816557841,0.0610411443072006,
58.3349321309129));
#42462=CARTESIAN_POINT('Ctrl Pts',(1.00509731318217,0.615893235420565,58.35870749621));
#42463=CARTESIAN_POINT('Ctrl Pts',(0.588875457601626,1.02116148665983,58.3824828615072));
#42464=CARTESIAN_POINT('Ctrl Pts',(0.029631650991658,1.17841718065477,58.4062582268043));
#42465=CARTESIAN_POINT('Ctrl Pts',(-0.536808883691014,1.04946715469958,
58.4300335921015));
#42466=CARTESIAN_POINT('Ctrl Pts',(-0.972873032527844,0.66562988888939,
58.4538089573986));
#42467=CARTESIAN_POINT('Ctrl Pts',(-1.17265258600602,0.120129092796946,
58.4775843226958));
#42468=CARTESIAN_POINT('Ctrl Pts',(-1.08762648394992,-0.4545478168615,58.5013596879929));
#42469=CARTESIAN_POINT('Ctrl Pts',(-0.738445271135204,-0.918827333039719,
58.5251350532901));
#42470=CARTESIAN_POINT('Ctrl Pts',(-0.20991563745684,-1.15994849521602,
58.5489104185873));
#42471=CARTESIAN_POINT('Ctrl Pts',(0.369596837555985,-1.11934948254397,
58.5726857838844));
#42472=CARTESIAN_POINT('Ctrl Pts',(0.859344218576179,-0.806890699167193,
58.5964611491816));
#42473=CARTESIAN_POINT('Ctrl Pts',(1.14038008825714,-0.298459948250121,
58.6202365144787));
#42474=CARTESIAN_POINT('Ctrl Pts',(1.14444842086004,0.282458666699742,58.6440118797758));
#42475=CARTESIAN_POINT('Ctrl Pts',(0.870561128226679,0.794775696925566,
58.6677872450731));
#42476=CARTESIAN_POINT('Ctrl Pts',(0.385238039718154,1.11406316659198,58.6915626103702));
#42477=CARTESIAN_POINT('Ctrl Pts',(-0.193648968529259,1.16277476898597,
58.7153379756674));
#42478=CARTESIAN_POINT('Ctrl Pts',(-0.72550387018033,0.929079770932609,
58.7391133409644));
#42479=CARTESIAN_POINT('Ctrl Pts',(-1.08115346788616,0.469736378493884,
58.7628887062617));
#42480=CARTESIAN_POINT('Ctrl Pts',(-1.17422007568598,-0.103693299006395,
58.7866640715588));
#42481=CARTESIAN_POINT('Ctrl Pts',(-0.98210032702512,-0.651938673542211,
58.810439436856));
#42482=CARTESIAN_POINT('Ctrl Pts',(-0.551454922277587,-1.04184574438764,
58.8342148021531));
#42483=CARTESIAN_POINT('Ctrl Pts',(0.0131239956955444,-1.17871661019085,
58.8579901674503));
#42484=CARTESIAN_POINT('Ctrl Pts',(0.574515449417203,-1.02930903269318,
58.8817655327474));
#42485=CARTESIAN_POINT('Ctrl Pts',(0.996372610426357,-0.629910078975558,
58.9055408980446));
#42486=CARTESIAN_POINT('Ctrl Pts',(1.17623776301348,-0.0775229724911266,
58.9293162633417));
#42487=CARTESIAN_POINT('Ctrl Pts',(1.07042651735873,0.493692371156451,58.9530916286389));
#42488=CARTESIAN_POINT('Ctrl Pts',(0.704637568490134,0.945003165854559,
58.976866993936));
#42489=CARTESIAN_POINT('Ctrl Pts',(0.167711177038103,1.16679820341794,59.0006423592332));
#42490=CARTESIAN_POINT('Ctrl Pts',(-0.40994773168867,1.10520945692938,59.0244177245303));
#42491=CARTESIAN_POINT('Ctrl Pts',(-0.888041403574033,0.775195170225595,
59.0481930898275));
#42492=CARTESIAN_POINT('Ctrl Pts',(-1.15045379260996,0.25690690429061,59.0719684551246));
#42493=CARTESIAN_POINT('Ctrl Pts',(-1.13345201373606,-0.323777113089378,
59.0957438204218));
#42494=CARTESIAN_POINT('Ctrl Pts',(-0.841165340050963,-0.825824410573927,
59.119519185719));
#42495=CARTESIAN_POINT('Ctrl Pts',(-0.344582313852902,-1.12730125316288,
59.1432945510161));
#42496=CARTESIAN_POINT('Ctrl Pts',(0.235690453836842,-1.15498705463438,
59.1670699163133));
#42497=CARTESIAN_POINT('Ctrl Pts',(0.758720373125246,-0.902157681232892,
59.1908452816104));
#42498=CARTESIAN_POINT('Ctrl Pts',(1.09747759663501,-0.430218562229815,
59.2146206469076));
#42499=CARTESIAN_POINT('Ctrl Pts',(1.16968714006124,0.146209031110073,59.2383960122047));
#42500=CARTESIAN_POINT('Ctrl Pts',(0.957811254716368,0.687126397936767,
59.2621713775019));
#42501=CARTESIAN_POINT('Ctrl Pts',(0.513308873226614,1.0611593127658,59.285946742799));
#42502=CARTESIAN_POINT('Ctrl Pts',(-0.0558623759866322,1.17746527819375,
59.3097221080962));
#42503=CARTESIAN_POINT('Ctrl Pts',(-0.611466162166566,1.00779671508134,
59.3334974733933));
#42504=CARTESIAN_POINT('Ctrl Pts',(-1.0185613250481,0.593361536937717,59.3572728386905));
#42505=CARTESIAN_POINT('Ctrl Pts',(-1.17827543974936,0.0348148602032075,
59.3810482039876));
#42506=CARTESIAN_POINT('Ctrl Pts',(-1.05181825953123,-0.532187406193635,
59.4048235692848));
#42507=CARTESIAN_POINT('Ctrl Pts',(-0.669902819584936,-0.969935718862406,
59.428598934582));
#42508=CARTESIAN_POINT('Ctrl Pts',(-0.125286069804721,-1.17211283036932,
59.4523742998791));
#42509=CARTESIAN_POINT('Ctrl Pts',(0.449759283949248,-1.08961537840405,
59.4761496651763));
#42510=CARTESIAN_POINT('Ctrl Pts',(0.915570249780245,-0.742479766933245,
59.4999250304734));
#42511=CARTESIAN_POINT('Ctrl Pts',(1.15901391880021,-0.215015864438216,
59.5237003957705));
#42512=CARTESIAN_POINT('Ctrl Pts',(1.12096439722085,0.364669586731168,59.5474757610677));
#42513=CARTESIAN_POINT('Ctrl Pts',(0.810662883888195,0.855786640341092,
59.5712511263649));
#42514=CARTESIAN_POINT('Ctrl Pts',(0.303473245214488,1.13905622183395,59.5950264916621));
#42515=CARTESIAN_POINT('Ctrl Pts',(-0.277421860672377,1.14567979871612,
59.6188018569592));
#42516=CARTESIAN_POINT('Ctrl Pts',(-0.790938667314156,0.874048679653256,
59.6425772222563));
#42517=CARTESIAN_POINT('Ctrl Pts',(-1.11235786466458,0.39013473751478,59.6663525875535));
#42518=CARTESIAN_POINT('Ctrl Pts',(-1.16361527954326,-0.188532410620455,
59.6901279528507));
#42519=CARTESIAN_POINT('Ctrl Pts',(-0.932262144109214,-0.721410103283539,
59.7139033181478));
#42520=CARTESIAN_POINT('Ctrl Pts',(-0.474487297526397,-1.07907680671876,
59.737678683445));
#42521=CARTESIAN_POINT('Ctrl Pts',(0.0985268338626855,-1.1746647809062,
59.7614540487421));
#42522=CARTESIAN_POINT('Ctrl Pts',(0.647613337220575,-0.984958625042814,
59.7852294140393));
#42523=CARTESIAN_POINT('Ctrl Pts',(1.03940801280157,-0.556032145814661,
59.8090047793364));
#42524=CARTESIAN_POINT('Ctrl Pts',(1.17876732421126,0.00793835356166478,
59.8327801446336));
#42525=CARTESIAN_POINT('Ctrl Pts',(1.03181736987376,0.569982571640854,59.8565555099308));
#42526=CARTESIAN_POINT('Ctrl Pts',(0.634308662750459,0.993585990155316,
59.8803308752279));
#42527=CARTESIAN_POINT('Ctrl Pts',(0.0826615307175012,1.17587384724203,
59.9041062405251));
#42528=CARTESIAN_POINT('Ctrl Pts',(-0.298334586488231,1.10695115621182,
59.9199564840565));
#42529=CARTESIAN_POINT('Ctrl Pts',(-0.469144895675092,1.02908090910628,
59.9278816058222));
#42530=CARTESIAN_POINT('Ctrl Pts',(-0.511838811167433,1.07233375495119,
56.061775));
#42531=CARTESIAN_POINT('Ctrl Pts',(-0.689828373128885,0.987377028210164,
56.0697001217657));
#42532=CARTESIAN_POINT('Ctrl Pts',(-1.00248906618882,0.727160715310048,
56.0855503652972));
#42533=CARTESIAN_POINT('Ctrl Pts',(-1.22808975961479,0.159987383133561,
56.1093257305943));
#42534=CARTESIAN_POINT('Ctrl Pts',(-1.15536499180269,-0.445976802327642,
56.1331010958914));
#42535=CARTESIAN_POINT('Ctrl Pts',(-0.802055519840889,-0.943663949036954,
56.1568764611886));
#42536=CARTESIAN_POINT('Ctrl Pts',(-0.25393731698881,-1.21214453152697,
56.1806518264858));
#42537=CARTESIAN_POINT('Ctrl Pts',(0.355850424798725,-1.18623579571104,
56.2044271917829));
#42538=CARTESIAN_POINT('Ctrl Pts',(0.879214052955683,-0.87221885056635,
56.2282025570801));
#42539=CARTESIAN_POINT('Ctrl Pts',(1.18903924223887,-0.346365164625703,
56.2519779223772));
#42540=CARTESIAN_POINT('Ctrl Pts',(1.21007940302208,0.263612040134405,56.2757532876744));
#42541=CARTESIAN_POINT('Ctrl Pts',(0.937223711614153,0.809564638275162,
56.2995286529715));
#42542=CARTESIAN_POINT('Ctrl Pts',(0.436741790776142,1.15889600747247,56.3233040182687));
#42543=CARTESIAN_POINT('Ctrl Pts',(-0.169812970733057,1.22676274551112,
56.3470793835658));
#42544=CARTESIAN_POINT('Ctrl Pts',(-0.735124722712158,0.996681966856387,
56.370854748863));
#42545=CARTESIAN_POINT('Ctrl Pts',(-1.12189453620986,0.524534028843431,
56.3946301141602));
#42546=CARTESIAN_POINT('Ctrl Pts',(-1.23618644915751,-0.0750090564451986,
56.4184054794573));
#42547=CARTESIAN_POINT('Ctrl Pts',(-1.05024204873632,-0.656334470487052,
56.4421808447545));
#42548=CARTESIAN_POINT('Ctrl Pts',(-0.60922220653789,-1.07825395877292,
56.4659562100516));
#42549=CARTESIAN_POINT('Ctrl Pts',(-0.0202387377872045,-1.2382946704094,
56.4897315753488));
#42550=CARTESIAN_POINT('Ctrl Pts',(0.573660174227889,-1.09758703596446,
56.513506940646));
#42551=CARTESIAN_POINT('Ctrl Pts',(1.02823251667656,-0.690305141743117,
56.5372823059431));
#42552=CARTESIAN_POINT('Ctrl Pts',(1.23307493963353,-0.115366764391829,
56.5610576712402));
#42553=CARTESIAN_POINT('Ctrl Pts',(1.13843674853363,0.487591085486743,56.5848330365374));
#42554=CARTESIAN_POINT('Ctrl Pts',(0.767303005121764,0.972126224007736,
56.6086084018345));
#42555=CARTESIAN_POINT('Ctrl Pts',(0.209812076315972,1.22055814679065,56.6323837671317));
#42556=CARTESIAN_POINT('Ctrl Pts',(-0.398636541616641,1.17254944661446,
56.6561591324289));
#42557=CARTESIAN_POINT('Ctrl Pts',(-0.910267105413995,0.839760140676135,
56.679934497726));
#42558=CARTESIAN_POINT('Ctrl Pts',(-1.20081836340238,0.303015767218183,
56.7037098630232));
#42559=CARTESIAN_POINT('Ctrl Pts',(-1.19972325890673,-0.307322955708736,
56.7274852283203));
#42560=CARTESIAN_POINT('Ctrl Pts',(-0.907247763244644,-0.843021229361873,
56.7512605936174));
#42561=CARTESIAN_POINT('Ctrl Pts',(-0.394426278475162,-1.17397240509116,
56.7750359589146));
#42562=CARTESIAN_POINT('Ctrl Pts',(0.21419070117631,-1.21979737686095,56.7988113242118));
#42563=CARTESIAN_POINT('Ctrl Pts',(0.770786541927939,-0.969366496145824,
56.8225866895089));
#42564=CARTESIAN_POINT('Ctrl Pts',(1.140179140244,-0.483502663094748,56.8463620548061));
#42565=CARTESIAN_POINT('Ctrl Pts',(1.23265300632948,0.119790913904855,56.8701374201032));
#42566=CARTESIAN_POINT('Ctrl Pts',(1.02574873459012,0.693990511861678,56.8939127854004));
#42567=CARTESIAN_POINT('Ctrl Pts',(0.569717786924172,1.09963854985604,56.9176881506976));
#42568=CARTESIAN_POINT('Ctrl Pts',(-0.0246822307551888,1.23821407056785,
56.9414635159947));
#42569=CARTESIAN_POINT('Ctrl Pts',(-0.613087600919873,1.07606082108103,
56.9652388812919));
#42570=CARTESIAN_POINT('Ctrl Pts',(-1.05259054408814,0.652561448113126,
56.989014246589));
#42571=CARTESIAN_POINT('Ctrl Pts',(-1.23644766043974,0.0705725163243472,
57.0127896118862));
#42572=CARTESIAN_POINT('Ctrl Pts',(-1.1200050199258,-0.528556574463199,
57.0365649771833));
#42573=CARTESIAN_POINT('Ctrl Pts',(-0.73154339637436,-0.999313542532237,
57.0603403424805));
#42574=CARTESIAN_POINT('Ctrl Pts',(-0.165409631011685,-1.22736422916583,
57.0841157077776));
#42575=CARTESIAN_POINT('Ctrl Pts',(0.440897668229782,-1.15732127916876,
57.1078910730748));
#42576=CARTESIAN_POINT('Ctrl Pts',(0.940122826586366,-0.806196234175355,
57.1316664383719));
#42577=CARTESIAN_POINT('Ctrl Pts',(1.211017530464,-0.259267888439993,57.1554418036691));
#42578=CARTESIAN_POINT('Ctrl Pts',(1.18778876952072,0.350629628051763,57.1792171689663));
#42579=CARTESIAN_POINT('Ctrl Pts',(0.876078182692593,0.875368673689724,
57.2029925342634));
#42580=CARTESIAN_POINT('Ctrl Pts',(0.351591856401113,1.18750430044682,57.2267678995605));
#42581=CARTESIAN_POINT('Ctrl Pts',(-0.258286640033346,1.21122719117742,
57.2505432648577));
#42582=CARTESIAN_POINT('Ctrl Pts',(-0.805434284459037,0.940775696159941,
57.2743186301548));
#42583=CARTESIAN_POINT('Ctrl Pts',(-1.15696368515882,0.441835182269334,
57.298093995452));
#42584=CARTESIAN_POINT('Ctrl Pts',(-1.22749784079349,-0.16441516935669,
57.3218693607492));
#42585=CARTESIAN_POINT('Ctrl Pts',(-0.999905909140176,-0.73073351499286,
57.3456447260463));
#42586=CARTESIAN_POINT('Ctrl Pts',(-0.529463826194227,-1.11957641714134,
57.3694200913435));
#42587=CARTESIAN_POINT('Ctrl Pts',(0.0695707264230086,-1.23650443229785,
57.3931954566407));
#42588=CARTESIAN_POINT('Ctrl Pts',(0.651708427763611,-1.05311890223713,
57.4169708219377));
#42589=CARTESIAN_POINT('Ctrl Pts',(1.0755637458976,-0.613959221429223,57.440746187235));
#42590=CARTESIAN_POINT('Ctrl Pts',(1.23819366669324,-0.0256854205339441,
57.4645215525321));
#42591=CARTESIAN_POINT('Ctrl Pts',(1.10009977284055,0.568826675590577,57.4882969178293));
#42592=CARTESIAN_POINT('Ctrl Pts',(0.694821343093825,1.02518612858766,57.5120722831264));
#42593=CARTESIAN_POINT('Ctrl Pts',(0.120789566907943,1.23255554746772,57.5358476484236));
#42594=CARTESIAN_POINT('Ctrl Pts',(-0.482578734174961,1.14057049864941,
57.5596230137207));
#42595=CARTESIAN_POINT('Ctrl Pts',(-0.96874168870103,0.771571667209171,
57.5833983790179));
#42596=CARTESIAN_POINT('Ctrl Pts',(-1.21962343975183,0.215178907598248,
57.607173744315));
#42597=CARTESIAN_POINT('Ctrl Pts',(-1.1742915829458,-0.393474999574203,
57.6309491096122));
#42598=CARTESIAN_POINT('Ctrl Pts',(-0.843756002496121,-0.906564451828457,
57.6547244749094));
#42599=CARTESIAN_POINT('Ctrl Pts',(-0.308294867564569,-1.19947387287119,
57.6784998402065));
#42600=CARTESIAN_POINT('Ctrl Pts',(0.302042767792087,-1.20106347188305,
57.7022752055036));
#42601=CARTESIAN_POINT('Ctrl Pts',(0.839022368973077,-0.910947178177785,
57.7260505708008));
#42602=CARTESIAN_POINT('Ctrl Pts',(1.17222608746303,-0.399586407349361,
57.7498259360979));
#42603=CARTESIAN_POINT('Ctrl Pts',(1.2207277354008,0.208823114358751,57.7736013013951));
#42604=CARTESIAN_POINT('Ctrl Pts',(0.972747571880807,0.766515139098543,
57.7973766666923));
#42605=CARTESIAN_POINT('Ctrl Pts',(0.488513284006311,1.13804132983677,57.8211520319894));
#42606=CARTESIAN_POINT('Ctrl Pts',(-0.114367692366517,1.23316800477876,
57.8449273972866));
#42607=CARTESIAN_POINT('Ctrl Pts',(-0.689471843799805,1.02879146267578,
57.8687027625837));
#42608=CARTESIAN_POINT('Ctrl Pts',(-1.09712189775428,0.574549248137447,
57.8924781278809));
#42609=CARTESIAN_POINT('Ctrl Pts',(-1.23831066128074,-0.0192354679100782,
57.916253493178));
#42610=CARTESIAN_POINT('Ctrl Pts',(-1.07874719533202,-0.608348408094048,
57.9400288584752));
#42611=CARTESIAN_POINT('Ctrl Pts',(-0.657185158119568,-1.04970994327701,
57.9638042237723));
#42612=CARTESIAN_POINT('Ctrl Pts',(-0.0760105877500149,-1.23612527181397,
57.9875795890695));
#42613=CARTESIAN_POINT('Ctrl Pts',(0.523624902358283,-1.12231914297919,
58.0113549543667));
#42614=CARTESIAN_POINT('Ctrl Pts',(0.996086039764082,-0.735931993090646,
58.0351303196638));
#42615=CARTESIAN_POINT('Ctrl Pts',(1.22662476902529,-0.170806829725578,
58.058905684961));
#42616=CARTESIAN_POINT('Ctrl Pts',(1.15924945656108,0.435802701379992,58.0826810502581));
#42617=CARTESIAN_POINT('Ctrl Pts',(0.810323746866142,0.936567521501829,
58.1064564155553));
#42618=CARTESIAN_POINT('Ctrl Pts',(0.26459227502536,1.20986537476868,58.1302317808524));
#42619=CARTESIAN_POINT('Ctrl Pts',(-0.345401517333186,1.18931959072875,
58.1540071461496));
#42620=CARTESIAN_POINT('Ctrl Pts',(-0.871506605790379,0.87992018565947,
58.1777825114468));
#42621=CARTESIAN_POINT('Ctrl Pts',(-1.18594626739684,0.35681192232712,58.2015578767439));
#42622=CARTESIAN_POINT('Ctrl Pts',(-1.21235159714309,-0.252956324237721,
58.2253332420411));
#42623=CARTESIAN_POINT('Ctrl Pts',(-0.944309453287311,-0.80128830860027,
58.2491086073382));
#42624=CARTESIAN_POINT('Ctrl Pts',(-0.446920036351515,-1.15500899484585,
58.2728839726354));
#42625=CARTESIAN_POINT('Ctrl Pts',(0.159014192102606,-1.22820917753338,
58.2966593379325));
#42626=CARTESIAN_POINT('Ctrl Pts',(0.726328166133983,-1.00311050844247,
58.3204347032297));
#42627=CARTESIAN_POINT('Ctrl Pts',(1.11723663698614,-0.534383377401609,
58.3442100685268));
#42628=CARTESIAN_POINT('Ctrl Pts',(1.23679849027999,0.0641310494877601,
58.367985433824));
#42629=CARTESIAN_POINT('Ctrl Pts',(1.0559753796113,0.647069775775413,58.3917607991211));
#42630=CARTESIAN_POINT('Ctrl Pts',(0.618684356956339,1.07285272219666,58.4155361644183));
#42631=CARTESIAN_POINT('Ctrl Pts',(0.0311316063569641,1.23806870574815,
58.4393115297154));
#42632=CARTESIAN_POINT('Ctrl Pts',(-0.563982170979687,1.10259122429135,
58.4630868950126));
#42633=CARTESIAN_POINT('Ctrl Pts',(-1.02211990457384,0.69932410064378,58.4868622603097));
#42634=CARTESIAN_POINT('Ctrl Pts',(-1.23201230708637,0.126210032307217,
58.5106376256069));
#42635=CARTESIAN_POINT('Ctrl Pts',(-1.14268218032353,-0.477557045637837,
58.534412990904));
#42636=CARTESIAN_POINT('Ctrl Pts',(-0.775825400468297,-0.965338409603322,
58.5581883562012));
#42637=CARTESIAN_POINT('Ctrl Pts',(-0.220541575469977,-1.21866513470948,
58.5819637214983));
#42638=CARTESIAN_POINT('Ctrl Pts',(0.388305844342232,-1.17601099838264,
58.6057390867956));
#42639=CARTESIAN_POINT('Ctrl Pts',(0.902844257492586,-0.847735538820877,
58.6295144520926));
#42640=CARTESIAN_POINT('Ctrl Pts',(1.19810617420309,-0.313568002837821,
58.6532898173898));
#42641=CARTESIAN_POINT('Ctrl Pts',(1.20238044596602,0.29675673577161,58.677065182687));
#42642=CARTESIAN_POINT('Ctrl Pts',(0.914628967560865,0.835007274678378,
58.7008405479842));
#42643=CARTESIAN_POINT('Ctrl Pts',(0.404738804787115,1.17045708890448,58.7246159132813));
#42644=CARTESIAN_POINT('Ctrl Pts',(-0.203451487106854,1.22163447457137,
58.7483912785784));
#42645=CARTESIAN_POINT('Ctrl Pts',(-0.762228905276438,0.976109826314818,
58.7721666438755));
#42646=CARTESIAN_POINT('Ctrl Pts',(-1.1358814999262,0.493514452871106,58.7959420091728));
#42647=CARTESIAN_POINT('Ctrl Pts',(-1.23365914315699,-0.108942257973756,
58.8197173744699));
#42648=CARTESIAN_POINT('Ctrl Pts',(-1.03181428508979,-0.684939835424913,
58.8434927397671));
#42649=CARTESIAN_POINT('Ctrl Pts',(-0.57936959262874,-1.09458401788281,
58.8672681050642));
#42650=CARTESIAN_POINT('Ctrl Pts',(0.0137883328856377,-1.23838329241939,
58.8910434703614));
#42651=CARTESIAN_POINT('Ctrl Pts',(0.6035974445799,-1.08141269733801,58.9148188356585));
#42652=CARTESIAN_POINT('Ctrl Pts',(1.04680903205098,-0.661796152515074,
58.9385942009557));
#42653=CARTESIAN_POINT('Ctrl Pts',(1.23577896589818,-0.0814471884774405,
58.9623695662528));
#42654=CARTESIAN_POINT('Ctrl Pts',(1.12461155073152,0.518683098846014,58.98614493155));
#42655=CARTESIAN_POINT('Ctrl Pts',(0.740306350555223,0.992839264128324,
59.0099202968471));
#42656=CARTESIAN_POINT('Ctrl Pts',(0.176200723566927,1.22586157541615,59.0336956621443));
#42657=CARTESIAN_POINT('Ctrl Pts',(-0.430699302359262,1.16115520410258,
59.0574710274414));
#42658=CARTESIAN_POINT('Ctrl Pts',(-0.932994095149541,0.81443558092912,
59.0812463927386));
#42659=CARTESIAN_POINT('Ctrl Pts',(-1.20868980987552,0.269911542121367,
59.1050217580358));
#42660=CARTESIAN_POINT('Ctrl Pts',(-1.19082740027104,-0.340166723579763,
59.1287971233329));
#42661=CARTESIAN_POINT('Ctrl Pts',(-0.883745163405079,-0.867627675460732,
59.1525724886301));
#42662=CARTESIAN_POINT('Ctrl Pts',(-0.362025084442952,-1.18436528795019,
59.1763478539272));
#42663=CARTESIAN_POINT('Ctrl Pts',(0.247621114092068,-1.213452545806,59.2001232192244));
#42664=CARTESIAN_POINT('Ctrl Pts',(0.797126828936751,-0.947824939351406,
59.2238985845215));
#42665=CARTESIAN_POINT('Ctrl Pts',(1.15303195672905,-0.451996243157917,
59.2476739498187));
#42666=CARTESIAN_POINT('Ctrl Pts',(1.22889675014856,0.153610138146963,59.2714493151158));
#42667=CARTESIAN_POINT('Ctrl Pts',(1.0062956989636,0.721908763843951,59.295224680413));
#42668=CARTESIAN_POINT('Ctrl Pts',(0.539292589040162,1.11487523986926,59.3190000457101));
#42669=CARTESIAN_POINT('Ctrl Pts',(-0.0586901317064581,1.23706861794625,
59.3427754110073));
#42670=CARTESIAN_POINT('Ctrl Pts',(-0.642418603895192,1.0588114253432,59.3665507763045));
#42671=CARTESIAN_POINT('Ctrl Pts',(-1.07012094029954,0.623397521808901,
59.3903261416016));
#42672=CARTESIAN_POINT('Ctrl Pts',(-1.2379197899124,0.0365771898273263,
59.4141015068987));
#42673=CARTESIAN_POINT('Ctrl Pts',(-1.10506134214416,-0.559126754105465,
59.4378768721959));
#42674=CARTESIAN_POINT('Ctrl Pts',(-0.703813327263037,-1.01903390397248,
59.4616522374931));
#42675=CARTESIAN_POINT('Ctrl Pts',(-0.131628055698595,-1.23144522899762,
59.4854276027902));
#42676=CARTESIAN_POINT('Ctrl Pts',(0.47252611699692,-1.14477175269494,59.5092029680874));
#42677=CARTESIAN_POINT('Ctrl Pts',(0.961916452658219,-0.780064122605945,
59.5329783333845));
#42678=CARTESIAN_POINT('Ctrl Pts',(1.2176832499979,-0.225899976146337,59.5567536986817));
#42679=CARTESIAN_POINT('Ctrl Pts',(1.17770766010544,0.383129175882436,59.5805290639788));
#42680=CARTESIAN_POINT('Ctrl Pts',(0.851698671684214,0.899106594504114,
59.604304429276));
#42681=CARTESIAN_POINT('Ctrl Pts',(0.318835073096213,1.1967152936083,59.6280797945732));
#42682=CARTESIAN_POINT('Ctrl Pts',(-0.291464966420505,1.20367415621872,
59.6518551598703));
#42683=CARTESIAN_POINT('Ctrl Pts',(-0.830976014473671,0.918293058980961,
59.6756305251674));
#42684=CARTESIAN_POINT('Ctrl Pts',(-1.16866546452492,0.409883373623204,
59.6994058904646));
#42685=CARTESIAN_POINT('Ctrl Pts',(-1.22251753180688,-0.198075928830864,
59.7231812557618));
#42686=CARTESIAN_POINT('Ctrl Pts',(-0.979453291349652,-0.757927911734636,
59.7469566210589));
#42687=CARTESIAN_POINT('Ctrl Pts',(-0.498505863616178,-1.13369971808696,
59.770731986356));
#42688=CARTESIAN_POINT('Ctrl Pts',(0.103514266156622,-1.23412635937334,
59.7945073516532));
#42689=CARTESIAN_POINT('Ctrl Pts',(0.680395550404662,-1.03481727026813,
59.8182827169504));
#42690=CARTESIAN_POINT('Ctrl Pts',(1.09202288822577,-0.584178515405407,
59.8420580822475));
#42691=CARTESIAN_POINT('Ctrl Pts',(1.23843657358556,0.00834019333831885,
59.8658334475447));
#42692=CARTESIAN_POINT('Ctrl Pts',(1.08404800664758,0.598835112348151,59.8896088128419));
#42693=CARTESIAN_POINT('Ctrl Pts',(0.666417392777619,1.04388135294971,59.913384178139));
#42694=CARTESIAN_POINT('Ctrl Pts',(0.0868458607279623,1.23539662869573,
59.9371595434362));
#42695=CARTESIAN_POINT('Ctrl Pts',(-0.313436295258493,1.16298506827277,
59.9530097869676));
#42696=CARTESIAN_POINT('Ctrl Pts',(-0.492893029168225,1.08117302612596,
59.9609349087333));
#42697=CARTESIAN_POINT('Ctrl Pts',(-1.1881744462934,-2.6792430042513E-5,
59.7155118763048));
#42698=CARTESIAN_POINT('Ctrl Pts',(-1.18822732035292,-0.0636541554091953,
59.7180683361238));
#42699=CARTESIAN_POINT('Ctrl Pts',(-1.18320405435424,-0.127273252397746,
59.7206247959428));
#42700=CARTESIAN_POINT('Ctrl Pts',(-1.17303148051702,-0.190058042239148,
59.7231812557618));
#42701=CARTESIAN_POINT('Ctrl Pts',(-1.14149611832114,-0.384693256465457,
59.7311063775275));
#42702=CARTESIAN_POINT('Ctrl Pts',(-1.06047470483539,-0.571310584100047,
59.7390314992932));
#42703=CARTESIAN_POINT('Ctrl Pts',(-0.939806093470275,-0.727247882309399,
59.7469566210589));
#42704=CARTESIAN_POINT('Ctrl Pts',(-0.819137482105158,-0.883185180518747,
59.7548817428246));
#42705=CARTESIAN_POINT('Ctrl Pts',(-0.658821672860672,-1.00844244930285,
59.7628068645903));
#42706=CARTESIAN_POINT('Ctrl Pts',(-0.478327079942962,-1.08780885724264,
59.770731986356));
#42707=CARTESIAN_POINT('Ctrl Pts',(-0.297832487025252,-1.16717526518242,
59.7786571081218));
#42708=CARTESIAN_POINT('Ctrl Pts',(-0.0971591104343092,-1.20065081227788,
59.7865822298875));
#42709=CARTESIAN_POINT('Ctrl Pts',(0.0993244585691621,-1.18417040430808,
59.7945073516532));
#42710=CARTESIAN_POINT('Ctrl Pts',(0.295808027572639,-1.16768999633827,
59.8024324734189));
#42711=CARTESIAN_POINT('Ctrl Pts',(0.488101788988651,-1.1012536333032,59.8103575951847));
#42712=CARTESIAN_POINT('Ctrl Pts',(0.652853226000178,-0.992928992641875,
59.8182827169504));
#42713=CARTESIAN_POINT('Ctrl Pts',(0.817604663011705,-0.88460435198055,
59.8262078387161));
#42714=CARTESIAN_POINT('Ctrl Pts',(0.954813775618739,-0.734391433692975,
59.8341329604818));
#42715=CARTESIAN_POINT('Ctrl Pts',(1.04782061281555,-0.56053185642523,59.8420580822475));
#42716=CARTESIAN_POINT('Ctrl Pts',(1.12495121150481,-0.416350055530902,
59.848630388165));
#42717=CARTESIAN_POINT('Ctrl Pts',(1.17168218150301,-0.255905525034767,
59.8552026940825));
#42718=CARTESIAN_POINT('Ctrl Pts',(1.18463057630128,-0.0928773270329352,
59.861775));
#42719=CARTESIAN_POINT('',(-0.590199102098993,-0.827621616530207,56.061775));
#42720=CARTESIAN_POINT('Ctrl Pts',(-0.590199102098968,-0.827621616530224,
56.061775));
#42721=CARTESIAN_POINT('Ctrl Pts',(-0.615134357767448,-0.812766705787686,
56.061775));
#42722=CARTESIAN_POINT('Ctrl Pts',(-0.639392267770691,-0.796859952851615,
56.061775));
#42723=CARTESIAN_POINT('Ctrl Pts',(-0.662901484824834,-0.779940878155282,
56.061775));
#42724=CARTESIAN_POINT('Ctrl Pts',(-0.698146337912065,-0.754575920204076,
56.061775));
#42725=CARTESIAN_POINT('Ctrl Pts',(-0.731709816296971,-0.726937622024356,
56.061775));
#42726=CARTESIAN_POINT('Ctrl Pts',(-0.763450748845136,-0.697254972180441,
56.061775));
#42727=CARTESIAN_POINT('Ctrl Pts',(-0.776265295565428,-0.685271401671611,
56.061775));
#42728=CARTESIAN_POINT('Ctrl Pts',(-0.788782535939489,-0.672954139864235,
56.061775));
#42729=CARTESIAN_POINT('Ctrl Pts',(-0.800992024443568,-0.660316467040226,
56.061775));
#42730=CARTESIAN_POINT('Ctrl Pts',(-0.808384981105688,-0.652664240866562,
56.061775));
#42731=CARTESIAN_POINT('Ctrl Pts',(-0.815659101518573,-0.644900665985542,
56.061775));
#42732=CARTESIAN_POINT('Ctrl Pts',(-0.822810165450187,-0.637031793761004,
56.061775));
#42733=CARTESIAN_POINT('Ctrl Pts',(-0.853515682503708,-0.603244123479613,
56.061775));
#42734=CARTESIAN_POINT('Ctrl Pts',(-0.881968856256046,-0.567503882812971,
56.061775));
#42735=CARTESIAN_POINT('Ctrl Pts',(-0.908008022156744,-0.530066595828932,
56.061775));
#42736=CARTESIAN_POINT('Ctrl Pts',(-0.924969563415267,-0.505680481073624,
56.061775));
#42737=CARTESIAN_POINT('Ctrl Pts',(-0.940906332635631,-0.480573325113094,
56.061775));
#42738=CARTESIAN_POINT('Ctrl Pts',(-0.955765822442545,-0.454806995938702,
56.061775));
#42739=CARTESIAN_POINT('Ctrl Pts',(-0.962684813681071,-0.442809477307636,
56.061775));
#42740=CARTESIAN_POINT('Ctrl Pts',(-0.969372662773929,-0.430663710074883,
56.061775));
#42741=CARTESIAN_POINT('Ctrl Pts',(-0.975808677947894,-0.418405110522661,
56.061775));
#42742=CARTESIAN_POINT('Ctrl Pts',(-0.981874487414775,-0.406851637262477,
56.061775));
#42743=CARTESIAN_POINT('Ctrl Pts',(-0.987719049555523,-0.39519409417799,
56.061775));
#42744=CARTESIAN_POINT('Ctrl Pts',(-0.993339017601775,-0.383438440842466,
56.061775));
#42745=CARTESIAN_POINT('Ctrl Pts',(-1.01324908218045,-0.341791261508261,
56.061775));
#42746=CARTESIAN_POINT('Ctrl Pts',(-1.03034352792734,-0.298915493303166,
56.061775));
#42747=CARTESIAN_POINT('Ctrl Pts',(-1.04462831590242,-0.255120180705625,
56.061775));
#42748=CARTESIAN_POINT('Ctrl Pts',(-1.05904170449985,-0.210930595230794,
56.061775));
#42749=CARTESIAN_POINT('Ctrl Pts',(-1.0705950057442,-0.165803798615469,
56.061775));
#42750=CARTESIAN_POINT('Ctrl Pts',(-1.07924869357493,-0.120029021709373,
56.061775));
#42751=CARTESIAN_POINT('Ctrl Pts',(-1.08423255818454,-0.0936662391480227,
56.061775));
#42752=CARTESIAN_POINT('Ctrl Pts',(-1.08825378413265,-0.0670880899307722,
56.061775));
#42753=CARTESIAN_POINT('Ctrl Pts',(-1.09129725999253,-0.0403477199554475,
56.061775));
#42754=CARTESIAN_POINT('Ctrl Pts',(-1.09228584736055,-0.0316618643118283,
56.061775));
#42755=CARTESIAN_POINT('Ctrl Pts',(-1.09317007591419,-0.0229689788750462,
56.061775));
#42756=CARTESIAN_POINT('Ctrl Pts',(-1.09394999532767,-0.014271318779927,
56.061775));
#42757=CARTESIAN_POINT('Ctrl Pts',(-1.09820214619636,0.0331486611431905,
56.061775));
#42758=CARTESIAN_POINT('Ctrl Pts',(-1.09935785012545,0.0807113437002552,
56.061775));
#42759=CARTESIAN_POINT('Ctrl Pts',(-1.09740239594642,0.128108944348922,
56.061775));
#42760=CARTESIAN_POINT('Ctrl Pts',(-1.0971991706204,0.133034855141317,56.061775));
#42761=CARTESIAN_POINT('Ctrl Pts',(-1.09696229903521,0.137959000314265,
56.061775));
#42762=CARTESIAN_POINT('Ctrl Pts',(-1.09669173443149,0.142881045058402,
56.061775));
#42763=CARTESIAN_POINT('Ctrl Pts',(-1.09412391271685,0.189594226312492,
56.061775));
#42764=CARTESIAN_POINT('Ctrl Pts',(-1.08852549990792,0.236117919595857,
56.061775));
#42765=CARTESIAN_POINT('Ctrl Pts',(-1.08001366796156,0.282192064001538,
56.061775));
#42766=CARTESIAN_POINT('Ctrl Pts',(-1.07595996531885,0.304134564994794,
56.061775));
#42767=CARTESIAN_POINT('Ctrl Pts',(-1.07124473547026,0.325975153615651,
56.061775));
#42768=CARTESIAN_POINT('Ctrl Pts',(-1.06587669291147,0.347685494908889,
56.061775));
#42769=CARTESIAN_POINT('Ctrl Pts',(-1.06298190770522,0.359393072505361,
56.061775));
#42770=CARTESIAN_POINT('Ctrl Pts',(-1.05989723894755,0.37106276652936,56.061775));
#42771=CARTESIAN_POINT('Ctrl Pts',(-1.05662375707351,0.3826900597016,56.061775));
#42772=CARTESIAN_POINT('Ctrl Pts',(-1.05399617734826,0.392023131022726,
56.061775));
#42773=CARTESIAN_POINT('Ctrl Pts',(-1.05124881344766,0.401321987665181,
56.061775));
#42774=CARTESIAN_POINT('Ctrl Pts',(-1.04838510858005,0.410577137809347,
56.061775));
#42775=CARTESIAN_POINT('Ctrl Pts',(-1.03397913167826,0.457135524711359,
56.061775));
#42776=CARTESIAN_POINT('Ctrl Pts',(-1.01661730418623,0.502644930856158,
56.061775));
#42777=CARTESIAN_POINT('Ctrl Pts',(-0.996446590099755,0.54682452658831,
56.061775));
#42778=CARTESIAN_POINT('Ctrl Pts',(-0.976533823419174,0.590439144201009,
56.061775));
#42779=CARTESIAN_POINT('Ctrl Pts',(-0.953883183691056,0.632758814049037,
56.061775));
#42780=CARTESIAN_POINT('Ctrl Pts',(-0.928586748315069,0.673506306109805,
56.061775));
#42781=CARTESIAN_POINT('Ctrl Pts',(-0.915799325391781,0.694104283899948,
56.061775));
#42782=CARTESIAN_POINT('Ctrl Pts',(-0.902335055056348,0.7143003027281,56.061775));
#42783=CARTESIAN_POINT('Ctrl Pts',(-0.888220713491049,0.734071072891337,
56.061775));
#42784=CARTESIAN_POINT('Ctrl Pts',(-0.879122478025178,0.746815494687745,
56.061775));
#42785=CARTESIAN_POINT('Ctrl Pts',(-0.869754065159863,0.759383184937614,
56.061775));
#42786=CARTESIAN_POINT('Ctrl Pts',(-0.860122058821546,0.771767493293035,
56.061775));
#42787=CARTESIAN_POINT('Ctrl Pts',(-0.854552989740373,0.778927898543135,
56.061775));
#42788=CARTESIAN_POINT('Ctrl Pts',(-0.848896461607506,0.786025972038092,
56.061775));
#42789=CARTESIAN_POINT('Ctrl Pts',(-0.843162068000595,0.793050710973022,
56.061775));
#42790=CARTESIAN_POINT('Ctrl Pts',(-0.811996437531328,0.831229188558734,
56.061775));
#42791=CARTESIAN_POINT('Ctrl Pts',(-0.778473601297604,0.867322786293068,
56.061775));
#42792=CARTESIAN_POINT('Ctrl Pts',(-0.742860732609996,0.901167302089467,
56.061775));
#42793=CARTESIAN_POINT('Ctrl Pts',(-0.706923922034914,0.935319674476243,
56.061775));
#42794=CARTESIAN_POINT('Ctrl Pts',(-0.668858204757825,0.967182723574884,
56.061775));
#42795=CARTESIAN_POINT('Ctrl Pts',(-0.628892453156465,0.996561433376393,
56.061775));
#42796=CARTESIAN_POINT('Ctrl Pts',(-0.591486565579768,1.02405839444809,
56.061775));
#42797=CARTESIAN_POINT('Ctrl Pts',(-0.552415331592047,1.04937941259432,
56.061775));
#42798=CARTESIAN_POINT('Ctrl Pts',(-0.511838811167469,1.07233375495117,
56.061775));
#42799=CARTESIAN_POINT('Ctrl Pts',(-0.590199102098993,-0.827621616530207,
56.061775));
#42800=CARTESIAN_POINT('Ctrl Pts',(-0.476210674841661,-0.908735228656824,
56.0683473059175));
#42801=CARTESIAN_POINT('Ctrl Pts',(-0.187550710949804,-1.03567600475847,
56.0828447336007));
#42802=CARTESIAN_POINT('Ctrl Pts',(0.304414618904077,-1.01477332192588,
56.1052672830496));
#42803=CARTESIAN_POINT('Ctrl Pts',(0.752129524692829,-0.746145432160931,
56.1290426483468));
#42804=CARTESIAN_POINT('Ctrl Pts',(1.01717154895307,-0.296300389836015,
56.1528180136439));
#42805=CARTESIAN_POINT('Ctrl Pts',(1.03517049480264,0.225508677645759,56.1765933789411));
#42806=CARTESIAN_POINT('Ctrl Pts',(0.801754274033107,0.69254746844306,56.2003687442382));
#42807=CARTESIAN_POINT('Ctrl Pts',(0.373613677358384,0.991385317760177,
56.2241441095354));
#42808=CARTESIAN_POINT('Ctrl Pts',(-0.14526763822163,1.04944237138876,56.2479194748325));
#42809=CARTESIAN_POINT('Ctrl Pts',(-0.628867346267627,0.852618234981034,
56.2716948401297));
#42810=CARTESIAN_POINT('Ctrl Pts',(-0.946309424739493,0.465101894360692,
56.2945056710427));
#42811=CARTESIAN_POINT('Ctrl Pts',(-1.0164049690006,0.148138950569523,56.30939138019));
#42812=CARTESIAN_POINT('Ctrl Pts',(-1.01653237544382,-1.90345246380841E-5,
56.3163519675715));
#42813=CARTESIAN_POINT('Origin',(-1.39932914042665E-16,0.,56.061775));
#42814=CARTESIAN_POINT('',(-1.188225,-1.45515594291686E-16,56.061775));
#42815=CARTESIAN_POINT('Origin',(0.,0.,56.061775));
#42816=CARTESIAN_POINT('Origin',(0.,0.,56.061775));
#42817=CARTESIAN_POINT('',(0.590159702139036,-0.827606761449038,56.061775));
#42818=CARTESIAN_POINT('Ctrl Pts',(0.51188116271663,1.07235883428022,56.061775));
#42819=CARTESIAN_POINT('Ctrl Pts',(0.541213176492396,1.05580342052956,56.061775));
#42820=CARTESIAN_POINT('Ctrl Pts',(0.569790684119403,1.03802023520366,56.061775));
#42821=CARTESIAN_POINT('Ctrl Pts',(0.597526191562895,1.01903462026179,56.061775));
#42822=CARTESIAN_POINT('Ctrl Pts',(0.637347544902611,0.991775956164436,
56.061775));
#42823=CARTESIAN_POINT('Ctrl Pts',(0.675434955264935,0.962039574884752,
56.061775));
#42824=CARTESIAN_POINT('Ctrl Pts',(0.71159321261738,0.93002723358959,56.061775));
#42825=CARTESIAN_POINT('Ctrl Pts',(0.726011613921828,0.917262050273659,
56.061775));
#42826=CARTESIAN_POINT('Ctrl Pts',(0.740122868411796,0.904134654496627,
56.061775));
#42827=CARTESIAN_POINT('Ctrl Pts',(0.753912893302178,0.890656748358753,
56.061775));
#42828=CARTESIAN_POINT('Ctrl Pts',(0.761733778079262,0.883012878838677,
56.061775));
#42829=CARTESIAN_POINT('Ctrl Pts',(0.769449908587933,0.875257488451145,
56.061775));
#42830=CARTESIAN_POINT('Ctrl Pts',(0.777050882853695,0.867401269087382,
56.061775));
#42831=CARTESIAN_POINT('Ctrl Pts',(0.811293653595113,0.832008606362631,
56.061775));
#42832=CARTESIAN_POINT('Ctrl Pts',(0.843249837994183,0.794526298977129,
56.061775));
#42833=CARTESIAN_POINT('Ctrl Pts',(0.872709194442015,0.755171056647391,
56.061775));
#42834=CARTESIAN_POINT('Ctrl Pts',(0.89231737439278,0.728976164203832,56.061775));
#42835=CARTESIAN_POINT('Ctrl Pts',(0.910818581336676,0.701950826308563,
56.061775));
#42836=CARTESIAN_POINT('Ctrl Pts',(0.928139018358984,0.674153489571596,
56.061775));
#42837=CARTESIAN_POINT('Ctrl Pts',(0.934162982461366,0.664485710494795,
56.061775));
#42838=CARTESIAN_POINT('Ctrl Pts',(0.940044027421705,0.654724521261419,
56.061775));
#42839=CARTESIAN_POINT('Ctrl Pts',(0.945778745449567,0.644872304782569,
56.061775));
#42840=CARTESIAN_POINT('Ctrl Pts',(0.950955710423823,0.635978305220254,
56.061775));
#42841=CARTESIAN_POINT('Ctrl Pts',(0.956008715846062,0.627018150888133,
56.061775));
#42842=CARTESIAN_POINT('Ctrl Pts',(0.96093425992874,0.617996981091859,56.061775));
#42843=CARTESIAN_POINT('Ctrl Pts',(0.966240504073969,0.608278556363322,
56.061775));
#42844=CARTESIAN_POINT('Ctrl Pts',(0.971399496552275,0.598488166785784,
56.061775));
#42845=CARTESIAN_POINT('Ctrl Pts',(0.976408975960127,0.588628330568485,
56.061775));
#42846=CARTESIAN_POINT('Ctrl Pts',(0.998306629291214,0.545528587499521,
56.061775));
#42847=CARTESIAN_POINT('Ctrl Pts',(1.01735139806086,0.501103250971285,56.061775));
#42848=CARTESIAN_POINT('Ctrl Pts',(1.03348950286457,0.455649362549699,56.061775));
#42849=CARTESIAN_POINT('Ctrl Pts',(1.04951099106991,0.410523931398352,56.061775));
#42850=CARTESIAN_POINT('Ctrl Pts',(1.06266777045703,0.364383618467088,56.061775));
#42851=CARTESIAN_POINT('Ctrl Pts',(1.07285691829592,0.317511905876643,56.061775));
#42852=CARTESIAN_POINT('Ctrl Pts',(1.07837716427354,0.292117889911543,56.061775));
#42853=CARTESIAN_POINT('Ctrl Pts',(1.08302546433836,0.266509169083111,56.061775));
#42854=CARTESIAN_POINT('Ctrl Pts',(1.08677904430391,0.240731714446861,56.061775));
#42855=CARTESIAN_POINT('Ctrl Pts',(1.0880860079379,0.231756230749861,56.061775));
#42856=CARTESIAN_POINT('Ctrl Pts',(1.08928435565178,0.222760175096169,56.061775));
#42857=CARTESIAN_POINT('Ctrl Pts',(1.09037158929866,0.213760065440079,56.061775));
#42858=CARTESIAN_POINT('Ctrl Pts',(1.09603301779298,0.166894814897787,56.061775));
#42859=CARTESIAN_POINT('Ctrl Pts',(1.09870084944373,0.119821996076729,56.061775));
#42860=CARTESIAN_POINT('Ctrl Pts',(1.09830409626352,0.0728155162236506,
56.061775));
#42861=CARTESIAN_POINT('Ctrl Pts',(1.09823697088453,0.0648626429196009,
56.061775));
#42862=CARTESIAN_POINT('Ctrl Pts',(1.09808200359928,0.0569116710356248,
56.061775));
#42863=CARTESIAN_POINT('Ctrl Pts',(1.09783870224064,0.0489639378119466,
56.061775));
#42864=CARTESIAN_POINT('Ctrl Pts',(1.09646708930469,0.00415854189393555,
56.061775));
#42865=CARTESIAN_POINT('Ctrl Pts',(1.09229131175929,-0.0405450829525213,
56.061775));
#42866=CARTESIAN_POINT('Ctrl Pts',(1.08536508685724,-0.0848917630206196,
56.061775));
#42867=CARTESIAN_POINT('Ctrl Pts',(1.08219399192013,-0.105195396620489,
56.061775));
#42868=CARTESIAN_POINT('Ctrl Pts',(1.07844580825791,-0.125424005149654,
56.061775));
#42869=CARTESIAN_POINT('Ctrl Pts',(1.0741230344062,-0.145551711443283,56.061775));
#42870=CARTESIAN_POINT('Ctrl Pts',(1.07095359998539,-0.16030923689511,56.061775));
#42871=CARTESIAN_POINT('Ctrl Pts',(1.06747524639181,-0.175012501031669,
56.061775));
#42872=CARTESIAN_POINT('Ctrl Pts',(1.0636884290732,-0.189650892812463,56.061775));
#42873=CARTESIAN_POINT('Ctrl Pts',(1.06147412044756,-0.198210565608511,
56.061775));
#42874=CARTESIAN_POINT('Ctrl Pts',(1.05915657217545,-0.206739316939933,
56.061775));
#42875=CARTESIAN_POINT('Ctrl Pts',(1.0567371423407,-0.215232892687751,56.061775));
#42876=CARTESIAN_POINT('Ctrl Pts',(1.04410920283738,-0.259564147585017,
56.061775));
#42877=CARTESIAN_POINT('Ctrl Pts',(1.02870411368939,-0.302960040082526,
56.061775));
#42878=CARTESIAN_POINT('Ctrl Pts',(1.01059776657305,-0.345147467590477,
56.061775));
#42879=CARTESIAN_POINT('Ctrl Pts',(0.993177632510785,-0.38573603237434,
56.061775));
#42880=CARTESIAN_POINT('Ctrl Pts',(0.973256491999253,-0.425206742761526,
56.061775));
#42881=CARTESIAN_POINT('Ctrl Pts',(0.950863549147145,-0.463291842602604,
56.061775));
#42882=CARTESIAN_POINT('Ctrl Pts',(0.939898284887777,-0.481941163813304,
56.061775));
#42883=CARTESIAN_POINT('Ctrl Pts',(0.928339758868041,-0.500257777247556,
56.061775));
#42884=CARTESIAN_POINT('Ctrl Pts',(0.916206631623963,-0.518216412717626,
56.061775));
#42885=CARTESIAN_POINT('Ctrl Pts',(0.906618806063435,-0.532407664546469,
56.061775));
#42886=CARTESIAN_POINT('Ctrl Pts',(0.896672138992213,-0.546375343126482,
56.061775));
#42887=CARTESIAN_POINT('Ctrl Pts',(0.886375271377727,-0.560105994464807,
56.061775));
#42888=CARTESIAN_POINT('Ctrl Pts',(0.881062189104107,-0.567190875320056,
56.061775));
#42889=CARTESIAN_POINT('Ctrl Pts',(0.875661590439594,-0.574204963613947,
56.061775));
#42890=CARTESIAN_POINT('Ctrl Pts',(0.870176513113682,-0.581145175673688,
56.061775));
#42891=CARTESIAN_POINT('Ctrl Pts',(0.842127545718367,-0.616635246316926,
56.061775));
#42892=CARTESIAN_POINT('Ctrl Pts',(0.81186116587577,-0.650211508350667,
56.061775));
#42893=CARTESIAN_POINT('Ctrl Pts',(0.779583315567684,-0.681676312373442,
56.061775));
#42894=CARTESIAN_POINT('Ctrl Pts',(0.747876545089263,-0.712584421487781,
56.061775));
#42895=CARTESIAN_POINT('Ctrl Pts',(0.714227917032577,-0.741455699548816,
56.061775));
#42896=CARTESIAN_POINT('Ctrl Pts',(0.678805048714601,-0.768062116484009,
56.061775));
#42897=CARTESIAN_POINT('Ctrl Pts',(0.650373815730447,-0.789417056800181,
56.061775));
#42898=CARTESIAN_POINT('Ctrl Pts',(0.620798928602909,-0.809312328764666,
56.061775));
#42899=CARTESIAN_POINT('Ctrl Pts',(0.590159702138998,-0.827606761449064,
56.061775));
#42900=CARTESIAN_POINT('Origin',(0.,0.,56.061775));
#42901=CARTESIAN_POINT('Origin',(0.,0.,55.5071980324285));
#42902=CARTESIAN_POINT('Ctrl Pts',(0.590159702138998,-0.827606761449064,
56.061775));
#42903=CARTESIAN_POINT('Ctrl Pts',(0.727528654917474,-0.729650069900356,
56.0697001217657));
#42904=CARTESIAN_POINT('Ctrl Pts',(0.952386591942655,-0.464074653132307,
56.0855503652972));
#42905=CARTESIAN_POINT('Ctrl Pts',(1.05840218504528,0.0472158302600112,
56.1093257305943));
#42906=CARTESIAN_POINT('Ctrl Pts',(0.907323368999851,0.546975187147921,
56.1331010958915));
#42907=CARTESIAN_POINT('Ctrl Pts',(0.535893220447681,0.913924938167876,
56.1568764611886));
#42908=CARTESIAN_POINT('Ctrl Pts',(0.0343021097832936,1.05889180686411,
56.1806518264858));
#42909=CARTESIAN_POINT('Ctrl Pts',(-0.475617027886791,0.946689808672358,
56.2044271917829));
#42910=CARTESIAN_POINT('Ctrl Pts',(-0.870023079724685,0.604559065518011,
56.22820255708));
#42911=CARTESIAN_POINT('Ctrl Pts',(-1.00549040154112,0.242800257196262,
56.2457928372953));
#42912=CARTESIAN_POINT('Ctrl Pts',(-1.01652086625353,0.0370683686476844,
56.2554579957447));
#42913=CARTESIAN_POINT('Ctrl Pts',(-1.01648283811887,2.60095369413633E-5,
56.2571980324285));
#42914=CARTESIAN_POINT('Ctrl Pts',(0.689876791927102,-0.967444397671189,
55.9626150912667));
#42915=CARTESIAN_POINT('Ctrl Pts',(0.850456465716625,-0.85293632829864,
55.9705402130324));
#42916=CARTESIAN_POINT('Ctrl Pts',(1.11330781200822,-0.542487621159544,
55.9863904565638));
#42917=CARTESIAN_POINT('Ctrl Pts',(1.2372364655554,0.0551937134810881,56.010165821861));
#42918=CARTESIAN_POINT('Ctrl Pts',(1.06063042389617,0.639395550061563,56.0339411871581));
#42919=CARTESIAN_POINT('Ctrl Pts',(0.626441104667066,1.06834743565215,56.0577165524553));
#42920=CARTESIAN_POINT('Ctrl Pts',(0.0400980096876628,1.23780881695182,
56.0814919177524));
#42921=CARTESIAN_POINT('Ctrl Pts',(-0.555980268044734,1.10664846445778,
56.1052672830496));
#42922=CARTESIAN_POINT('Ctrl Pts',(-1.01702764347953,0.706709162178262,
56.1290426483467));
#42923=CARTESIAN_POINT('Ctrl Pts',(-1.2310656854131,0.135131117029301,56.1528180136439));
#42924=CARTESIAN_POINT('Ctrl Pts',(-1.14611146910879,-0.469267475342316,
56.1765933789411));
#42925=CARTESIAN_POINT('Ctrl Pts',(-0.782797550539819,-0.959693272702349,
56.2003687442382));
#42926=CARTESIAN_POINT('Ctrl Pts',(-0.229363317643444,-1.21703566512132,
56.2241441095354));
#42927=CARTESIAN_POINT('Ctrl Pts',(0.379777109177097,-1.17879286552796,
56.2479194748325));
#42928=CARTESIAN_POINT('Ctrl Pts',(0.896679912107581,-0.854253141586999,
56.2716948401297));
#42929=CARTESIAN_POINT('Ctrl Pts',(1.19580337944822,-0.322238373221072,
56.2954702054269));
#42930=CARTESIAN_POINT('Ctrl Pts',(1.20449848491306,0.288039388201827,56.319245570724));
#42931=CARTESIAN_POINT('Ctrl Pts',(0.920653427402792,0.828360162236165,
56.3430209360211));
#42932=CARTESIAN_POINT('Ctrl Pts',(0.41320650609164,1.16749461393021,56.3667963013183));
#42933=CARTESIAN_POINT('Ctrl Pts',(-0.19459712002736,1.22307614310528,56.3905716666154));
#42934=CARTESIAN_POINT('Ctrl Pts',(-0.75513835931515,0.981605495597739,
56.4143470319126));
#42935=CARTESIAN_POINT('Ctrl Pts',(-1.13227687719907,0.501729373380553,
56.4381223972098));
#42936=CARTESIAN_POINT('Ctrl Pts',(-1.23441590924795,-0.100003268739267,
56.4618977625069));
#42937=CARTESIAN_POINT('Ctrl Pts',(-1.03674864192874,-0.677447816589128,
56.4856731278041));
#42938=CARTESIAN_POINT('Ctrl Pts',(-0.587283118157996,-1.09035857858026,
56.5094484931012));
#42939=CARTESIAN_POINT('Ctrl Pts',(0.00481762038262453,-1.23845067777583,
56.5332238583984));
#42940=CARTESIAN_POINT('Ctrl Pts',(0.595748288989899,-1.08575654127344,
56.5569992236955));
#42941=CARTESIAN_POINT('Ctrl Pts',(1.04198778136724,-0.669361452604685,
56.5807745889927));
#42942=CARTESIAN_POINT('Ctrl Pts',(1.23515657175416,-0.0903965375675185,
56.6045499542899));
#42943=CARTESIAN_POINT('Ctrl Pts',(1.12833917586245,0.510523256048042,56.628325319587));
#42944=CARTESIAN_POINT('Ctrl Pts',(0.747478655449841,0.987450733150073,
56.6521006848842));
#42945=CARTESIAN_POINT('Ctrl Pts',(0.185075748994057,1.22455308496042,56.6758760501813));
#42946=CARTESIAN_POINT('Ctrl Pts',(-0.422277060480572,1.16424455117628,
56.6996514154785));
#42947=CARTESIAN_POINT('Ctrl Pts',(-0.927070171999913,0.821172446529851,
56.7234267807756));
#42948=CARTESIAN_POINT('Ctrl Pts',(-1.20670296646235,0.278659723467029,
56.7472021460728));
#42949=CARTESIAN_POINT('Ctrl Pts',(-1.19326018722141,-0.331531923567072,
56.7709775113699));
#42950=CARTESIAN_POINT('Ctrl Pts',(-0.890006722445684,-0.861203416594047,
56.7947528766671));
#42951=CARTESIAN_POINT('Ctrl Pts',(-0.370594651923479,-1.18171184927523,
56.8185282419642));
#42952=CARTESIAN_POINT('Ctrl Pts',(0.238824854763645,-1.21521437594315,
56.8423036072614));
#42953=CARTESIAN_POINT('Ctrl Pts',(0.790240251682412,-0.953574137323725,
56.8660789725585));
#42954=CARTESIAN_POINT('Ctrl Pts',(1.14972762524983,-0.460336483986605,
56.8898543378557));
#42955=CARTESIAN_POINT('Ctrl Pts',(1.22997719735517,0.144704473801232,56.9136297031528));
#42956=CARTESIAN_POINT('Ctrl Pts',(1.01149851339784,0.714600621428312,56.93740506845));
#42957=CARTESIAN_POINT('Ctrl Pts',(0.547354147534323,1.11093956988161,56.9611804337472));
#42958=CARTESIAN_POINT('Ctrl Pts',(-0.0497277640765374,1.23746128837702,
56.9849557990443));
#42959=CARTESIAN_POINT('Ctrl Pts',(-0.634732144272647,1.0634370671454,57.0087311643415));
#42960=CARTESIAN_POINT('Ctrl Pts',(-1.06557722222055,0.631132691465518,
57.0325065296386));
#42961=CARTESIAN_POINT('Ctrl Pts',(-1.23762235982929,0.0455432234513654,
57.0562818949358));
#42962=CARTESIAN_POINT('Ctrl Pts',(-1.10908243780363,-0.551107464027959,
57.0800572602329));
#42963=CARTESIAN_POINT('Ctrl Pts',(-0.711176333065604,-1.01390902651033,
57.1038326255301));
#42964=CARTESIAN_POINT('Ctrl Pts',(-0.140544696353038,-1.2304594585271,
57.1276079908272));
#42965=CARTESIAN_POINT('Ctrl Pts',(0.46422145287787,-1.14816450626194,57.1513833561244));
#42966=CARTESIAN_POINT('Ctrl Pts',(0.956240743595242,-0.787011391937999,
57.1751587214215));
#42967=CARTESIAN_POINT('Ctrl Pts',(1.21601497292081,-0.234714457126464,
57.1989340867187));
#42968=CARTESIAN_POINT('Ctrl Pts',(1.18045199356654,0.374588282834027,57.2227094520159));
#42969=CARTESIAN_POINT('Ctrl Pts',(0.858189093138855,0.892913641495793,
57.246484817313));
#42970=CARTESIAN_POINT('Ctrl Pts',(0.327495230156222,1.19437438225068,57.2702601826101));
#42971=CARTESIAN_POINT('Ctrl Pts',(-0.282738382980947,1.20575382957762,
57.2940355479073));
#42972=CARTESIAN_POINT('Ctrl Pts',(-0.824302475860749,0.924288222927029,
57.3178109132045));
#42973=CARTESIAN_POINT('Ctrl Pts',(-1.16566575069977,0.418337959546242,
57.3415862785016));
#42974=CARTESIAN_POINT('Ctrl Pts',(-1.22392028367976,-0.189215300515123,
57.3653616437988));
#42975=CARTESIAN_POINT('Ctrl Pts',(-0.984917621412899,-0.750813272246919,
57.3891370090959));
#42976=CARTESIAN_POINT('Ctrl Pts',(-0.506705058309881,-1.13005896953874,
57.4129123743931));
#42977=CARTESIAN_POINT('Ctrl Pts',(0.0945724841541603,-1.2348438508543,
57.4366877396902));
#42978=CARTESIAN_POINT('Ctrl Pts',(0.672880923350564,-1.03971849735525,
57.4604631049874));
#42979=CARTESIAN_POINT('Ctrl Pts',(1.0877647517472,-0.592073589689751,57.4842384702846));
#42980=CARTESIAN_POINT('Ctrl Pts',(1.23845988787003,-0.0006299910492471,
57.5080138355817));
#42981=CARTESIAN_POINT('Ctrl Pts',(1.08836655140774,0.59096661540952,57.5317892008789));
#42982=CARTESIAN_POINT('Ctrl Pts',(0.673938361780622,1.03903338506143,57.555564566176));
#42983=CARTESIAN_POINT('Ctrl Pts',(0.095828738106295,1.23474699582737,57.5793399314732));
#42984=CARTESIAN_POINT('Ctrl Pts',(-0.505555099006082,1.13057389524998,
57.6031152967703));
#42985=CARTESIAN_POINT('Ctrl Pts',(-0.984153250827362,0.751814917142313,
57.6268906620675));
#42986=CARTESIAN_POINT('Ctrl Pts',(-1.22372714679232,0.190460392090562,
57.6506660273646));
#42987=CARTESIAN_POINT('Ctrl Pts',(-1.16609075524636,-0.417151820421223,
57.6744413926618));
#42988=CARTESIAN_POINT('Ctrl Pts',(-0.82524239971067,-0.923449117424206,
57.6982167579589));
#42989=CARTESIAN_POINT('Ctrl Pts',(-0.283964944005771,-1.20546555377064,
57.7219921232561));
#42990=CARTESIAN_POINT('Ctrl Pts',(0.326279930516472,-1.19470695055061,
57.7457674885532));
#42991=CARTESIAN_POINT('Ctrl Pts',(0.857280218357737,-0.893786282040778,
57.7695428538504));
#42992=CARTESIAN_POINT('Ctrl Pts',(1.18007028479188,-0.375789054794004,
57.7933182191476));
#42993=CARTESIAN_POINT('Ctrl Pts',(1.21625313690915,0.233477188843838,57.8170935844447));
#42994=CARTESIAN_POINT('Ctrl Pts',(0.957040936743427,0.786038126396572,
57.8408689497418));
#42995=CARTESIAN_POINT('Ctrl Pts',(0.465389329872678,1.14769162338689,57.864644315039));
#42996=CARTESIAN_POINT('Ctrl Pts',(-0.139292781304968,1.23060180880254,
57.8884196803362));
#42997=CARTESIAN_POINT('Ctrl Pts',(-0.710144436332023,1.01463203689734,
57.9121950456333));
#42998=CARTESIAN_POINT('Ctrl Pts',(-1.10852117924344,0.552235534822328,
57.9359704109305));
#42999=CARTESIAN_POINT('Ctrl Pts',(-1.2376680539947,-0.0442840701915317,
57.9597457762276));
#43000=CARTESIAN_POINT('Ctrl Pts',(-1.06621877123237,-0.630048270074204,
57.9835211415248));
#43001=CARTESIAN_POINT('Ctrl Pts',(-0.635813733195539,-1.0627907543029,
58.007296506822));
#43002=CARTESIAN_POINT('Ctrl Pts',(-0.0509867041603225,-1.23741005602453,
58.0310718721191));
#43003=CARTESIAN_POINT('Ctrl Pts',(0.546223618848922,-1.11149586097446,
58.0548472374163));
#43004=CARTESIAN_POINT('Ctrl Pts',(1.0107709710081,-0.715629327877998,58.0786226027134));
#43005=CARTESIAN_POINT('Ctrl Pts',(1.2298293416664,-0.145955750582684,58.1023979680106));
#43006=CARTESIAN_POINT('Ctrl Pts',(1.15019536641724,0.459166538223408,58.1261733333077));
#43007=CARTESIAN_POINT('Ctrl Pts',(0.791209988003854,0.952769670820134,
58.1499486986049));
#43008=CARTESIAN_POINT('Ctrl Pts',(0.240061063466199,1.21497077189505,58.173724063902));
#43009=CARTESIAN_POINT('Ctrl Pts',(-0.36939221256026,1.18208827252943,58.1974994291992));
#43010=CARTESIAN_POINT('Ctrl Pts',(-0.889130092481378,0.862108444104235,
58.2212747944963));
#43011=CARTESIAN_POINT('Ctrl Pts',(-1.19292227640834,0.332745748583669,
58.2450501597935));
#43012=CARTESIAN_POINT('Ctrl Pts',(-1.20698584421457,-0.277431906271434,
58.2688255250906));
#43013=CARTESIAN_POINT('Ctrl Pts',(-0.927905134948138,-0.820228840805201,
58.2926008903878));
#43014=CARTESIAN_POINT('Ctrl Pts',(-0.423461318665824,-1.16381433327897,
58.316376255685));
#43015=CARTESIAN_POINT('Ctrl Pts',(0.183829819914051,-1.22474074320329,
58.3401516209821));
#43016=CARTESIAN_POINT('Ctrl Pts',(0.746473658012812,-0.98821069041209,
58.3639269862793));
#43017=CARTESIAN_POINT('Ctrl Pts',(1.12781919681433,-0.511670939226426,
58.3877023515764));
#43018=CARTESIAN_POINT('Ctrl Pts',(1.23524789996815,0.0891398697331011,
58.4114777168736));
#43019=CARTESIAN_POINT('Ctrl Pts',(1.04266823568555,0.668301010805869,58.4352530821707));
#43020=CARTESIAN_POINT('Ctrl Pts',(0.596852605428911,1.08514987819401,58.4590284474679));
#43021=CARTESIAN_POINT('Ctrl Pts',(0.00607759029129267,1.23844513550178,
58.4828038127651));
#43022=CARTESIAN_POINT('Ctrl Pts',(-0.586173507453946,1.09095550317642,
58.5065791780622));
#43023=CARTESIAN_POINT('Ctrl Pts',(-1.03605888491723,0.678502231194445,
58.5303545433593));
#43024=CARTESIAN_POINT('Ctrl Pts',(-1.23431352927824,0.101259084493505,
58.5541299086565));
#43025=CARTESIAN_POINT('Ctrl Pts',(-1.13278673961859,-0.50057716018217,
58.5779052739537));
#43026=CARTESIAN_POINT('Ctrl Pts',(-0.756136632270754,-0.980836726519766,
58.6016806392508));
#43027=CARTESIAN_POINT('Ctrl Pts',(-0.195841350045654,-1.22287753122055,
58.625456004548));
#43028=CARTESIAN_POINT('Ctrl Pts',(0.412018509059322,-1.16791439709608,
58.6492313698451));
#43029=CARTESIAN_POINT('Ctrl Pts',(0.919810195403461,-0.829296385608678,
58.6730067351423));
#43030=CARTESIAN_POINT('Ctrl Pts',(1.20420481701146,-0.289264670221184,
58.6967821004394));
#43031=CARTESIAN_POINT('Ctrl Pts',(1.19613059797621,0.321021624406906,58.7205574657366));
#43032=CARTESIAN_POINT('Ctrl Pts',(0.897548548125092,0.853340432951767,
58.7443328310338));
#43033=CARTESIAN_POINT('Ctrl Pts',(0.380976186673455,1.17840588760389,58.7681081963309));
#43034=CARTESIAN_POINT('Ctrl Pts',(-0.228125005467955,1.21726836508307,
58.7918835616281));
#43035=CARTESIAN_POINT('Ctrl Pts',(-0.781820792375621,0.960489218763501,
58.8156589269252));
#43036=CARTESIAN_POINT('Ctrl Pts',(-1.14563341530098,0.47043317112805,58.8394342922223));
#43037=CARTESIAN_POINT('Ctrl Pts',(-1.23120260983117,-0.133878393688783,
58.8632096575195));
#43038=CARTESIAN_POINT('Ctrl Pts',(-1.01774592869022,-0.705674510937058,
58.8869850228167));
#43039=CARTESIAN_POINT('Ctrl Pts',(-0.557106237127393,-1.10608134027545,
58.9107603881138));
#43040=CARTESIAN_POINT('Ctrl Pts',(0.0388395194718907,-1.2378508724717,
58.934535753411));
#43041=CARTESIAN_POINT('Ctrl Pts',(0.62535220532555,-1.06897984548177,58.9583111187081));
#43042=CARTESIAN_POINT('Ctrl Pts',(1.059983722875,-0.64048247282172,58.9820864840053));
#43043=CARTESIAN_POINT('Ctrl Pts',(1.23717381007099,-0.056429198348077,
59.0058618493025));
#43044=CARTESIAN_POINT('Ctrl Pts',(1.11388777825955,0.541329205009086,59.0296372145996));
#43045=CARTESIAN_POINT('Ctrl Pts',(0.720068476266758,1.00761335850545,59.0534125798967));
#43046=CARTESIAN_POINT('Ctrl Pts',(0.151363980773296,1.22917542933311,59.0771879451939));
#43047=CARTESIAN_POINT('Ctrl Pts',(-0.454102739340545,1.15220397190566,
59.100963310491));
#43048=CARTESIAN_POINT('Ctrl Pts',(-0.949280163288418,0.795393275266316,
59.1247386757882));
#43049=CARTESIAN_POINT('Ctrl Pts',(-1.21390306288918,0.245403024961089,
59.1485140410854));
#43050=CARTESIAN_POINT('Ctrl Pts',(-1.18370167974241,-0.364188995065361,
59.1722894063825));
#43051=CARTESIAN_POINT('Ctrl Pts',(-0.866011114480599,-0.885329340046922,
59.1960647716797));
#43052=CARTESIAN_POINT('Ctrl Pts',(-0.337989828847549,-1.19144708919335,
59.2198401369768));
#43053=CARTESIAN_POINT('Ctrl Pts',(0.272120061643497,-1.20819450536858,
59.243615502274));
#43054=CARTESIAN_POINT('Ctrl Pts',(0.816139335472622,-0.931504093306501,
59.2673908675711));
#43055=CARTESIAN_POINT('Ctrl Pts',(1.16194039768241,-0.428576484402961,
59.2911662328683));
#43056=CARTESIAN_POINT('Ctrl Pts',(1.22553750571355,0.178440782463945,59.3149415981654));
#43057=CARTESIAN_POINT('Ctrl Pts',(0.991484638916142,0.742119600560311,
59.3387169634626));
#43058=CARTESIAN_POINT('Ctrl Pts',(0.516626920037774,1.12555760237105,59.3624923287597));
#43059=CARTESIAN_POINT('Ctrl Pts',(-0.0837055306015586,1.23562804876679,
59.3862676940569));
#43060=CARTESIAN_POINT('Ctrl Pts',(-0.66370816752893,1.04559779985052,59.4100430593541));
#43061=CARTESIAN_POINT('Ctrl Pts',(-1.08251400861023,0.601620072902204,
59.4338184246512));
#43062=CARTESIAN_POINT('Ctrl Pts',(-1.23840642074766,0.011525071951662,
59.4575937899484));
#43063=CARTESIAN_POINT('Ctrl Pts',(-1.0935233469385,-0.581369057887385,
59.4813691552455));
#43064=CARTESIAN_POINT('Ctrl Pts',(-0.683052971567649,-1.033064338435,59.5051445205427));
#43065=CARTESIAN_POINT('Ctrl Pts',(-0.106687473759109,-1.23385618060568,
59.5289198858398));
#43066=CARTESIAN_POINT('Ctrl Pts',(0.495589540417238,-1.13497766591134,
59.552695251137));
#43067=CARTESIAN_POINT('Ctrl Pts',(0.977501214644604,-0.760443717735149,
59.5764706164341));
#43068=CARTESIAN_POINT('Ctrl Pts',(1.22200427569806,-0.201218517620435,
59.6002459817313));
#43069=CARTESIAN_POINT('Ctrl Pts',(1.16971539613015,0.406877223320946,59.6240213470285));
#43070=CARTESIAN_POINT('Ctrl Pts',(0.83333442333768,0.916153481637932,59.6477967123256));
#43071=CARTESIAN_POINT('Ctrl Pts',(0.294558588880807,1.20292076975491,59.6715720776228));
#43072=CARTESIAN_POINT('Ctrl Pts',(-0.315756654949849,1.19753112793076,
59.6953474429199));
#43073=CARTESIAN_POINT('Ctrl Pts',(-0.849385120103183,0.901293403997361,
59.7191228082171));
#43074=CARTESIAN_POINT('Ctrl Pts',(-1.17671661268543,0.386156096850363,
59.7428981735142));
#43075=CARTESIAN_POINT('Ctrl Pts',(-1.21826471063664,-0.222768480037991,
59.7666735388113));
#43076=CARTESIAN_POINT('Ctrl Pts',(-0.963909730368294,-0.777587035150415,
59.7904489041086));
#43077=CARTESIAN_POINT('Ctrl Pts',(-0.475491739768952,-1.14355062114423,
59.8142242694057));
#43078=CARTESIAN_POINT('Ctrl Pts',(0.128495139722361,-1.23176138211002,
59.8379996347029));
#43079=CARTESIAN_POINT('Ctrl Pts',(0.5101794029784,-1.09109740948615,59.8538498782343));
#43080=CARTESIAN_POINT('Ctrl Pts',(0.672748867539255,-0.97943229058963,
59.861775));
#43081=CARTESIAN_POINT('Ctrl Pts',(0.656637761997734,-0.920831852263814,
55.9956683941778));
#43082=CARTESIAN_POINT('Ctrl Pts',(0.809480528783575,-0.811840908832545,
56.0035935159435));
#43083=CARTESIAN_POINT('Ctrl Pts',(1.0596674053197,-0.516349965150465,56.0194437594749));
#43084=CARTESIAN_POINT('Ctrl Pts',(1.17762503871869,0.0525344190740624,
56.0432191247721));
#43085=CARTESIAN_POINT('Ctrl Pts',(1.00952807226406,0.608588762423683,56.0669944900692));
#43086=CARTESIAN_POINT('Ctrl Pts',(0.596258476593938,1.01687326982406,56.0907698553664));
#43087=CARTESIAN_POINT('Ctrl Pts',(0.0381660430528731,1.17816981358925,
56.1145452206636));
#43088=CARTESIAN_POINT('Ctrl Pts',(-0.529192521325419,1.0533289125293,56.1383205859607));
#43089=CARTESIAN_POINT('Ctrl Pts',(-0.968026122227916,0.672659129958179,
56.1620959512579));
#43090=CARTESIAN_POINT('Ctrl Pts',(-1.17175157361617,0.128620349750434,
56.185871316555));
#43091=CARTESIAN_POINT('Ctrl Pts',(-1.09089054579335,-0.44665764726822,
56.2096466818522));
#43092=CARTESIAN_POINT('Ctrl Pts',(-0.745081495273847,-0.913454185103445,
56.2334220471493));
#43093=CARTESIAN_POINT('Ctrl Pts',(-0.218312338296022,-1.15839753528211,
56.2571974124465));
#43094=CARTESIAN_POINT('Ctrl Pts',(0.361479026322095,-1.12199731624102,
56.2809727777436));
#43095=CARTESIAN_POINT('Ctrl Pts',(0.853476878197205,-0.813094276594377,
56.3047481430408));
#43096=CARTESIAN_POINT('Ctrl Pts',(1.13818824471077,-0.306712570560035,
56.3285235083379));
#43097=CARTESIAN_POINT('Ctrl Pts',(1.14646441033857,0.274161330616311,56.3522988736351));
#43098=CARTESIAN_POINT('Ctrl Pts',(0.876295322903381,0.788448849742304,
56.3760742389322));
#43099=CARTESIAN_POINT('Ctrl Pts',(0.393297757770615,1.11124342695173,56.3998496042294));
#43100=CARTESIAN_POINT('Ctrl Pts',(-0.185221214688251,1.16414697632897,
56.4236249695266));
#43101=CARTESIAN_POINT('Ctrl Pts',(-0.718754954597366,0.934310652766648,
56.4474003348237));
#43102=CARTESIAN_POINT('Ctrl Pts',(-1.07772251988488,0.477555495010681,
56.4711757001209));
#43103=CARTESIAN_POINT('Ctrl Pts',(-1.17494037994631,-0.0951850001997911,
56.494951065418));
#43104=CARTESIAN_POINT('Ctrl Pts',(-0.986796941072066,-0.644807628493671,
56.5187264307152));
#43105=CARTESIAN_POINT('Ctrl Pts',(-0.558987165359032,-1.03782389144296,
56.5425017960123));
#43106=CARTESIAN_POINT('Ctrl Pts',(0.00458550208272216,-1.17878074884598,
56.5662771613095));
#43107=CARTESIAN_POINT('Ctrl Pts',(0.567044474859859,-1.03344358540405,
56.5900525266066));
#43108=CARTESIAN_POINT('Ctrl Pts',(0.991783652954465,-0.637110874505737,
56.6138278919038));
#43109=CARTESIAN_POINT('Ctrl Pts',(1.17564535651048,-0.0860411320039726,
56.637603257201));
#43110=CARTESIAN_POINT('Ctrl Pts',(1.0739745413714,0.485925678645828,56.6613786224981));
#43111=CARTESIAN_POINT('Ctrl Pts',(0.711464303770228,0.939874260282695,
56.6851539877953));
#43112=CARTESIAN_POINT('Ctrl Pts',(0.176158593884617,1.16555275748542,56.7089293530924));
#43113=CARTESIAN_POINT('Ctrl Pts',(-0.401931282776427,1.10814995583041,
56.7327047183896));
#43114=CARTESIAN_POINT('Ctrl Pts',(-0.882402901620151,0.78160744616053,
56.7564800836867));
#43115=CARTESIAN_POINT('Ctrl Pts',(-1.14856267751879,0.265233588544357,
56.7802554489839));
#43116=CARTESIAN_POINT('Ctrl Pts',(-1.13576758630961,-0.31555834733007,
56.804030814281));
#43117=CARTESIAN_POINT('Ctrl Pts',(-0.847125210223656,-0.81970967963345,
56.8278061795782));
#43118=CARTESIAN_POINT('Ctrl Pts',(-0.352738990055884,-1.12477566010987,
56.8515815448753));
#43119=CARTESIAN_POINT('Ctrl Pts',(0.227318008050931,-1.15666399783905,
56.8753569101725));
#43120=CARTESIAN_POINT('Ctrl Pts',(0.752165598810427,-0.907629876462535,
56.8991322754696));
#43121=CARTESIAN_POINT('Ctrl Pts',(1.09433247151586,-0.438156960993706,
56.9229076407668));
#43122=CARTESIAN_POINT('Ctrl Pts',(1.17071553012162,0.137732451562079,56.946683006064));
#43123=CARTESIAN_POINT('Ctrl Pts',(0.962763391773544,0.68017036993826,56.9704583713611));
#43124=CARTESIAN_POINT('Ctrl Pts',(0.520982016880328,1.05741326772864,56.9942337366582));
#43125=CARTESIAN_POINT('Ctrl Pts',(-0.04733182518165,1.17783902932711,57.0180091019554));
#43126=CARTESIAN_POINT('Ctrl Pts',(-0.604150044704295,1.01219948832483,
57.0417844672526));
#43127=CARTESIAN_POINT('Ctrl Pts',(-1.01423652835186,0.600724017530526,
57.0655598325497));
#43128=CARTESIAN_POINT('Ctrl Pts',(-1.17799234017794,0.0433489003706404,
57.0893351978469));
#43129=CARTESIAN_POINT('Ctrl Pts',(-1.05564561433647,-0.524554494417324,
57.113110563144));
#43130=CARTESIAN_POINT('Ctrl Pts',(-0.676911067591465,-0.965057763687454,
57.1368859284412));
#43131=CARTESIAN_POINT('Ctrl Pts',(-0.133773096810682,-1.17117455541475,
57.1606612937383));
#43132=CARTESIAN_POINT('Ctrl Pts',(0.441854747769617,-1.09284466533661,
57.1844366590355));
#43133=CARTESIAN_POINT('Ctrl Pts',(0.910168002682683,-0.749092309114078,
57.2082120243326));
#43134=CARTESIAN_POINT('Ctrl Pts',(1.15742602116528,-0.223405653936416,
57.2319873896298));
#43135=CARTESIAN_POINT('Ctrl Pts',(1.12357650564827,0.356540203394322,57.2557627549269));
#43136=CARTESIAN_POINT('Ctrl Pts',(0.816840589629669,0.849892070685862,
57.2795381202241));
#43137=CARTESIAN_POINT('Ctrl Pts',(0.311716146290415,1.13682809818508,57.3033134855212));
#43138=CARTESIAN_POINT('Ctrl Pts',(-0.269115733713632,1.14765927110315,
57.3270888508185));
#43139=CARTESIAN_POINT('Ctrl Pts',(-0.784586667202436,0.879754989942892,
57.3508642161156));
#43140=CARTESIAN_POINT('Ctrl Pts',(-1.10950268038265,0.398181972099398,
57.3746395814127));
#43141=CARTESIAN_POINT('Ctrl Pts',(-1.16495044527317,-0.180098697216517,
57.3984149467099));
#43142=CARTESIAN_POINT('Ctrl Pts',(-0.937463196681984,-0.714638255027005,
57.422190312007));
#43143=CARTESIAN_POINT('Ctrl Pts',(-0.482291445914716,-1.07561147347857,
57.4459656773042));
#43144=CARTESIAN_POINT('Ctrl Pts',(0.0900158768467722,-1.17534770285084,
57.4697410426014));
#43145=CARTESIAN_POINT('Ctrl Pts',(0.640460773242784,-0.989623705566161,
57.4935164078985));
#43146=CARTESIAN_POINT('Ctrl Pts',(1.03535503806711,-0.563546826652665,
57.5172917731957));
#43147=CARTESIAN_POINT('Ctrl Pts',(1.17878951518762,-0.000599637380898037,
57.5410671384928));
#43148=CARTESIAN_POINT('Ctrl Pts',(1.03592784235172,0.562493187622534,57.56484250379));
#43149=CARTESIAN_POINT('Ctrl Pts',(0.641467263115012,0.988971602743467,
57.5886178690871));
#43150=CARTESIAN_POINT('Ctrl Pts',(0.0912116030884411,1.17525551440667,
57.6123932343843));
#43151=CARTESIAN_POINT('Ctrl Pts',(-0.481196892927188,1.07610158949723,
57.6361685996814));
#43152=CARTESIAN_POINT('Ctrl Pts',(-0.936735654320081,0.715591639559026,
57.6599439649786));
#43153=CARTESIAN_POINT('Ctrl Pts',(-1.16476661393545,0.181283798897194,
57.6837193302757));
#43154=CARTESIAN_POINT('Ctrl Pts',(-1.10990720773822,-0.397052982474613,
57.7074946955729));
#43155=CARTESIAN_POINT('Ctrl Pts',(-0.785481304477495,-0.87895631347501,
57.73127006087));
#43156=CARTESIAN_POINT('Ctrl Pts',(-0.270283197666202,-1.14738488474469,
57.7550454261672));
#43157=CARTESIAN_POINT('Ctrl Pts',(0.310559401136881,-1.137144642975,57.7788207914644));
#43158=CARTESIAN_POINT('Ctrl Pts',(0.815975505444798,-0.850722666440334,
57.8025961567615));
#43159=CARTESIAN_POINT('Ctrl Pts',(1.12321318802626,-0.357683120827827,
57.8263715220587));
#43160=CARTESIAN_POINT('Ctrl Pts',(1.15765271014818,0.222227998613616,57.8501468873558));
#43161=CARTESIAN_POINT('Ctrl Pts',(0.910929641636386,0.748165936587234,
57.873922252653));
#43162=CARTESIAN_POINT('Ctrl Pts',(0.442966355153904,1.09239456648361,57.8976976179501));
#43163=CARTESIAN_POINT('Ctrl Pts',(-0.132581500419862,1.17131004709584,
57.9214729832473));
#43164=CARTESIAN_POINT('Ctrl Pts',(-0.675928888788414,0.965745938631122,
57.9452483485444));
#43165=CARTESIAN_POINT('Ctrl Pts',(-1.05511139783698,0.525628213508114,
57.9690237138416));
#43166=CARTESIAN_POINT('Ctrl Pts',(-1.17803583274772,-0.0421504145131365,
57.9927990791388));
#43167=CARTESIAN_POINT('Ctrl Pts',(-1.01484716681986,-0.599691844766081,
58.0165744444359));
#43168=CARTESIAN_POINT('Ctrl Pts',(-0.605179521471793,-1.0115843155528,
58.0403498097331));
#43169=CARTESIAN_POINT('Ctrl Pts',(-0.0485301081341635,-1.17779026540625,
58.0641251750302));
#43170=CARTESIAN_POINT('Ctrl Pts',(0.519905958322425,-1.05794275609888,
58.0879005403274));
#43171=CARTESIAN_POINT('Ctrl Pts',(0.962070903184065,-0.681149512168836,
58.1116759056245));
#43172=CARTESIAN_POINT('Ctrl Pts',(1.17057479828413,-0.138923440438677,
58.1354512709216));
#43173=CARTESIAN_POINT('Ctrl Pts',(1.0947776763944,0.437043384516588,58.1592266362188));
#43174=CARTESIAN_POINT('Ctrl Pts',(0.753088612159024,0.906864170048437,
58.183002001516));
#43175=CARTESIAN_POINT('Ctrl Pts',(0.228494654845404,1.1564321309045,58.2067773668131));
#43176=CARTESIAN_POINT('Ctrl Pts',(-0.351594485556477,1.12513394687367,
58.2305527321103));
#43177=CARTESIAN_POINT('Ctrl Pts',(-0.846290817264516,0.820571101913176,
58.2543280974074));
#43178=CARTESIAN_POINT('Ctrl Pts',(-1.13544595641476,0.316713688909432,
58.2781034627046));
#43179=CARTESIAN_POINT('Ctrl Pts',(-1.14883192590677,-0.26406492894472,
58.3018788280017));
#43180=CARTESIAN_POINT('Ctrl Pts',(-0.883197635126317,-0.780709304407554,
58.3256541932989));
#43181=CARTESIAN_POINT('Ctrl Pts',(-0.403058482087211,-1.10774046630914,
58.3494295585961));
#43182=CARTESIAN_POINT('Ctrl Pts',(0.174972695051272,-1.16573137414575,
58.3732049238932));
#43183=CARTESIAN_POINT('Ctrl Pts',(0.710507728225752,-0.940597601959907,
58.3969802891904));
#43184=CARTESIAN_POINT('Ctrl Pts',(1.07347961549125,-0.487018065174191,
58.4207556544875));
#43185=CARTESIAN_POINT('Ctrl Pts',(1.1757322844297,0.0848450118213287,58.4445310197847));
#43186=CARTESIAN_POINT('Ctrl Pts',(0.992431322228083,0.636101525970394,
58.4683063850818));
#43187=CARTESIAN_POINT('Ctrl Pts',(0.568095584106511,1.03286615202548,58.492081750379));
#43188=CARTESIAN_POINT('Ctrl Pts',(0.00578476524201244,1.17877547360485,
58.5158571156761));
#43189=CARTESIAN_POINT('Ctrl Pts',(-0.557931016930909,1.0383920555492,58.5396324809733));
#43190=CARTESIAN_POINT('Ctrl Pts',(-0.986140417319333,0.645811240232391,
58.5634078462705));
#43191=CARTESIAN_POINT('Ctrl Pts',(-1.17484293275723,0.0963803093564249,
58.5871832115676));
#43192=CARTESIAN_POINT('Ctrl Pts',(-1.07820781656684,-0.476458796723713,
58.6109585768648));
#43193=CARTESIAN_POINT('Ctrl Pts',(-0.719705129653402,-0.933578923836559,
58.6347339421619));
#43194=CARTESIAN_POINT('Ctrl Pts',(-0.186405496322565,-1.1639579337854,
58.6585093074591));
#43195=CARTESIAN_POINT('Ctrl Pts',(0.392166999754567,-1.11164298449851,
58.6822846727562));
#43196=CARTESIAN_POINT('Ctrl Pts',(0.875492718758175,-0.789339964833067,
58.7060600380534));
#43197=CARTESIAN_POINT('Ctrl Pts',(1.14618489168258,-0.275327577187317,
58.7298354033505));
#43198=CARTESIAN_POINT('Ctrl Pts',(1.13849969748671,0.305554446054918,58.7536107686477));
#43199=CARTESIAN_POINT('Ctrl Pts',(0.854303662366784,0.81222554327474,58.7773861339448));
#43200=CARTESIAN_POINT('Ctrl Pts',(0.362620330933121,1.12162898334307,58.801161499242));
#43201=CARTESIAN_POINT('Ctrl Pts',(-0.217133689376275,1.15861902350129,
58.8249368645392));
#43202=CARTESIAN_POINT('Ctrl Pts',(-0.744151798402677,0.914211781599485,
58.8487122298363));
#43203=CARTESIAN_POINT('Ctrl Pts',(-1.09043552514888,0.447767178536508,
58.8724875951335));
#43204=CARTESIAN_POINT('Ctrl Pts',(-1.17188190086373,-0.127427984011593,
58.8962629604306));
#43205=CARTESIAN_POINT('Ctrl Pts',(-0.968709799659506,-0.671674329362741,
58.9200383257278));
#43206=CARTESIAN_POINT('Ctrl Pts',(-0.530264239967304,-1.05278911301986,
58.9438136910249));
#43207=CARTESIAN_POINT('Ctrl Pts',(0.036968188293232,-1.17820984282748,
58.9675890563221));
#43208=CARTESIAN_POINT('Ctrl Pts',(0.595222041631902,-1.01747520944581,
58.9913644216192));
#43209=CARTESIAN_POINT('Ctrl Pts',(1.00891253001624,-0.609623316038242,
59.0151397869164));
#43210=CARTESIAN_POINT('Ctrl Pts',(1.1775654020451,-0.0537103769081715,
59.0389151522136));
#43211=CARTESIAN_POINT('Ctrl Pts',(1.060219428153,0.51524736277654,59.0626905175107));
#43212=CARTESIAN_POINT('Ctrl Pts',(0.685374777458641,0.959065427958262,
59.0864658828078));
#43213=CARTESIAN_POINT('Ctrl Pts',(0.144071096092974,1.16995239217321,59.110241248105));
#43214=CARTESIAN_POINT('Ctrl Pts',(-0.432223565087148,1.09668950503987,
59.1340166134021));
#43215=CARTESIAN_POINT('Ctrl Pts',(-0.903542790864627,0.757070343995723,
59.1577919786993));
#43216=CARTESIAN_POINT('Ctrl Pts',(-1.15541586530421,0.233579234703329,
59.1815673439965));
#43217=CARTESIAN_POINT('Ctrl Pts',(-1.12666961833547,-0.346641964858551,
59.2053427092936));
#43218=CARTESIAN_POINT('Ctrl Pts',(-0.82428573729697,-0.842673189303012,
59.2291180745908));
#43219=CARTESIAN_POINT('Ctrl Pts',(-0.321705103562753,-1.13404184535795,
59.2528934398879));
#43220=CARTESIAN_POINT('Ctrl Pts',(0.259009014889653,-1.14998235242418,
59.2766688051851));
#43221=CARTESIAN_POINT('Ctrl Pts',(0.776816835983212,-0.886623191674403,
59.3004441704823));
#43222=CARTESIAN_POINT('Ctrl Pts',(1.10595681901059,-0.407927193458844,
59.3242195357794));
#43223=CARTESIAN_POINT('Ctrl Pts',(1.16648974775348,0.16984330740993,59.3479949010765));
#43224=CARTESIAN_POINT('Ctrl Pts',(0.94371380798938,0.706363454096405,59.3717702663737));
#43225=CARTESIAN_POINT('Ctrl Pts',(0.491735261326532,1.0713269871797,59.3955456316708));
#43226=CARTESIAN_POINT('Ctrl Pts',(-0.0796725051838685,1.17609411723707,
59.419320996968));
#43227=CARTESIAN_POINT('Ctrl Pts',(-0.631729970982799,0.995219736738363,
59.4430963622652));
#43228=CARTESIAN_POINT('Ctrl Pts',(-1.03035728156532,0.572633349702764,
59.4668717275623));
#43229=CARTESIAN_POINT('Ctrl Pts',(-1.17873862417058,0.0109697811866665,
59.4906470928595));
#43230=CARTESIAN_POINT('Ctrl Pts',(-1.04083617774728,-0.553358051079711,
59.5144224581566));
#43231=CARTESIAN_POINT('Ctrl Pts',(-0.650142720880909,-0.983290151411998,
59.5381978234538));
#43232=CARTESIAN_POINT('Ctrl Pts',(-0.101547152799094,-1.17440761965159,
59.5619731887509));
#43233=CARTESIAN_POINT('Ctrl Pts',(0.471711486017707,-1.08029318159782,
59.5857485540481));
#43234=CARTESIAN_POINT('Ctrl Pts',(0.93040412062756,-0.723804694957189,
59.6095239193452));
#43235=CARTESIAN_POINT('Ctrl Pts',(1.16312675268372,-0.191523585992356,
59.6332992846424));
#43236=CARTESIAN_POINT('Ctrl Pts',(1.11335720939914,0.387273426872361,59.6570746499396));
#43237=CARTESIAN_POINT('Ctrl Pts',(0.793183445420126,0.872012189522576,
59.6808500152367));
#43238=CARTESIAN_POINT('Ctrl Pts',(0.280366428967129,1.14496271124877,59.7046253805339));
#43239=CARTESIAN_POINT('Ctrl Pts',(-0.300543148672945,1.13983274835279,
59.728400745831));
#43240=CARTESIAN_POINT('Ctrl Pts',(-0.808460801791496,0.857868086924541,
59.7521761111282));
#43241=CARTESIAN_POINT('Ctrl Pts',(-1.12002109956608,0.367550667285518,
59.7759514764253));
#43242=CARTESIAN_POINT('Ctrl Pts',(-1.15956736401967,-0.212035247289841,
59.7997268417224));
#43243=CARTESIAN_POINT('Ctrl Pts',(-0.917467489156749,-0.740122028302085,
59.8235022070197));
#43244=CARTESIAN_POINT('Ctrl Pts',(-0.452582019722852,-1.0884530823275,
59.8472775723168));
#43245=CARTESIAN_POINT('Ctrl Pts',(0.122304101199269,-1.17241375087369,
59.871052937614));
#43246=CARTESIAN_POINT('Ctrl Pts',(0.485598392798923,-1.03852712465534,
59.8869031811454));
#43247=CARTESIAN_POINT('Ctrl Pts',(0.64033508002711,-0.932242155189131,
59.8948283029111));
#43248=CARTESIAN_POINT('Ctrl Pts',(0.623398732068366,-0.874219306856439,
56.0287216970889));
#43249=CARTESIAN_POINT('Ctrl Pts',(0.768504591850525,-0.770745489366451,
56.0366468188546));
#43250=CARTESIAN_POINT('Ctrl Pts',(1.00602699863118,-0.490212309141386,
56.0524970623861));
#43251=CARTESIAN_POINT('Ctrl Pts',(1.11801361188198,0.0498751246670368,
56.0762724276832));
#43252=CARTESIAN_POINT('Ctrl Pts',(0.958425720631955,0.577781974785802,
56.1000477929803));
#43253=CARTESIAN_POINT('Ctrl Pts',(0.566075848520809,0.965399103995967,
56.1238231582775));
#43254=CARTESIAN_POINT('Ctrl Pts',(0.0362340764180832,1.11853081022668,
56.1475985235747));
#43255=CARTESIAN_POINT('Ctrl Pts',(-0.502404774606105,1.00000936060083,
56.1713738888718));
#43256=CARTESIAN_POINT('Ctrl Pts',(-0.919024600976301,0.638609097738095,
56.195149254169));
#43257=CARTESIAN_POINT('Ctrl Pts',(-1.11243746181925,0.122109582471567,
56.2189246194661));
#43258=CARTESIAN_POINT('Ctrl Pts',(-1.03566962247792,-0.424047819194122,
56.2426999847633));
#43259=CARTESIAN_POINT('Ctrl Pts',(-0.707365440007877,-0.867215097504543,
56.2664753500605));
#43260=CARTESIAN_POINT('Ctrl Pts',(-0.207261358948599,-1.0997594054429,
56.2902507153576));
#43261=CARTESIAN_POINT('Ctrl Pts',(0.343180943467093,-1.06520176695407,
56.3140260806547));
#43262=CARTESIAN_POINT('Ctrl Pts',(0.81027384428683,-0.771935411601755,
56.3378014459519));
#43263=CARTESIAN_POINT('Ctrl Pts',(1.08057310997332,-0.291186767898998,
56.3615768112491));
#43264=CARTESIAN_POINT('Ctrl Pts',(1.08843033576408,0.260283273030794,56.3853521765462));
#43265=CARTESIAN_POINT('Ctrl Pts',(0.83193721840397,0.748537537248444,56.4091275418434));
#43266=CARTESIAN_POINT('Ctrl Pts',(0.373389009449589,1.05499223997325,56.4329029071405));
#43267=CARTESIAN_POINT('Ctrl Pts',(-0.175845309349143,1.10521780955267,
56.4566782724377));
#43268=CARTESIAN_POINT('Ctrl Pts',(-0.682371549879583,0.887015809935557,
56.4804536377348));
#43269=CARTESIAN_POINT('Ctrl Pts',(-1.0231681625707,0.45338161664081,56.504229003032));
#43270=CARTESIAN_POINT('Ctrl Pts',(-1.11546485064466,-0.0903667316603153,
56.5280043683291));
#43271=CARTESIAN_POINT('Ctrl Pts',(-0.936845240215391,-0.612167440398215,
56.5517797336263));
#43272=CARTESIAN_POINT('Ctrl Pts',(-0.530691212560068,-0.985289204305658,
56.5755550989234));
#43273=CARTESIAN_POINT('Ctrl Pts',(0.00435338378282068,-1.11911081991613,
56.5993304642206));
#43274=CARTESIAN_POINT('Ctrl Pts',(0.538340660729817,-0.98113062953466,
56.6231058295177));
#43275=CARTESIAN_POINT('Ctrl Pts',(0.941579524541688,-0.60486029640679,
56.6468811948149));
#43276=CARTESIAN_POINT('Ctrl Pts',(1.1161341412668,-0.0816857264404262,
56.6706565601121));
#43277=CARTESIAN_POINT('Ctrl Pts',(1.01960990688035,0.461328101243613,56.6944319254092));
#43278=CARTESIAN_POINT('Ctrl Pts',(0.675449952090617,0.892297787415319,
56.7182072907064));
#43279=CARTESIAN_POINT('Ctrl Pts',(0.167241438775177,1.10655243001042,56.7419826560035));
#43280=CARTESIAN_POINT('Ctrl Pts',(-0.381585505072281,1.05205536048454,
56.7657580213007));
#43281=CARTESIAN_POINT('Ctrl Pts',(-0.837735631240389,0.742042445791208,
56.7895333865978));
#43282=CARTESIAN_POINT('Ctrl Pts',(-1.09042238857522,0.251807453621685,
56.813308751895));
#43283=CARTESIAN_POINT('Ctrl Pts',(-1.07827498539781,-0.299584771093069,
56.8370841171922));
#43284=CARTESIAN_POINT('Ctrl Pts',(-0.804243698001629,-0.778215942672852,
56.8608594824893));
#43285=CARTESIAN_POINT('Ctrl Pts',(-0.334883328188288,-1.06783947094452,
56.8846348477864));
#43286=CARTESIAN_POINT('Ctrl Pts',(0.215811161338217,-1.09811361973494,
56.9084102130836));
#43287=CARTESIAN_POINT('Ctrl Pts',(0.714090945938441,-0.861685615601347,
56.9321855783807));
#43288=CARTESIAN_POINT('Ctrl Pts',(1.03893731778188,-0.415977438000807,
56.9559609436779));
#43289=CARTESIAN_POINT('Ctrl Pts',(1.11145386288807,0.130760429322928,56.979736308975));
#43290=CARTESIAN_POINT('Ctrl Pts',(0.914028270149248,0.645740118448208,
57.0035116742722));
#43291=CARTESIAN_POINT('Ctrl Pts',(0.494609886226332,1.00388696557566,57.0272870395693));
#43292=CARTESIAN_POINT('Ctrl Pts',(-0.0449358862867625,1.11821677027719,
57.0510624048665));
#43293=CARTESIAN_POINT('Ctrl Pts',(-0.573567945135943,0.960961909504253,
57.0748377701637));
#43294=CARTESIAN_POINT('Ctrl Pts',(-0.962895834483168,0.570315343595536,
57.0986131354608));
#43295=CARTESIAN_POINT('Ctrl Pts',(-1.11836232052659,0.0411545772899142,
57.122388500758));
#43296=CARTESIAN_POINT('Ctrl Pts',(-1.00220879086932,-0.498001524806689,
57.1461638660551));
#43297=CARTESIAN_POINT('Ctrl Pts',(-0.642645802117325,-0.916206500864576,
57.1699392313523));
#43298=CARTESIAN_POINT('Ctrl Pts',(-0.127001497268327,-1.11188965230239,
57.1937145966494));
#43299=CARTESIAN_POINT('Ctrl Pts',(0.419488042661364,-1.03752482441128,
57.2174899619466));
#43300=CARTESIAN_POINT('Ctrl Pts',(0.864095261770125,-0.711173226290157,
57.2412653272438));
#43301=CARTESIAN_POINT('Ctrl Pts',(1.09883706940975,-0.212096850746369,
57.2650406925409));
#43302=CARTESIAN_POINT('Ctrl Pts',(1.06670101773,0.338492123954616,57.2888160578381));
#43303=CARTESIAN_POINT('Ctrl Pts',(0.775492086120482,0.80687049987593,57.3125914231352));
#43304=CARTESIAN_POINT('Ctrl Pts',(0.295937062424609,1.07928181411947,57.3363667884324));
#43305=CARTESIAN_POINT('Ctrl Pts',(-0.255493084446318,1.08956471262869,
57.3601421537295));
#43306=CARTESIAN_POINT('Ctrl Pts',(-0.744870858544122,0.835221756958756,
57.3839175190267));
#43307=CARTESIAN_POINT('Ctrl Pts',(-1.05333961006553,0.378025984652554,
57.4076928843238));
#43308=CARTESIAN_POINT('Ctrl Pts',(-1.10598060686658,-0.17098209391791,
57.431468249621));
#43309=CARTESIAN_POINT('Ctrl Pts',(-0.890008771951069,-0.678463237807091,
57.4552436149181));
#43310=CARTESIAN_POINT('Ctrl Pts',(-0.457877833519551,-1.0211639774184,
57.4790189802153));
#43311=CARTESIAN_POINT('Ctrl Pts',(0.0854592695393839,-1.11585155484739,
57.5027943455124));
#43312=CARTESIAN_POINT('Ctrl Pts',(0.608040623135005,-0.939528913777072,
57.5265697108096));
#43313=CARTESIAN_POINT('Ctrl Pts',(0.982945324387024,-0.535020063615578,
57.5503450761068));
#43314=CARTESIAN_POINT('Ctrl Pts',(1.1191191425052,-0.000569283712549584,
57.5741204414039));
#43315=CARTESIAN_POINT('Ctrl Pts',(0.983489133295694,0.534019759835548,
57.5978958067011));
#43316=CARTESIAN_POINT('Ctrl Pts',(0.608996164449402,0.938909820425502,
57.6216711719982));
#43317=CARTESIAN_POINT('Ctrl Pts',(0.0865944680705869,1.11576403298596,
57.6454465372954));
#43318=CARTESIAN_POINT('Ctrl Pts',(-0.456838686848294,1.02162928374448,
57.6692219025925));
#43319=CARTESIAN_POINT('Ctrl Pts',(-0.889318057812799,0.67936836197574,
57.6929972678897));
#43320=CARTESIAN_POINT('Ctrl Pts',(-1.10580608107857,0.172107205703827,
57.7167726331868));
#43321=CARTESIAN_POINT('Ctrl Pts',(-1.05372366023009,-0.376954144528003,
57.740547998484));
#43322=CARTESIAN_POINT('Ctrl Pts',(-0.74572020924432,-0.834463509525814,
57.7643233637811));
#43323=CARTESIAN_POINT('Ctrl Pts',(-0.256601451326632,-1.08930421571873,
57.7880987290783));
#43324=CARTESIAN_POINT('Ctrl Pts',(0.294838871757291,-1.0795823353994,57.8118740943754));
#43325=CARTESIAN_POINT('Ctrl Pts',(0.774670792531859,-0.80765905083989,
57.8356494596726));
#43326=CARTESIAN_POINT('Ctrl Pts',(1.06635609126063,-0.339577186861649,
57.8594248249698));
#43327=CARTESIAN_POINT('Ctrl Pts',(1.09905228338722,0.210978808383394,57.8832001902669));
#43328=CARTESIAN_POINT('Ctrl Pts',(0.864818346529344,0.710293746777896,
57.9069755555641));
#43329=CARTESIAN_POINT('Ctrl Pts',(0.420543380435131,1.03709750958033,57.9307509208612));
#43330=CARTESIAN_POINT('Ctrl Pts',(-0.125870219534756,1.11201828538914,
57.9545262861584));
#43331=CARTESIAN_POINT('Ctrl Pts',(-0.641713341244805,0.916859840364906,
57.9783016514555));
#43332=CARTESIAN_POINT('Ctrl Pts',(-1.00170161643053,0.4990208921939,58.0020770167527));
#43333=CARTESIAN_POINT('Ctrl Pts',(-1.11840361150074,-0.0400167588347418,
58.0258523820498));
#43334=CARTESIAN_POINT('Ctrl Pts',(-0.96347556240735,-0.569335419457958,
58.049627747347));
#43335=CARTESIAN_POINT('Ctrl Pts',(-0.574545309748047,-0.960377876802694,
58.0734031126442));
#43336=CARTESIAN_POINT('Ctrl Pts',(-0.0460735121080044,-1.11817047478798,
58.0971784779413));
#43337=CARTESIAN_POINT('Ctrl Pts',(0.493588297795928,-1.00438965122329,
58.1209538432384));
#43338=CARTESIAN_POINT('Ctrl Pts',(0.913370835360033,-0.646669696459674,
58.1447292085356));
#43339=CARTESIAN_POINT('Ctrl Pts',(1.11132025490185,-0.13189113029467,58.1685045738328));
#43340=CARTESIAN_POINT('Ctrl Pts',(1.03935998637156,0.414920230809768,58.1922799391299));
#43341=CARTESIAN_POINT('Ctrl Pts',(0.714967236314193,0.86095866927674,58.2160553044271));
#43342=CARTESIAN_POINT('Ctrl Pts',(0.216928246224609,1.09789348991396,58.2398306697243));
#43343=CARTESIAN_POINT('Ctrl Pts',(-0.333796758552693,1.06817962121791,
58.2636060350214));
#43344=CARTESIAN_POINT('Ctrl Pts',(-0.803451542047654,0.779033759722117,
58.2873814003185));
#43345=CARTESIAN_POINT('Ctrl Pts',(-1.07796963642117,0.300681629235197,
58.3111567656157));
#43346=CARTESIAN_POINT('Ctrl Pts',(-1.09067800759897,-0.250697951618005,
58.3349321309128));
#43347=CARTESIAN_POINT('Ctrl Pts',(-0.838490135304495,-0.741189768009906,
58.35870749621));
#43348=CARTESIAN_POINT('Ctrl Pts',(-0.382655645508598,-1.05166659933932,
58.3824828615072));
#43349=CARTESIAN_POINT('Ctrl Pts',(0.166115570188494,-1.10672200508822,
58.4062582268043));
#43350=CARTESIAN_POINT('Ctrl Pts',(0.674541798438691,-0.892984513507725,
58.4300335921015));
#43351=CARTESIAN_POINT('Ctrl Pts',(1.01914003416817,-0.462365191121956,
58.4538089573986));
#43352=CARTESIAN_POINT('Ctrl Pts',(1.11621666889125,0.0805501539095563,
58.4775843226958));
#43353=CARTESIAN_POINT('Ctrl Pts',(0.942194408770615,0.603902041134919,
58.5013596879929));
#43354=CARTESIAN_POINT('Ctrl Pts',(0.53933856278411,0.980582425856949,58.5251350532901));
#43355=CARTESIAN_POINT('Ctrl Pts',(0.00549194019273262,1.11910581170792,
58.5489104185872));
#43356=CARTESIAN_POINT('Ctrl Pts',(-0.529688526407874,0.985828607921979,
58.5726857838844));
#43357=CARTESIAN_POINT('Ctrl Pts',(-0.936221949721437,0.613120249270339,
58.5964611491816));
#43358=CARTESIAN_POINT('Ctrl Pts',(-1.11537233623622,0.0915015342193444,
58.6202365144787));
#43359=CARTESIAN_POINT('Ctrl Pts',(-1.02362889351509,-0.452340433265256,
58.6440118797759));
#43360=CARTESIAN_POINT('Ctrl Pts',(-0.683273627036049,-0.886321121153351,
58.667787245073));
#43361=CARTESIAN_POINT('Ctrl Pts',(-0.176969642599475,-1.10503833635026,
58.6915626103702));
#43362=CARTESIAN_POINT('Ctrl Pts',(0.372315490449813,-1.05537157190093,
58.7153379756673));
#43363=CARTESIAN_POINT('Ctrl Pts',(0.831175242112888,-0.749383544057456,
58.7391133409645));
#43364=CARTESIAN_POINT('Ctrl Pts',(1.0881649663537,-0.261390484153449,58.7628887062616));
#43365=CARTESIAN_POINT('Ctrl Pts',(1.0808687969972,0.290087267702929,58.7866640715588));
#43366=CARTESIAN_POINT('Ctrl Pts',(0.811058776608478,0.771110653597713,
58.8104394368559));
#43367=CARTESIAN_POINT('Ctrl Pts',(0.344264475192786,1.06485207908224,58.8342148021531));
#43368=CARTESIAN_POINT('Ctrl Pts',(-0.206142373284595,1.09996968191952,
58.8579901674502));
#43369=CARTESIAN_POINT('Ctrl Pts',(-0.706482804429733,0.867934344435469,
58.8817655327474));
#43370=CARTESIAN_POINT('Ctrl Pts',(-1.03523763499677,0.425101185944966,
58.9055408980446));
#43371=CARTESIAN_POINT('Ctrl Pts',(-1.11256119189629,-0.120977574334403,
58.9293162633417));
#43372=CARTESIAN_POINT('Ctrl Pts',(-0.919673670628794,-0.637674147788424,
58.9530916286389));
#43373=CARTESIAN_POINT('Ctrl Pts',(-0.503422242807215,-0.999496885764276,
58.976866993936));
#43374=CARTESIAN_POINT('Ctrl Pts',(0.0350968571145739,-1.11856881318326,
59.0006423592332));
#43375=CARTESIAN_POINT('Ctrl Pts',(0.565091877938255,-0.965970573409845,
59.0244177245303));
#43376=CARTESIAN_POINT('Ctrl Pts',(0.957841337157492,-0.578764159254765,
59.0481930898275));
#43377=CARTESIAN_POINT('Ctrl Pts',(1.11795699401921,-0.050991555468266,
59.0719684551247));
#43378=CARTESIAN_POINT('Ctrl Pts',(1.00655107804644,0.489165520543995,59.0957438204218));
#43379=CARTESIAN_POINT('Ctrl Pts',(0.650681078650523,0.910517497411072,
59.119519185719));
#43380=CARTESIAN_POINT('Ctrl Pts',(0.136778211412653,1.11072935501331,59.1432945510161));
#43381=CARTESIAN_POINT('Ctrl Pts',(-0.410344390833752,1.04117503817409,
59.1670699163132));
#43382=CARTESIAN_POINT('Ctrl Pts',(-0.857805418440835,0.71874741272513,
59.1908452816104));
#43383=CARTESIAN_POINT('Ctrl Pts',(-1.09692866771924,0.221755444445569,
59.2146206469076));
#43384=CARTESIAN_POINT('Ctrl Pts',(-1.06963755692854,-0.32909493465174,
59.2383960122047));
#43385=CARTESIAN_POINT('Ctrl Pts',(-0.782560360113341,-0.800017038559101,
59.2621713775019));
#43386=CARTESIAN_POINT('Ctrl Pts',(-0.305420378277957,-1.07663660152255,
59.2859467427991));
#43387=CARTESIAN_POINT('Ctrl Pts',(0.245897968135809,-1.09177019947979,
59.3097221080962));
#43388=CARTESIAN_POINT('Ctrl Pts',(0.737494336493802,-0.841742290042304,
59.3334974733934));
#43389=CARTESIAN_POINT('Ctrl Pts',(1.04997324033878,-0.387277902514728,
59.3572728386905));
#43390=CARTESIAN_POINT('Ctrl Pts',(1.10744198979342,0.161245832355916,59.3810482039877));
#43391=CARTESIAN_POINT('Ctrl Pts',(0.895942977062618,0.670607307632499,
59.4048235692848));
#43392=CARTESIAN_POINT('Ctrl Pts',(0.466843602615289,1.01709637198835,59.428598934582));
#43393=CARTESIAN_POINT('Ctrl Pts',(-0.0756394797661783,1.11656018570735,
59.4523742998791));
#43394=CARTESIAN_POINT('Ctrl Pts',(-0.599751774436666,0.944841673626204,
59.4761496651763));
#43395=CARTESIAN_POINT('Ctrl Pts',(-0.978200554520414,0.543646626503323,
59.4999250304734));
#43396=CARTESIAN_POINT('Ctrl Pts',(-1.1190708275935,0.0104144904216708,
59.5237003957706));
#43397=CARTESIAN_POINT('Ctrl Pts',(-0.988149008556066,-0.525347044272036,
59.5474757610677));
#43398=CARTESIAN_POINT('Ctrl Pts',(-0.617232470194169,-0.933515964389,59.5712511263649));
#43399=CARTESIAN_POINT('Ctrl Pts',(-0.0964068318390796,-1.1149590586975,
59.595026491662));
#43400=CARTESIAN_POINT('Ctrl Pts',(0.447833431618176,-1.02560869728431,
59.6188018569592));
#43401=CARTESIAN_POINT('Ctrl Pts',(0.883307026610518,-0.68716567217923,
59.6425772222563));
#43402=CARTESIAN_POINT('Ctrl Pts',(1.10424922966938,-0.181828654364277,
59.6663525875535));
#43403=CARTESIAN_POINT('Ctrl Pts',(1.05699902266814,0.367669630423775,59.6901279528507));
#43404=CARTESIAN_POINT('Ctrl Pts',(0.753032467502573,0.827870897407221,
59.7139033181478));
#43405=CARTESIAN_POINT('Ctrl Pts',(0.266174269053451,1.08700465274262,59.737678683445));
#43406=CARTESIAN_POINT('Ctrl Pts',(-0.285329642396041,1.08213436877481,
59.7614540487421));
#43407=CARTESIAN_POINT('Ctrl Pts',(-0.76753648347981,0.814442769851721,
59.7852294140393));
#43408=CARTESIAN_POINT('Ctrl Pts',(-1.06332558644673,0.348945237720674,
59.8090047793364));
#43409=CARTESIAN_POINT('Ctrl Pts',(-1.1008700174027,-0.201302014541691,
59.8327801446336));
#43410=CARTESIAN_POINT('Ctrl Pts',(-0.871025247945204,-0.702657021453754,
59.8565555099308));
#43411=CARTESIAN_POINT('Ctrl Pts',(-0.429672299676753,-1.03335554351077,
59.8803308752279));
#43412=CARTESIAN_POINT('Ctrl Pts',(0.116113062676177,-1.11306611963735,
59.904106240525));
#43413=CARTESIAN_POINT('Ctrl Pts',(0.461017382619445,-0.985956839824536,
59.9199564840565));
#43414=CARTESIAN_POINT('Ctrl Pts',(0.607921292514964,-0.885052019788631,
59.9278816058222));
#43415=CARTESIAN_POINT('Ctrl Pts',(0.590159702138998,-0.827606761449064,
56.061775));
#43416=CARTESIAN_POINT('Ctrl Pts',(0.727528654917474,-0.729650069900356,
56.0697001217657));
#43417=CARTESIAN_POINT('Ctrl Pts',(0.952386591942655,-0.464074653132307,
56.0855503652972));
#43418=CARTESIAN_POINT('Ctrl Pts',(1.05840218504528,0.0472158302600112,
56.1093257305943));
#43419=CARTESIAN_POINT('Ctrl Pts',(0.907323368999851,0.546975187147921,
56.1331010958915));
#43420=CARTESIAN_POINT('Ctrl Pts',(0.535893220447681,0.913924938167876,
56.1568764611886));
#43421=CARTESIAN_POINT('Ctrl Pts',(0.0343021097832936,1.05889180686411,
56.1806518264858));
#43422=CARTESIAN_POINT('Ctrl Pts',(-0.475617027886791,0.946689808672358,
56.2044271917829));
#43423=CARTESIAN_POINT('Ctrl Pts',(-0.870023079724685,0.604559065518011,
56.22820255708));
#43424=CARTESIAN_POINT('Ctrl Pts',(-1.05312335002233,0.1155988151927,56.2519779223772));
#43425=CARTESIAN_POINT('Ctrl Pts',(-0.980448699162488,-0.401437991120026,
56.2757532876744));
#43426=CARTESIAN_POINT('Ctrl Pts',(-0.669649384741906,-0.820976009905639,
56.2995286529715));
#43427=CARTESIAN_POINT('Ctrl Pts',(-0.196210379601176,-1.04112127560369,
56.3233040182687));
#43428=CARTESIAN_POINT('Ctrl Pts',(0.324882860612091,-1.00840621766713,
56.3470793835659));
#43429=CARTESIAN_POINT('Ctrl Pts',(0.767070810376454,-0.730776546609132,
56.370854748863));
#43430=CARTESIAN_POINT('Ctrl Pts',(1.02295797523586,-0.275660965237961,
56.3946301141602));
#43431=CARTESIAN_POINT('Ctrl Pts',(1.03039626118959,0.246405215445278,56.4184054794573));
#43432=CARTESIAN_POINT('Ctrl Pts',(0.787579113904559,0.708626224754583,
56.4421808447545));
#43433=CARTESIAN_POINT('Ctrl Pts',(0.353480261128564,0.998741052994776,
56.4659562100516));
#43434=CARTESIAN_POINT('Ctrl Pts',(-0.166469404010035,1.04628864277636,
56.4897315753488));
#43435=CARTESIAN_POINT('Ctrl Pts',(-0.645988145161798,0.839720967104466,
56.5135069406459));
#43436=CARTESIAN_POINT('Ctrl Pts',(-0.968613805256519,0.429207738270938,
56.5372823059431));
#43437=CARTESIAN_POINT('Ctrl Pts',(-1.05598932134302,-0.0855484631208394,
56.5610576712402));
#43438=CARTESIAN_POINT('Ctrl Pts',(-0.886893539358715,-0.579527252302758,
56.5848330365374));
#43439=CARTESIAN_POINT('Ctrl Pts',(-0.502395259761104,-0.932754517168359,
56.6086084018346));
#43440=CARTESIAN_POINT('Ctrl Pts',(0.00412126548291853,-1.05944089098629,
56.6323837671317));
#43441=CARTESIAN_POINT('Ctrl Pts',(0.509636846599777,-0.928817673665269,
56.6561591324289));
#43442=CARTESIAN_POINT('Ctrl Pts',(0.89137539612891,-0.572609718307843,
56.679934497726));
#43443=CARTESIAN_POINT('Ctrl Pts',(1.05662292602311,-0.0773303208768799,
56.7037098630232));
#43444=CARTESIAN_POINT('Ctrl Pts',(0.965245272389302,0.436730523841399,
56.7274852283203));
#43445=CARTESIAN_POINT('Ctrl Pts',(0.639435600411005,0.844721314547941,
56.7512605936175));
#43446=CARTESIAN_POINT('Ctrl Pts',(0.158324283665738,1.04755210253542,56.7750359589146));
#43447=CARTESIAN_POINT('Ctrl Pts',(-0.361239727368135,0.995960765138673,
56.7988113242118));
#43448=CARTESIAN_POINT('Ctrl Pts',(-0.793068360860628,0.702477445421887,
56.8225866895089));
#43449=CARTESIAN_POINT('Ctrl Pts',(-1.03228209963166,0.238381318699013,
56.8463620548061));
#43450=CARTESIAN_POINT('Ctrl Pts',(-1.02078238448601,-0.283611194856068,
56.8701374201032));
#43451=CARTESIAN_POINT('Ctrl Pts',(-0.761362185779602,-0.736722205712254,
56.8939127854004));
#43452=CARTESIAN_POINT('Ctrl Pts',(-0.317027666320693,-1.01090328177916,
56.9176881506975));
#43453=CARTESIAN_POINT('Ctrl Pts',(0.204304314625503,-1.03956324163084,
56.9414635159947));
#43454=CARTESIAN_POINT('Ctrl Pts',(0.676016293066456,-0.815741354740158,
56.9652388812919));
#43455=CARTESIAN_POINT('Ctrl Pts',(0.98354216404791,-0.393797915007909,
56.989014246589));
#43456=CARTESIAN_POINT('Ctrl Pts',(1.05219219565452,0.123788407083776,57.0127896118862));
#43457=CARTESIAN_POINT('Ctrl Pts',(0.865293148524952,0.611309866958155,
57.0365649771833));
#43458=CARTESIAN_POINT('Ctrl Pts',(0.468237755572337,0.950360663422683,
57.0603403424805));
#43459=CARTESIAN_POINT('Ctrl Pts',(-0.0425399473918753,1.05859451122728,
57.0841157077776));
#43460=CARTESIAN_POINT('Ctrl Pts',(-0.54298584556759,0.90972433068368,57.1078910730748));
#43461=CARTESIAN_POINT('Ctrl Pts',(-0.911555140614478,0.539906669660545,
57.1316664383719));
#43462=CARTESIAN_POINT('Ctrl Pts',(-1.05873230087524,0.0389602542091891,
57.1554418036691));
#43463=CARTESIAN_POINT('Ctrl Pts',(-0.948771967402165,-0.471448555196054,
57.1792171689663));
#43464=CARTESIAN_POINT('Ctrl Pts',(-0.608380536643186,-0.867355238041698,
57.2029925342634));
#43465=CARTESIAN_POINT('Ctrl Pts',(-0.120229897725971,-1.05260474919004,
57.2267678995606));
#43466=CARTESIAN_POINT('Ctrl Pts',(0.397121337553111,-0.982204983485956,
57.2505432648577));
#43467=CARTESIAN_POINT('Ctrl Pts',(0.818022520857566,-0.673254143466235,
57.2743186301549));
#43468=CARTESIAN_POINT('Ctrl Pts',(1.04024811765422,-0.200788047556321,
57.298093995452));
#43469=CARTESIAN_POINT('Ctrl Pts',(1.00982552981173,0.320444044514911,57.3218693607492));
#43470=CARTESIAN_POINT('Ctrl Pts',(0.734143582611297,0.763848929065998,
57.3456447260463));
#43471=CARTESIAN_POINT('Ctrl Pts',(0.280157978558803,1.02173553005387,57.3694200913435));
#43472=CARTESIAN_POINT('Ctrl Pts',(-0.241870435179003,1.03147015415423,
57.3931954566406));
#43473=CARTESIAN_POINT('Ctrl Pts',(-0.705155049885808,0.79068852397462,
57.4169708219378));
#43474=CARTESIAN_POINT('Ctrl Pts',(-0.997176539748407,0.35786999720571,
57.440746187235));
#43475=CARTESIAN_POINT('Ctrl Pts',(-1.04701076846,-0.161865490619304,57.4645215525321));
#43476=CARTESIAN_POINT('Ctrl Pts',(-0.842554347220154,-0.642288220587176,
57.4882969178293));
#43477=CARTESIAN_POINT('Ctrl Pts',(-0.433464221124387,-0.966716481358237,
57.5120722831264));
#43478=CARTESIAN_POINT('Ctrl Pts',(0.0809026622319955,-1.05635540684393,
57.5358476484236));
#43479=CARTESIAN_POINT('Ctrl Pts',(0.575620473027226,-0.889434121987983,
57.5596230137207));
#43480=CARTESIAN_POINT('Ctrl Pts',(0.930535610706933,-0.506493300578492,
57.5833983790179));
#43481=CARTESIAN_POINT('Ctrl Pts',(1.05944876982279,-0.000538930044200919,
57.607173744315));
#43482=CARTESIAN_POINT('Ctrl Pts',(0.931050424239669,0.505546332048563,
57.6309491096122));
#43483=CARTESIAN_POINT('Ctrl Pts',(0.576525065783793,0.888848038107536,
57.6547244749094));
#43484=CARTESIAN_POINT('Ctrl Pts',(0.0819773330527327,1.05627255156526,
57.6784998402065));
#43485=CARTESIAN_POINT('Ctrl Pts',(-0.432480480769399,0.967156977991728,
57.7022752055036));
#43486=CARTESIAN_POINT('Ctrl Pts',(-0.841900461305519,0.643145084392453,
57.7260505708008));
#43487=CARTESIAN_POINT('Ctrl Pts',(-1.0468455482217,0.16293061251046,57.7498259360979));
#43488=CARTESIAN_POINT('Ctrl Pts',(-0.99754011272195,-0.356855306581392,
57.7736013013951));
#43489=CARTESIAN_POINT('Ctrl Pts',(-0.705959114011145,-0.789970705576619,
57.7973766666922));
#43490=CARTESIAN_POINT('Ctrl Pts',(-0.242919704987064,-1.03122354669277,
57.8211520319894));
#43491=CARTESIAN_POINT('Ctrl Pts',(0.2791183423777,-1.02202002782379,57.8449273972865));
#43492=CARTESIAN_POINT('Ctrl Pts',(0.73336607961892,-0.764595435239446,
57.8687027625837));
#43493=CARTESIAN_POINT('Ctrl Pts',(1.00949899449501,-0.321471252895473,
57.8924781278809));
#43494=CARTESIAN_POINT('Ctrl Pts',(1.04045185662625,0.199729618153172,57.916253493178));
#43495=CARTESIAN_POINT('Ctrl Pts',(0.818707051422304,0.672421556968558,
57.9400288584752));
#43496=CARTESIAN_POINT('Ctrl Pts',(0.398120405716357,0.981800452677053,
57.9638042237723));
#43497=CARTESIAN_POINT('Ctrl Pts',(-0.11915893864965,1.05272652368244,57.9875795890695));
#43498=CARTESIAN_POINT('Ctrl Pts',(-0.607497793701196,0.867973742098689,
58.0113549543666));
#43499=CARTESIAN_POINT('Ctrl Pts',(-0.948291835024074,0.472413570879686,
58.0351303196638));
#43500=CARTESIAN_POINT('Ctrl Pts',(-1.05877139025375,-0.0378831031563466,
58.058905684961));
#43501=CARTESIAN_POINT('Ctrl Pts',(-0.912103957994839,-0.538978994149835,
58.0826810502581));
#43502=CARTESIAN_POINT('Ctrl Pts',(-0.543911098024301,-0.909171438052593,
58.1064564155553));
#43503=CARTESIAN_POINT('Ctrl Pts',(-0.0436169160818455,-1.0585506841697,
58.1302317808524));
#43504=CARTESIAN_POINT('Ctrl Pts',(0.467270637269431,-0.950836546347711,
58.1540071461496));
#43505=CARTESIAN_POINT('Ctrl Pts',(0.864670767536001,-0.612189880750512,
58.1777825114467));
#43506=CARTESIAN_POINT('Ctrl Pts',(1.05206571151958,-0.124858820150662,
58.2015578767439));
#43507=CARTESIAN_POINT('Ctrl Pts',(0.983942296348724,0.392797077102948,
58.2253332420411));
#43508=CARTESIAN_POINT('Ctrl Pts',(0.676845860469362,0.815053168505043,
58.2491086073382));
#43509=CARTESIAN_POINT('Ctrl Pts',(0.205361837603814,1.03935484892341,58.2728839726354));
#43510=CARTESIAN_POINT('Ctrl Pts',(-0.315999031548909,1.01122529556216,
58.2966593379325));
#43511=CARTESIAN_POINT('Ctrl Pts',(-0.760612266830792,0.737496417531059,
58.3204347032296));
#43512=CARTESIAN_POINT('Ctrl Pts',(-1.02049331642759,0.28464956956096,58.3442100685268));
#43513=CARTESIAN_POINT('Ctrl Pts',(-1.03252408929118,-0.237330974291291,
58.367985433824));
#43514=CARTESIAN_POINT('Ctrl Pts',(-0.793782635482674,-0.701670231612259,
58.3917607991211));
#43515=CARTESIAN_POINT('Ctrl Pts',(-0.362252808929985,-0.995592732369494,
58.4155361644183));
#43516=CARTESIAN_POINT('Ctrl Pts',(0.157258445325715,-1.04771263603068,
58.4393115297154));
#43517=CARTESIAN_POINT('Ctrl Pts',(0.63857586865163,-0.845371425055543,
58.4630868950126));
#43518=CARTESIAN_POINT('Ctrl Pts',(0.964800452845084,-0.437712317069721,
58.4868622603097));
#43519=CARTESIAN_POINT('Ctrl Pts',(1.0567010533528,0.0762552959977839,58.5106376256069));
#43520=CARTESIAN_POINT('Ctrl Pts',(0.891957495313147,0.571702556299444,
58.534412990904));
#43521=CARTESIAN_POINT('Ctrl Pts',(0.51058154146171,0.928298699688416,58.5581883562012));
#43522=CARTESIAN_POINT('Ctrl Pts',(0.00519911514345259,1.059436149811,58.5819637214983));
#43523=CARTESIAN_POINT('Ctrl Pts',(-0.501446035884838,0.93326516029476,
58.6057390867955));
#43524=CARTESIAN_POINT('Ctrl Pts',(-0.886303482123542,0.580429258308285,
58.6295144520927));
#43525=CARTESIAN_POINT('Ctrl Pts',(-1.05590173971521,0.0866227590822638,
58.6532898173898));
#43526=CARTESIAN_POINT('Ctrl Pts',(-0.969049970463342,-0.428222069806799,
58.677065182687));
#43527=CARTESIAN_POINT('Ctrl Pts',(-0.646842124418696,-0.839063318470144,
58.7008405479841));
#43528=CARTESIAN_POINT('Ctrl Pts',(-0.167533788876386,-1.04611873891511,
58.7246159132813));
#43529=CARTESIAN_POINT('Ctrl Pts',(0.352463981145058,-0.999100159303358,
58.7483912785784));
#43530=CARTESIAN_POINT('Ctrl Pts',(0.786857765467602,-0.709427123281846,
58.7721666438756));
#43531=CARTESIAN_POINT('Ctrl Pts',(1.03014504102483,-0.247453391119582,
58.7959420091728));
#43532=CARTESIAN_POINT('Ctrl Pts',(1.0232378965077,0.274620089350941,58.8197173744699));
#43533=CARTESIAN_POINT('Ctrl Pts',(0.767813890850171,0.729995763920686,
58.8434927397671));
#43534=CARTESIAN_POINT('Ctrl Pts',(0.325908619452451,1.00807517482141,58.8672681050642));
#43535=CARTESIAN_POINT('Ctrl Pts',(-0.195151057192915,1.04132034033774,
58.8910434703614));
#43536=CARTESIAN_POINT('Ctrl Pts',(-0.66881381045679,0.821656907271453,
58.9148188356585));
#43537=CARTESIAN_POINT('Ctrl Pts',(-0.980039744844674,0.402435193353424,
58.9385942009557));
#43538=CARTESIAN_POINT('Ctrl Pts',(-1.05324048292885,-0.114527164657214,
58.9623695662528));
#43539=CARTESIAN_POINT('Ctrl Pts',(-0.870637541598082,-0.603673966214107,
58.98614493155));
#43540=CARTESIAN_POINT('Ctrl Pts',(-0.476580245647126,-0.946204658508691,
59.0099202968471));
#43541=CARTESIAN_POINT('Ctrl Pts',(0.0332255259359154,-1.05892778353904,
59.0336956621443));
#43542=CARTESIAN_POINT('Ctrl Pts',(0.534961714244608,-0.914465937373881,
59.0574710274415));
#43543=CARTESIAN_POINT('Ctrl Pts',(0.906770144298739,-0.547905002471288,
59.0812463927386));
#43544=CARTESIAN_POINT('Ctrl Pts',(1.05834858599332,-0.0482727340283605,
59.1050217580358));
#43545=CARTESIAN_POINT('Ctrl Pts',(0.952882727939887,0.463083678311449,
59.1287971233329));
#43546=CARTESIAN_POINT('Ctrl Pts',(0.615987379842406,0.861969566863883,
59.15257248863));
#43547=CARTESIAN_POINT('Ctrl Pts',(0.129485326732331,1.05150631785341,59.1763478539272));
#43548=CARTESIAN_POINT('Ctrl Pts',(-0.388465216580355,0.985660571308298,
59.2001232192243));
#43549=CARTESIAN_POINT('Ctrl Pts',(-0.812068046017044,0.680424481454538,
59.2238985845215));
#43550=CARTESIAN_POINT('Ctrl Pts',(-1.03844147013426,0.209931654187809,
59.2476739498187));
#43551=CARTESIAN_POINT('Ctrl Pts',(-1.01260549552161,-0.311547904444929,
59.2714493151158));
#43552=CARTESIAN_POINT('Ctrl Pts',(-0.740834982929712,-0.75736088781519,
59.295224680413));
#43553=CARTESIAN_POINT('Ctrl Pts',(-0.289135652993162,-1.01923135768715,
59.3190000457102));
#43554=CARTESIAN_POINT('Ctrl Pts',(0.232786921381965,-1.0335580465354,59.3427754110073));
#43555=CARTESIAN_POINT('Ctrl Pts',(0.698171837004391,-0.796861388410206,
59.3665507763045));
#43556=CARTESIAN_POINT('Ctrl Pts',(0.993989661666965,-0.36662861157061,
59.3903261416016));
#43557=CARTESIAN_POINT('Ctrl Pts',(1.04839423183335,0.152648357301901,59.4141015068988));
#43558=CARTESIAN_POINT('Ctrl Pts',(0.848172146135856,0.634851161168593,
59.4378768721959));
#43559=CARTESIAN_POINT('Ctrl Pts',(0.441951943904046,0.962865756797002,
59.4616522374931));
#43560=CARTESIAN_POINT('Ctrl Pts',(-0.0716064543484882,1.05702625417764,
59.4854276027902));
#43561=CARTESIAN_POINT('Ctrl Pts',(-0.567773577890534,0.894463610514046,
59.5092029680874));
#43562=CARTESIAN_POINT('Ctrl Pts',(-0.926043827475508,0.514659903303883,
59.5329783333845));
#43563=CARTESIAN_POINT('Ctrl Pts',(-1.05940303101641,0.00985919965667513,
59.5567536986817));
#43564=CARTESIAN_POINT('Ctrl Pts',(-0.935461839364852,-0.497336037464362,
59.5805290639788));
#43565=CARTESIAN_POINT('Ctrl Pts',(-0.584322219507429,-0.883741777366003,
59.604304429276));
#43566=CARTESIAN_POINT('Ctrl Pts',(-0.0912665108790651,-1.05551049774341,
59.6280797945731));
#43567=CARTESIAN_POINT('Ctrl Pts',(0.423955377218644,-0.970924212970794,
59.6518551598703));
#43568=CARTESIAN_POINT('Ctrl Pts',(0.836209932593474,-0.65052664940127,
59.6756305251674));
#43569=CARTESIAN_POINT('Ctrl Pts',(1.04537170665504,-0.172133722736198,
59.6994058904646));
#43570=CARTESIAN_POINT('Ctrl Pts',(1.00064083593713,0.348065833975191,59.7231812557618));
#43571=CARTESIAN_POINT('Ctrl Pts',(0.712881489585019,0.783729605291864,
59.7469566210589));
#43572=CARTESIAN_POINT('Ctrl Pts',(0.251982109139772,1.02904659423647,59.7707319863561));
#43573=CARTESIAN_POINT('Ctrl Pts',(-0.270116136119136,1.02443598919684,
59.7945073516532));
#43574=CARTESIAN_POINT('Ctrl Pts',(-0.726612165168123,0.7710174527789,59.8182827169504));
#43575=CARTESIAN_POINT('Ctrl Pts',(-1.00663007332738,0.330339808155829,
59.8420580822475));
#43576=CARTESIAN_POINT('Ctrl Pts',(-1.04217267078573,-0.19056878179354,
59.8658334475447));
#43577=CARTESIAN_POINT('Ctrl Pts',(-0.82458300673366,-0.665192014605423,
59.8896088128418));
#43578=CARTESIAN_POINT('Ctrl Pts',(-0.406762579630654,-0.978258004694046,
59.913384178139));
#43579=CARTESIAN_POINT('Ctrl Pts',(0.109922024153085,-1.05371848840101,
59.9371595434362));
#43580=CARTESIAN_POINT('Ctrl Pts',(0.436436372439967,-0.933386554993731,
59.9530097869676));
#43581=CARTESIAN_POINT('Ctrl Pts',(0.575507505002819,-0.837861884388131,
59.9609349087333));
#43582=CARTESIAN_POINT('Ctrl Pts',(0.672748867539213,-0.979432290589659,
59.861775));
#43583=CARTESIAN_POINT('Ctrl Pts',(0.510179402978367,-1.09109740948616,
59.8538498782343));
#43584=CARTESIAN_POINT('Ctrl Pts',(0.319337271350366,-1.16142939579809,
59.8459247564686));
#43585=CARTESIAN_POINT('Ctrl Pts',(0.123251725621158,-1.18189359545975,
59.8379996347028));
#43586=CARTESIAN_POINT('Ctrl Pts',(-0.0728338201080729,-1.20235779512143,
59.8300745129371));
#43587=CARTESIAN_POINT('Ctrl Pts',(-0.274162779938513,-1.17295420813283,
59.8221493911714));
#43588=CARTESIAN_POINT('Ctrl Pts',(-0.456230258286956,-1.09725848363956,
59.8142242694057));
#43589=CARTESIAN_POINT('Ctrl Pts',(-0.638297736635399,-1.02156275914629,
59.80629914764));
#43590=CARTESIAN_POINT('Ctrl Pts',(-0.801103733501846,-0.899574897148353,
59.7983740258743));
#43591=CARTESIAN_POINT('Ctrl Pts',(-0.924899228646461,-0.74611120696398,
59.7904489041085));
#43592=CARTESIAN_POINT('Ctrl Pts',(-1.04869472379108,-0.592647516779607,
59.7825237823428));
#43593=CARTESIAN_POINT('Ctrl Pts',(-1.13347971721386,-0.407707998408799,
59.7745986605771));
#43594=CARTESIAN_POINT('Ctrl Pts',(-1.16894753093338,-0.213750809742003,
59.7666735388113));
#43595=CARTESIAN_POINT('Ctrl Pts',(-1.18182974287435,-0.143303907329611,
59.7637950671059));
#43596=CARTESIAN_POINT('Ctrl Pts',(-1.18820601150139,-0.0716673900178602,
59.7609165954006));
#43597=CARTESIAN_POINT('Ctrl Pts',(-1.18815715028295,-2.22996587661006E-5,
59.7580381236952));
#43598=CARTESIAN_POINT('Origin',(0.,0.,57.95));
#43599=CARTESIAN_POINT('Origin',(0.,0.,59.861775));
#43600=CARTESIAN_POINT('Origin',(1.7,0.,-23.));
#43601=CARTESIAN_POINT('',(-1.7,-2.0818995585505E-16,-23.));
#43602=CARTESIAN_POINT('Origin',(0.,0.,-23.));
#43603=CARTESIAN_POINT('Origin',(0.,0.,-22.85));
#43604=CARTESIAN_POINT('',(-2.,-2.4492935982947E-16,-22.7));
#43605=CARTESIAN_POINT('Origin',(0.,0.,-22.7));
#43606=CARTESIAN_POINT('',(-1.85,-2.2655965784226E-16,-22.85));
#43607=CARTESIAN_POINT('Origin',(0.,0.,16.65));
#43608=CARTESIAN_POINT('',(-2.,-2.44929359829471E-16,56.));
#43609=CARTESIAN_POINT('Origin',(0.,0.,56.));
#43610=CARTESIAN_POINT('',(-2.,-2.44929359829471E-16,16.65));
#43611=CARTESIAN_POINT('Origin',(1.25,0.,56.));
#43612=CARTESIAN_POINT('',(-1.25,-1.53080849893419E-16,56.));
#43613=CARTESIAN_POINT('Origin',(0.,0.,56.));
#43614=CARTESIAN_POINT('Origin',(0.,0.,56.025));
#43615=CARTESIAN_POINT('',(-1.225,-1.50019232895551E-16,56.025));
#43616=CARTESIAN_POINT('Origin',(0.,0.,59.925));
#43617=CARTESIAN_POINT('',(-1.05,-1.28587913910472E-16,60.));
#43618=CARTESIAN_POINT('Origin',(0.,0.,60.));
#43619=CARTESIAN_POINT('',(-1.125,-1.37772764904077E-16,59.925));
#43620=CARTESIAN_POINT('Origin',(0.,0.,60.));
#43621=CARTESIAN_POINT('',(0.,0.,0.));
#43622=CARTESIAN_POINT('Origin',(8.82473422894286,15.6190101383511,11.));
#43623=CARTESIAN_POINT('',(8.77479843761413,15.5731118537254,15.4247984376141));
#43624=CARTESIAN_POINT('',(8.89946845788571,15.6877018085946,15.3));
#43625=CARTESIAN_POINT('Ctrl Pts',(8.77479843761413,15.5731118537254,15.4247984376141));
#43626=CARTESIAN_POINT('Ctrl Pts',(8.8368855031481,15.6301789338622,15.3628561636274));
#43627=CARTESIAN_POINT('Ctrl Pts',(8.89946845788572,15.6877018085946,15.3));
#43628=CARTESIAN_POINT('',(8.89946845788571,15.6877018085946,11.2));
#43629=CARTESIAN_POINT('',(8.89946845788571,15.6877018085946,11.));
#43630=CARTESIAN_POINT('',(8.79981911738071,15.5961095123365,11.1001808826193));
#43631=CARTESIAN_POINT('Ctrl Pts',(8.89946845788572,15.6877018085946,11.2));
#43632=CARTESIAN_POINT('Ctrl Pts',(8.84948539827205,15.6417600775122,11.1497987369429));
#43633=CARTESIAN_POINT('Ctrl Pts',(8.79981911738071,15.5961095123365,11.1001808826193));
#43634=CARTESIAN_POINT('',(8.75,15.5503184681076,11.15));
#43635=CARTESIAN_POINT('',(7.66780970362768,14.5556275476194,12.2321902963723));
#43636=CARTESIAN_POINT('',(8.75,15.5503184681076,15.4));
#43637=CARTESIAN_POINT('',(8.75,15.5503184681076,11.));
#43638=CARTESIAN_POINT('',(6.85932538040084,13.8125123872206,13.5093253804008));
#43639=CARTESIAN_POINT('Origin',(7.5,0.,11.));
#43640=CARTESIAN_POINT('',(22.9811689265378,2.89756944144577,15.3));
#43641=CARTESIAN_POINT('Origin',(7.5,0.,15.3));
#43642=CARTESIAN_POINT('',(22.9811689265378,2.89756944144577,11.2));
#43643=CARTESIAN_POINT('',(22.9811689265378,2.89756944144577,11.));
#43644=CARTESIAN_POINT('Origin',(7.5,0.,11.2));
#43645=CARTESIAN_POINT('Origin',(7.5,0.,15.4));
#43646=CARTESIAN_POINT('',(8.77928932188135,15.5682375662889,15.4292893218813));
#43647=CARTESIAN_POINT('Ctrl Pts',(8.77928932188135,15.5682375662889,15.4292893218813));
#43648=CARTESIAN_POINT('Ctrl Pts',(8.77704423120747,15.5706747100072,15.4270442312075));
#43649=CARTESIAN_POINT('Ctrl Pts',(8.77479843761413,15.5731118537254,15.4247984376141));
#43650=CARTESIAN_POINT('',(22.8714720490513,2.77928932188135,15.4292893218813));
#43651=CARTESIAN_POINT('Origin',(7.5,-9.56492666618245E-16,15.4292893218813));
#43652=CARTESIAN_POINT('',(22.877968161414,2.77386128332979,15.4238612833298));
#43653=CARTESIAN_POINT('Ctrl Pts',(22.877968161414,2.77386128332979,15.4238612833298));
#43654=CARTESIAN_POINT('Ctrl Pts',(22.8747201052327,2.77657587596802,15.426575875968));
#43655=CARTESIAN_POINT('Ctrl Pts',(22.8714720490513,2.77928932188135,15.4292893218813));
#43656=CARTESIAN_POINT('Ctrl Pts',(22.9811689265378,2.89756944144577,15.3));
#43657=CARTESIAN_POINT('Ctrl Pts',(22.9293648449271,2.83547118557273,15.3623442379101));
#43658=CARTESIAN_POINT('Ctrl Pts',(22.877968161414,2.77386128332979,15.4238612833298));
#43659=CARTESIAN_POINT('Origin',(8.8,8.375,15.45));
#43660=CARTESIAN_POINT('',(8.75,7.5,15.4));
#43661=CARTESIAN_POINT('',(8.75,8.375,15.4));
#43662=CARTESIAN_POINT('',(8.85,7.5,15.5));
#43663=CARTESIAN_POINT('',(8.75,7.5,15.4));
#43664=CARTESIAN_POINT('',(8.85,15.3909064060568,15.5));
#43665=CARTESIAN_POINT('',(8.85,8.375,15.5));
#43666=CARTESIAN_POINT('Ctrl Pts',(8.77928932188134,15.5682375662889,15.4292893218812));
#43667=CARTESIAN_POINT('Ctrl Pts',(8.80288271557749,15.5091473511845,15.4528827155773));
#43668=CARTESIAN_POINT('Ctrl Pts',(8.826454184001,15.4500345909188,15.4764541840008));
#43669=CARTESIAN_POINT('Ctrl Pts',(8.84999999999999,15.3909064060567,15.4999999999998));
#43670=CARTESIAN_POINT('Origin',(6.17526577105714,15.6190101383511,11.));
#43671=CARTESIAN_POINT('',(6.20018088261929,15.5961095123365,11.1001808826193));
#43672=CARTESIAN_POINT('',(6.10053154211429,15.6877018085946,11.2));
#43673=CARTESIAN_POINT('Ctrl Pts',(6.20018088261929,15.5961095123365,11.1001808826193));
#43674=CARTESIAN_POINT('Ctrl Pts',(6.15051460172865,15.6417600775116,11.1497987369422));
#43675=CARTESIAN_POINT('Ctrl Pts',(6.10053154211428,15.6877018085946,11.2));
#43676=CARTESIAN_POINT('',(6.10053154211429,15.6877018085946,15.3));
#43677=CARTESIAN_POINT('',(6.10053154211429,15.6877018085946,11.));
#43678=CARTESIAN_POINT('',(6.22520156238587,15.5731118537254,15.4247984376141));
#43679=CARTESIAN_POINT('Ctrl Pts',(6.10053154211428,15.6877018085946,15.3));
#43680=CARTESIAN_POINT('Ctrl Pts',(6.16311449685252,15.6301789338617,15.362856163628));
#43681=CARTESIAN_POINT('Ctrl Pts',(6.22520156238587,15.5731118537254,15.4247984376141));
#43682=CARTESIAN_POINT('',(6.25,15.5503184681076,15.4));
#43683=CARTESIAN_POINT('',(8.88782844934798,13.1257689067529,12.762171550652));
#43684=CARTESIAN_POINT('',(6.25,15.5503184681076,11.15));
#43685=CARTESIAN_POINT('',(6.25,15.5503184681076,11.));
#43686=CARTESIAN_POINT('',(8.07934412612115,13.8688840671517,12.9793441261211));
#43687=CARTESIAN_POINT('Origin',(6.175,3.75,11.075));
#43688=CARTESIAN_POINT('',(6.25,7.5,11.15));
#43689=CARTESIAN_POINT('',(6.25,3.75,11.15));
#43690=CARTESIAN_POINT('',(6.1,7.5,11.));
#43691=CARTESIAN_POINT('',(6.25,7.5,11.15));
#43692=CARTESIAN_POINT('',(6.1,15.4868492599366,11.));
#43693=CARTESIAN_POINT('',(6.1,3.75,11.));
#43694=CARTESIAN_POINT('Ctrl Pts',(6.1,15.4868492599366,11.));
#43695=CARTESIAN_POINT('Ctrl Pts',(6.14991436752269,15.5414793861366,11.0499143675227));
#43696=CARTESIAN_POINT('Ctrl Pts',(6.20018088261929,15.5961095123365,11.1001808826193));
#43697=CARTESIAN_POINT('Origin',(6.25,7.5,15.5));
#43698=CARTESIAN_POINT('',(6.25,7.5,15.4));
#43699=CARTESIAN_POINT('',(6.25,3.75,15.4));
#43700=CARTESIAN_POINT('',(6.25,7.5,15.5));
#43701=CARTESIAN_POINT('Origin',(6.2,3.75,15.45));
#43702=CARTESIAN_POINT('',(6.22071067811865,15.568237566289,15.4292893218813));
#43703=CARTESIAN_POINT('Ctrl Pts',(6.22520156238587,15.5731118537254,15.4247984376141));
#43704=CARTESIAN_POINT('Ctrl Pts',(6.22295576879253,15.5706747100072,15.4270442312075));
#43705=CARTESIAN_POINT('Ctrl Pts',(6.22071067811865,15.568237566289,15.4292893218813));
#43706=CARTESIAN_POINT('',(6.15,15.3909064060568,15.5));
#43707=CARTESIAN_POINT('Ctrl Pts',(6.15000000000001,15.3909064060567,15.4999999999998));
#43708=CARTESIAN_POINT('Ctrl Pts',(6.17354581599823,15.4500345909168,15.4764541840016));
#43709=CARTESIAN_POINT('Ctrl Pts',(6.19711728442092,15.5091473511805,15.4528827155789));
#43710=CARTESIAN_POINT('Ctrl Pts',(6.22071067811866,15.5682375662889,15.4292893218812));
#43711=CARTESIAN_POINT('',(6.15,7.5,15.5));
#43712=CARTESIAN_POINT('',(6.15,3.75,15.5));
#43713=CARTESIAN_POINT('',(6.25,7.5,15.4));
#43714=CARTESIAN_POINT('Origin',(7.5,7.5,11.075));
#43715=CARTESIAN_POINT('',(8.75,7.5,11.15));
#43716=CARTESIAN_POINT('',(8.9,7.5,11.));
#43717=CARTESIAN_POINT('',(8.75,7.5,11.15));
#43718=CARTESIAN_POINT('Origin',(7.5,7.5,11.));
#43719=CARTESIAN_POINT('Origin',(7.5,7.5,11.15));
#43720=CARTESIAN_POINT('Origin',(8.825,8.375,11.075));
#43721=CARTESIAN_POINT('',(8.9,15.4868492599366,11.));
#43722=CARTESIAN_POINT('Ctrl Pts',(8.79981911738071,15.5961095123365,11.1001808826193));
#43723=CARTESIAN_POINT('Ctrl Pts',(8.85008563247733,15.5414793861366,11.0499143675227));
#43724=CARTESIAN_POINT('Ctrl Pts',(8.9,15.4868492599366,11.));
#43725=CARTESIAN_POINT('',(8.9,8.375,11.));
#43726=CARTESIAN_POINT('',(8.75,8.375,11.15));
#43727=CARTESIAN_POINT('Origin',(7.5,0.,11.));
#43728=CARTESIAN_POINT('',(22.777188877539,2.9,11.));
#43729=CARTESIAN_POINT('Origin',(7.5,0.,11.));
#43730=CARTESIAN_POINT('',(15.,2.9,11.));
#43731=CARTESIAN_POINT('',(11.25,2.9,11.));
#43732=CARTESIAN_POINT('',(15.,-2.9,11.));
#43733=CARTESIAN_POINT('Origin',(15.,0.,11.));
#43734=CARTESIAN_POINT('',(22.777188877539,-2.9,11.));
#43735=CARTESIAN_POINT('',(15.875,-2.9,11.));
#43736=CARTESIAN_POINT('',(11.15,-15.1155549021529,11.));
#43737=CARTESIAN_POINT('Origin',(7.5,0.,11.));
#43738=CARTESIAN_POINT('',(11.15,-7.5,11.));
#43739=CARTESIAN_POINT('',(11.15,-3.75,11.));
#43740=CARTESIAN_POINT('',(3.85,-7.5,11.));
#43741=CARTESIAN_POINT('Origin',(7.5,-7.5,11.));
#43742=CARTESIAN_POINT('',(3.85,-15.1155549021529,11.));
#43743=CARTESIAN_POINT('',(3.85,-8.375,11.));
#43744=CARTESIAN_POINT('',(-7.90064933695979,-2.15,11.));
#43745=CARTESIAN_POINT('Origin',(7.5,0.,11.));
#43746=CARTESIAN_POINT('',(-4.44089209850063E-16,-2.15,11.));
#43747=CARTESIAN_POINT('',(3.75,-2.15,11.));
#43748=CARTESIAN_POINT('',(1.21771195646252E-15,2.15,11.));
#43749=CARTESIAN_POINT('Origin',(3.33066907387547E-16,1.11022302462516E-15,
11.));
#43750=CARTESIAN_POINT('',(-7.90064933695979,2.15,11.));
#43751=CARTESIAN_POINT('',(-0.875,2.15,11.));
#43752=CARTESIAN_POINT('Origin',(7.5,0.,11.));
#43753=CARTESIAN_POINT('',(5.345,2.63911385216255E-16,11.));
#43754=CARTESIAN_POINT('Origin',(7.5,0.,11.));
#43755=CARTESIAN_POINT('Origin',(7.5,0.,11.1));
#43756=CARTESIAN_POINT('',(22.8988337499022,2.79887314750332,11.1011268524967));
#43757=CARTESIAN_POINT('Ctrl Pts',(22.8988337499022,2.79887314750332,11.1011268524967));
#43758=CARTESIAN_POINT('Ctrl Pts',(22.9398717132847,2.84806591130492,11.1503003777304));
#43759=CARTESIAN_POINT('Ctrl Pts',(22.9811689265378,2.89756944144577,11.2));
#43760=CARTESIAN_POINT('Ctrl Pts',(22.777188877539,2.9,11.));
#43761=CARTESIAN_POINT('Ctrl Pts',(22.8380113137205,2.84963708154271,11.0503629184573));
#43762=CARTESIAN_POINT('Ctrl Pts',(22.8988337499022,2.79887314750332,11.1011268524967));
#43763=CARTESIAN_POINT('Origin',(22.9196156729043,-2.82378472072289,11.));
#43764=CARTESIAN_POINT('',(22.877968161414,-2.77386128332979,15.4238612833298));
#43765=CARTESIAN_POINT('',(22.9811689265378,-2.89756944144577,15.3));
#43766=CARTESIAN_POINT('Ctrl Pts',(22.877968161414,-2.77386128332979,15.4238612833298));
#43767=CARTESIAN_POINT('Ctrl Pts',(22.9293648449275,-2.83547118557317,15.3623442379097));
#43768=CARTESIAN_POINT('Ctrl Pts',(22.9811689265378,-2.89756944144577,15.3));
#43769=CARTESIAN_POINT('',(22.9811689265378,-2.89756944144577,11.2));
#43770=CARTESIAN_POINT('',(22.9811689265378,-2.89756944144577,11.));
#43771=CARTESIAN_POINT('',(22.8988337499022,-2.79887314750331,11.1011268524967));
#43772=CARTESIAN_POINT('Ctrl Pts',(22.9811689265378,-2.89756944144577,11.2));
#43773=CARTESIAN_POINT('Ctrl Pts',(22.9398717132847,-2.84806591130493,11.1503003777304));
#43774=CARTESIAN_POINT('Ctrl Pts',(22.8988337499022,-2.79887314750331,11.1011268524967));
#43775=CARTESIAN_POINT('',(22.8580624192708,-2.75,11.15));
#43776=CARTESIAN_POINT('',(22.0225261537486,-1.74843133601861,12.1515686639814));
#43777=CARTESIAN_POINT('',(22.8580624192708,-2.75,15.4));
#43778=CARTESIAN_POINT('',(22.8580624192708,-2.75,11.));
#43779=CARTESIAN_POINT('',(21.310816473291,-0.895295280514285,13.5452952805143));
#43780=CARTESIAN_POINT('Origin',(15.875,-2.8,15.45));
#43781=CARTESIAN_POINT('',(15.,-2.75,15.4));
#43782=CARTESIAN_POINT('',(15.875,-2.75,15.4));
#43783=CARTESIAN_POINT('',(15.,-2.85,15.5));
#43784=CARTESIAN_POINT('',(15.,-2.75,15.4));
#43785=CARTESIAN_POINT('',(22.6848608818125,-2.85,15.5));
#43786=CARTESIAN_POINT('',(15.875,-2.85,15.5));
#43787=CARTESIAN_POINT('',(22.8714720490513,-2.77928932188134,15.4292893218813));
#43788=CARTESIAN_POINT('Ctrl Pts',(22.8714720490514,-2.77928932188136,15.4292893218813));
#43789=CARTESIAN_POINT('Ctrl Pts',(22.8092954963184,-2.80289320050232,15.4528932005023));
#43790=CARTESIAN_POINT('Ctrl Pts',(22.7470894475605,-2.82646471883622,15.4764647188362));
#43791=CARTESIAN_POINT('Ctrl Pts',(22.6848608818126,-2.85000000000001,15.5));
#43792=CARTESIAN_POINT('Ctrl Pts',(22.8714720490513,-2.77928932188134,15.4292893218813));
#43793=CARTESIAN_POINT('Ctrl Pts',(22.8747201052327,-2.776575875968,15.426575875968));
#43794=CARTESIAN_POINT('Ctrl Pts',(22.877968161414,-2.77386128332979,15.4238612833298));
#43795=CARTESIAN_POINT('Origin',(24.25,-2.75,15.5));
#43796=CARTESIAN_POINT('',(15.,-2.75,11.15));
#43797=CARTESIAN_POINT('',(15.875,-2.75,11.15));
#43798=CARTESIAN_POINT('',(15.,-2.75,15.5));
#43799=CARTESIAN_POINT('Origin',(15.875,-2.825,11.075));
#43800=CARTESIAN_POINT('Ctrl Pts',(22.8988337499022,-2.79887314750332,11.1011268524967));
#43801=CARTESIAN_POINT('Ctrl Pts',(22.8380113137205,-2.84963708154272,11.0503629184573));
#43802=CARTESIAN_POINT('Ctrl Pts',(22.777188877539,-2.9,11.));
#43803=CARTESIAN_POINT('',(15.,-2.75,11.15));
#43804=CARTESIAN_POINT('Origin',(22.9196156729043,2.82378472072289,11.));
#43805=CARTESIAN_POINT('',(22.8580624192708,2.75,15.4));
#43806=CARTESIAN_POINT('',(20.7138618022943,0.179717612662962,12.8297176126629));
#43807=CARTESIAN_POINT('',(22.8580624192708,2.75,11.15));
#43808=CARTESIAN_POINT('',(22.8580624192708,2.75,11.));
#43809=CARTESIAN_POINT('',(21.4255714827519,1.03285366816728,12.8671463318327));
#43810=CARTESIAN_POINT('Origin',(11.25,2.825,11.075));
#43811=CARTESIAN_POINT('',(15.,2.75,11.15));
#43812=CARTESIAN_POINT('',(11.25,2.75,11.15));
#43813=CARTESIAN_POINT('',(15.,2.75,11.15));
#43814=CARTESIAN_POINT('Origin',(15.,0.,11.075));
#43815=CARTESIAN_POINT('Origin',(15.,0.,11.15));
#43816=CARTESIAN_POINT('Origin',(7.5,0.,11.1));
#43817=CARTESIAN_POINT('',(11.1460890181319,-15.3221582967889,11.2));
#43818=CARTESIAN_POINT('Origin',(7.5,0.,11.2));
#43819=CARTESIAN_POINT('',(11.0481336735778,-15.2443978869161,11.1018663264221));
#43820=CARTESIAN_POINT('Ctrl Pts',(11.0481336735779,-15.2443978869161,11.1018663264222));
#43821=CARTESIAN_POINT('Ctrl Pts',(11.0969582861968,-15.2831565876936,11.1506841026816));
#43822=CARTESIAN_POINT('Ctrl Pts',(11.1460890181319,-15.3221582967889,11.2));
#43823=CARTESIAN_POINT('Ctrl Pts',(11.15,-15.1155549021529,11.));
#43824=CARTESIAN_POINT('Ctrl Pts',(11.0992829893245,-15.1799763945344,11.0507170106755));
#43825=CARTESIAN_POINT('Ctrl Pts',(11.0481336735778,-15.2443978869161,11.1018663264221));
#43826=CARTESIAN_POINT('Origin',(15.,0.,15.5));
#43827=CARTESIAN_POINT('',(15.,2.75,15.4));
#43828=CARTESIAN_POINT('',(15.,2.75,15.5));
#43829=CARTESIAN_POINT('Origin',(15.,0.,15.4));
#43830=CARTESIAN_POINT('Origin',(15.,2.75,15.5));
#43831=CARTESIAN_POINT('',(11.25,2.75,15.4));
#43832=CARTESIAN_POINT('Origin',(7.5,0.,11.075));
#43833=CARTESIAN_POINT('',(5.495,-2.45541683229044E-16,11.15));
#43834=CARTESIAN_POINT('',(5.42,2.54726534222649E-16,11.075));
#43835=CARTESIAN_POINT('Origin',(7.5,0.,11.15));
#43836=CARTESIAN_POINT('Origin',(7.5,0.,15.5));
#43837=CARTESIAN_POINT('',(5.495,2.45541683229044E-16,15.4));
#43838=CARTESIAN_POINT('Origin',(7.5,0.,15.4));
#43839=CARTESIAN_POINT('',(5.495,2.45541683229044E-16,15.5));
#43840=CARTESIAN_POINT('Origin',(-8.03762184672835,2.0743466612552,11.));
#43841=CARTESIAN_POINT('',(-7.99388777632041,2.02441760835096,15.424417608351));
#43842=CARTESIAN_POINT('',(-8.10274389348871,2.1486933225104,15.3));
#43843=CARTESIAN_POINT('Ctrl Pts',(-7.99388777632041,2.02441760835096,15.424417608351));
#43844=CARTESIAN_POINT('Ctrl Pts',(-8.04810000436536,2.08630906224183,15.3626437619559));
#43845=CARTESIAN_POINT('Ctrl Pts',(-8.10274389348871,2.1486933225104,15.3));
#43846=CARTESIAN_POINT('',(-8.10274389348871,2.1486933225104,11.2));
#43847=CARTESIAN_POINT('',(-8.10274389348871,2.1486933225104,11.));
#43848=CARTESIAN_POINT('',(-8.01579995129907,2.04943366867993,11.1005663313201));
#43849=CARTESIAN_POINT('Ctrl Pts',(-8.10274389348871,2.1486933225104,11.2));
#43850=CARTESIAN_POINT('Ctrl Pts',(-8.05913426317107,2.09890633678157,11.1500059138463));
#43851=CARTESIAN_POINT('Ctrl Pts',(-8.01579995129907,2.04943366867993,11.1005663313201));
#43852=CARTESIAN_POINT('',(-7.97249979996799,2.,11.15));
#43853=CARTESIAN_POINT('',(-7.05685105019854,0.954648528195632,12.1953514718044));
#43854=CARTESIAN_POINT('',(-7.97249979996799,2.,15.4));
#43855=CARTESIAN_POINT('',(-7.97249979996799,2.,11.));
#43856=CARTESIAN_POINT('',(-6.32882477728353,0.12349647770076,13.5234964777007));
#43857=CARTESIAN_POINT('Origin',(-0.875,2.05,15.45));
#43858=CARTESIAN_POINT('',(1.15599253443404E-15,2.,15.4));
#43859=CARTESIAN_POINT('',(-0.875,2.,15.4));
#43860=CARTESIAN_POINT('',(1.11022302462516E-15,2.1,15.5));
#43861=CARTESIAN_POINT('',(1.15599253443404E-15,2.,15.4));
#43862=CARTESIAN_POINT('',(-7.80661621652545,2.1,15.5));
#43863=CARTESIAN_POINT('',(-0.875,2.1,15.5));
#43864=CARTESIAN_POINT('',(-7.9883371262892,2.02928932188135,15.4292893218813));
#43865=CARTESIAN_POINT('Ctrl Pts',(-7.9883371262892,2.02928932188135,15.4292893218813));
#43866=CARTESIAN_POINT('Ctrl Pts',(-7.92778701650562,2.05288762137753,15.4528876213775));
#43867=CARTESIAN_POINT('Ctrl Pts',(-7.86721103212806,2.07645911131076,15.4764591113107));
#43868=CARTESIAN_POINT('Ctrl Pts',(-7.80661621652544,2.1,15.5));
#43869=CARTESIAN_POINT('Ctrl Pts',(-7.9883371262892,2.02928932188135,15.4292893218813));
#43870=CARTESIAN_POINT('Ctrl Pts',(-7.99111245130481,2.02685390151439,15.4268539015144));
#43871=CARTESIAN_POINT('Ctrl Pts',(-7.99388777632041,2.02441760835096,15.424417608351));
#43872=CARTESIAN_POINT('Origin',(-9.25,2.,15.5));
#43873=CARTESIAN_POINT('',(1.15599253443404E-15,2.,11.15));
#43874=CARTESIAN_POINT('',(-0.875,2.,11.15));
#43875=CARTESIAN_POINT('',(1.15599253443404E-15,2.,15.5));
#43876=CARTESIAN_POINT('Origin',(-0.875,2.075,11.075));
#43877=CARTESIAN_POINT('Ctrl Pts',(-8.01579995129907,2.04943366867993,11.1005663313201));
#43878=CARTESIAN_POINT('Ctrl Pts',(-7.95822464412934,2.09990411772965,11.0500958822704));
#43879=CARTESIAN_POINT('Ctrl Pts',(-7.90064933695979,2.15,11.));
#43880=CARTESIAN_POINT('',(1.15599253443404E-15,2.,11.15));
#43881=CARTESIAN_POINT('Origin',(-8.03762184672835,-2.0743466612552,11.));
#43882=CARTESIAN_POINT('',(-8.01579995129907,-2.04943366867993,11.1005663313201));
#43883=CARTESIAN_POINT('',(-8.10274389348871,-2.14869332251039,11.2));
#43884=CARTESIAN_POINT('Ctrl Pts',(-8.01579995129907,-2.04943366867993,
11.1005663313201));
#43885=CARTESIAN_POINT('Ctrl Pts',(-8.05913426317095,-2.09890633678143,
11.1500059138462));
#43886=CARTESIAN_POINT('Ctrl Pts',(-8.10274389348871,-2.1486933225104,11.2));
#43887=CARTESIAN_POINT('',(-8.10274389348871,-2.14869332251039,15.3));
#43888=CARTESIAN_POINT('',(-8.10274389348871,-2.14869332251039,11.));
#43889=CARTESIAN_POINT('',(-7.99388777632041,-2.02441760835096,15.424417608351));
#43890=CARTESIAN_POINT('Ctrl Pts',(-8.10274389348871,-2.1486933225104,15.3));
#43891=CARTESIAN_POINT('Ctrl Pts',(-8.04810000436667,-2.08630906224331,
15.3626437619544));
#43892=CARTESIAN_POINT('Ctrl Pts',(-7.99388777632041,-2.02441760835096,
15.424417608351));
#43893=CARTESIAN_POINT('',(-7.97249979996799,-2.,15.4));
#43894=CARTESIAN_POINT('',(-5.68766313969174,0.608486459740959,12.791513540259));
#43895=CARTESIAN_POINT('',(-7.97249979996799,-2.,11.15));
#43896=CARTESIAN_POINT('',(-7.97249979996799,-2.,11.));
#43897=CARTESIAN_POINT('',(-6.41568941260673,-0.222665590753897,12.9273344092461));
#43898=CARTESIAN_POINT('Origin',(7.5,0.,11.));
#43899=CARTESIAN_POINT('',(3.85391098186813,-15.3221582967889,11.2));
#43900=CARTESIAN_POINT('Origin',(7.5,0.,11.2));
#43901=CARTESIAN_POINT('',(3.85391098186813,-15.3221582967889,15.3));
#43902=CARTESIAN_POINT('',(3.85391098186813,-15.3221582967889,11.));
#43903=CARTESIAN_POINT('Origin',(7.5,0.,15.3));
#43904=CARTESIAN_POINT('Origin',(7.5,0.,11.1));
#43905=CARTESIAN_POINT('Ctrl Pts',(-7.90064933695979,-2.15,11.));
#43906=CARTESIAN_POINT('Ctrl Pts',(-7.95822464412947,-2.09990411772952,
11.0500958822705));
#43907=CARTESIAN_POINT('Ctrl Pts',(-8.01579995129907,-2.04943366867993,
11.1005663313201));
#43908=CARTESIAN_POINT('',(3.95186632642215,-15.2443978869161,11.1018663264222));
#43909=CARTESIAN_POINT('Ctrl Pts',(3.95186632642215,-15.2443978869161,11.1018663264222));
#43910=CARTESIAN_POINT('Ctrl Pts',(3.90071701067554,-15.1799763945344,11.0507170106755));
#43911=CARTESIAN_POINT('Ctrl Pts',(3.85,-15.1155549021529,11.));
#43912=CARTESIAN_POINT('Ctrl Pts',(3.85391098186813,-15.3221582967889,11.2));
#43913=CARTESIAN_POINT('Ctrl Pts',(3.90304171380303,-15.2831565876938,11.1506841026818));
#43914=CARTESIAN_POINT('Ctrl Pts',(3.95186632642215,-15.2443978869161,11.1018663264222));
#43915=CARTESIAN_POINT('Origin',(3.75,-2.075,11.075));
#43916=CARTESIAN_POINT('',(-2.44929359829471E-16,-2.,11.15));
#43917=CARTESIAN_POINT('',(3.75,-2.,11.15));
#43918=CARTESIAN_POINT('',(-2.44929359829471E-16,-2.,11.15));
#43919=CARTESIAN_POINT('Origin',(3.33066907387547E-16,1.11022302462516E-15,
11.075));
#43920=CARTESIAN_POINT('Origin',(3.33066907387547E-16,1.11022302462516E-15,
11.15));
#43921=CARTESIAN_POINT('Origin',(3.33066907387547E-16,1.11022302462516E-15,
15.5));
#43922=CARTESIAN_POINT('',(-2.44929359829471E-16,-2.,15.4));
#43923=CARTESIAN_POINT('',(-2.44929359829471E-16,-2.,15.5));
#43924=CARTESIAN_POINT('Origin',(3.33066907387547E-16,1.11022302462516E-15,
15.4));
#43925=CARTESIAN_POINT('Origin',(-2.44929359829471E-16,-2.,15.5));
#43926=CARTESIAN_POINT('',(3.75,-2.,15.4));
#43927=CARTESIAN_POINT('Origin',(3.92695549093406,-15.2641729873626,11.));
#43928=CARTESIAN_POINT('',(3.9768743850762,-15.2245456072889,15.4231256149238));
#43929=CARTESIAN_POINT('Ctrl Pts',(3.9768743850762,-15.2245456072889,15.4231256149238));
#43930=CARTESIAN_POINT('Ctrl Pts',(3.91563394307748,-15.2731604316489,15.3619555845659));
#43931=CARTESIAN_POINT('Ctrl Pts',(3.85391098186813,-15.3221582967889,15.3));
#43932=CARTESIAN_POINT('',(4.,-15.2061876779362,11.15));
#43933=CARTESIAN_POINT('',(4.95122255935958,-14.4510736366054,12.1012225593596));
#43934=CARTESIAN_POINT('',(4.,-15.2061876779362,15.4));
#43935=CARTESIAN_POINT('',(4.,-15.2061876779362,11.));
#43936=CARTESIAN_POINT('',(5.82568926143346,-13.756891103911,13.5743107385665));
#43937=CARTESIAN_POINT('Origin',(3.95,-8.375,15.45));
#43938=CARTESIAN_POINT('',(4.,-7.5,15.4));
#43939=CARTESIAN_POINT('',(4.,-8.375,15.4));
#43940=CARTESIAN_POINT('',(3.9,-7.5,15.5));
#43941=CARTESIAN_POINT('',(4.,-7.5,15.4));
#43942=CARTESIAN_POINT('',(3.9,-15.0247296148716,15.5));
#43943=CARTESIAN_POINT('',(3.9,-8.375,15.5));
#43944=CARTESIAN_POINT('',(3.97071067811865,-15.2167906922565,15.4292893218813));
#43945=CARTESIAN_POINT('Ctrl Pts',(3.97071067811864,-15.2167906922566,15.4292893218815));
#43946=CARTESIAN_POINT('Ctrl Pts',(3.94710042961717,-15.152801460133,15.452899570383));
#43947=CARTESIAN_POINT('Ctrl Pts',(3.92352887530507,-15.08877879261,15.4764711246951));
#43948=CARTESIAN_POINT('Ctrl Pts',(3.89999999999998,-15.0247296148717,15.5000000000002));
#43949=CARTESIAN_POINT('Ctrl Pts',(3.97071067811865,-15.2167906922565,15.4292893218813));
#43950=CARTESIAN_POINT('Ctrl Pts',(3.97379174649682,-15.2206681497727,15.4262082535032));
#43951=CARTESIAN_POINT('Ctrl Pts',(3.9768743850762,-15.2245456072889,15.4231256149238));
#43952=CARTESIAN_POINT('Origin',(4.,-16.75,15.5));
#43953=CARTESIAN_POINT('',(4.,-7.5,11.15));
#43954=CARTESIAN_POINT('',(4.,-8.375,11.15));
#43955=CARTESIAN_POINT('',(4.,-7.5,15.5));
#43956=CARTESIAN_POINT('Origin',(3.925,-8.375,11.075));
#43957=CARTESIAN_POINT('',(4.,-7.5,11.15));
#43958=CARTESIAN_POINT('Origin',(11.0730445090659,-15.2641729873626,11.));
#43959=CARTESIAN_POINT('',(11.1460890181319,-15.3221582967889,15.3));
#43960=CARTESIAN_POINT('',(11.1460890181319,-15.3221582967889,11.));
#43961=CARTESIAN_POINT('',(11.0231256149238,-15.2245456072889,15.4231256149238));
#43962=CARTESIAN_POINT('Ctrl Pts',(11.1460890181319,-15.3221582967889,15.3));
#43963=CARTESIAN_POINT('Ctrl Pts',(11.084366056921,-15.2731604316477,15.3619555845674));
#43964=CARTESIAN_POINT('Ctrl Pts',(11.0231256149238,-15.2245456072889,15.4231256149238));
#43965=CARTESIAN_POINT('',(11.,-15.2061876779362,15.4));
#43966=CARTESIAN_POINT('',(8.47635547471623,-13.2028295809074,12.8763554747162));
#43967=CARTESIAN_POINT('',(11.,-15.2061876779362,11.15));
#43968=CARTESIAN_POINT('',(11.,-15.2061876779362,11.));
#43969=CARTESIAN_POINT('',(9.35082217679008,-13.8970121136018,12.7991778232099));
#43970=CARTESIAN_POINT('Origin',(7.5,0.,11.));
#43971=CARTESIAN_POINT('Origin',(7.5,0.,15.3));
#43972=CARTESIAN_POINT('Origin',(11.075,-3.75,11.075));
#43973=CARTESIAN_POINT('',(11.,-7.5,11.15));
#43974=CARTESIAN_POINT('',(11.,-3.75,11.15));
#43975=CARTESIAN_POINT('',(11.,-7.5,11.15));
#43976=CARTESIAN_POINT('Origin',(7.5,-7.5,11.075));
#43977=CARTESIAN_POINT('Origin',(7.5,-7.5,11.15));
#43978=CARTESIAN_POINT('Origin',(7.5,-7.5,15.5));
#43979=CARTESIAN_POINT('',(11.,-7.5,15.4));
#43980=CARTESIAN_POINT('',(11.,-7.5,15.5));
#43981=CARTESIAN_POINT('Origin',(7.5,-7.5,15.4));
#43982=CARTESIAN_POINT('Origin',(11.,-7.5,15.5));
#43983=CARTESIAN_POINT('',(11.,-3.75,15.4));
#43984=CARTESIAN_POINT('Origin',(7.5,-4.78246333309122E-16,15.4646446609407));
#43985=CARTESIAN_POINT('Origin',(7.5,0.,15.5));
#43986=CARTESIAN_POINT('Origin',(7.5,-9.56492666618245E-16,15.4292893218813));
#43987=CARTESIAN_POINT('Origin',(7.5,-4.78246333309122E-16,15.4646446609407));
#43988=CARTESIAN_POINT('',(-7.9883371262892,-2.02928932188134,15.4292893218813));
#43989=CARTESIAN_POINT('Origin',(7.5,-9.56492666618245E-16,15.4292893218813));
#43990=CARTESIAN_POINT('',(-7.80661621652546,-2.1,15.5));
#43991=CARTESIAN_POINT('Origin',(7.5,0.,15.5));
#43992=CARTESIAN_POINT('Ctrl Pts',(-7.80661621652547,-2.1,15.5));
#43993=CARTESIAN_POINT('Ctrl Pts',(-7.86721103212863,-2.07645911131055,
15.4764591113106));
#43994=CARTESIAN_POINT('Ctrl Pts',(-7.92778701650677,-2.05288762137709,
15.4528876213771));
#43995=CARTESIAN_POINT('Ctrl Pts',(-7.98833712628922,-2.02928932188135,
15.4292893218814));
#43996=CARTESIAN_POINT('Origin',(7.5,-4.78246333309122E-16,15.4646446609407));
#43997=CARTESIAN_POINT('',(22.6848608818125,2.85,15.5));
#43998=CARTESIAN_POINT('Origin',(7.5,0.,15.5));
#43999=CARTESIAN_POINT('Ctrl Pts',(22.6848608818124,2.84999999999997,15.5));
#44000=CARTESIAN_POINT('Ctrl Pts',(22.7470894475593,2.82646471883652,15.4764647188366));
#44001=CARTESIAN_POINT('Ctrl Pts',(22.8092954963163,2.80289320050296,15.452893200503));
#44002=CARTESIAN_POINT('Ctrl Pts',(22.8714720490512,2.77928932188132,15.4292893218814));
#44003=CARTESIAN_POINT('Origin',(7.5,-4.78246333309122E-16,15.4646446609407));
#44004=CARTESIAN_POINT('',(11.0292893218813,-15.2167906922565,15.4292893218813));
#44005=CARTESIAN_POINT('Origin',(7.5,-9.56492666618245E-16,15.4292893218813));
#44006=CARTESIAN_POINT('',(11.1,-15.0247296148716,15.5));
#44007=CARTESIAN_POINT('Origin',(7.5,0.,15.5));
#44008=CARTESIAN_POINT('Ctrl Pts',(11.1,-15.0247296148717,15.5000000000002));
#44009=CARTESIAN_POINT('Ctrl Pts',(11.0764711246955,-15.0887787926085,15.4764711246956));
#44010=CARTESIAN_POINT('Ctrl Pts',(11.0528995703839,-15.15280146013,15.4528995703841));
#44011=CARTESIAN_POINT('Ctrl Pts',(11.0292893218814,-15.2167906922566,15.4292893218815));
#44012=CARTESIAN_POINT('Origin',(15.,0.,15.45));
#44013=CARTESIAN_POINT('',(15.,2.85,15.5));
#44014=CARTESIAN_POINT('',(15.,2.75,15.4));
#44015=CARTESIAN_POINT('Origin',(15.,0.,15.5));
#44016=CARTESIAN_POINT('Origin',(11.25,2.8,15.45));
#44017=CARTESIAN_POINT('',(11.25,2.85,15.5));
#44018=CARTESIAN_POINT('Origin',(7.5,-7.5,15.45));
#44019=CARTESIAN_POINT('',(11.1,-7.5,15.5));
#44020=CARTESIAN_POINT('',(11.,-7.5,15.4));
#44021=CARTESIAN_POINT('Origin',(7.5,-7.5,15.5));
#44022=CARTESIAN_POINT('Origin',(11.05,-3.75,15.45));
#44023=CARTESIAN_POINT('Ctrl Pts',(11.0231256149238,-15.2245456072889,15.4231256149238));
#44024=CARTESIAN_POINT('Ctrl Pts',(11.0262082535032,-15.2206681497727,15.4262082535032));
#44025=CARTESIAN_POINT('Ctrl Pts',(11.0292893218813,-15.2167906922565,15.4292893218813));
#44026=CARTESIAN_POINT('',(11.1,-3.75,15.5));
#44027=CARTESIAN_POINT('Origin',(7.5,7.5,15.45));
#44028=CARTESIAN_POINT('Origin',(7.5,7.5,15.5));
#44029=CARTESIAN_POINT('Origin',(7.5,7.5,15.4));
#44030=CARTESIAN_POINT('Origin',(3.33066907387547E-16,1.11022302462516E-15,
15.45));
#44031=CARTESIAN_POINT('',(2.40522482451567E-16,-2.1,15.5));
#44032=CARTESIAN_POINT('',(-2.44929359829471E-16,-2.,15.4));
#44033=CARTESIAN_POINT('Origin',(3.33066907387547E-16,1.11022302462516E-15,
15.5));
#44034=CARTESIAN_POINT('Origin',(3.75,-2.05,15.45));
#44035=CARTESIAN_POINT('Ctrl Pts',(-7.99388777632041,-2.02441760835096,
15.424417608351));
#44036=CARTESIAN_POINT('Ctrl Pts',(-7.99111245130481,-2.0268539015144,15.4268539015144));
#44037=CARTESIAN_POINT('Ctrl Pts',(-7.9883371262892,-2.02928932188134,15.4292893218813));
#44038=CARTESIAN_POINT('',(3.75,-2.1,15.5));
#44039=CARTESIAN_POINT('Origin',(7.5,0.,15.4));
#44040=CARTESIAN_POINT('Origin',(7.5,0.,15.4));
#44041=CARTESIAN_POINT('Origin',(7.5,0.,15.5));
#44042=CARTESIAN_POINT('',(5.395,-2.57788151220518E-16,15.5));
#44043=CARTESIAN_POINT('Origin',(7.5,0.,15.5));
#44044=CARTESIAN_POINT('Origin',(7.5,0.,15.45));
#44045=CARTESIAN_POINT('',(5.445,-2.51664917224781E-16,15.45));
#44046=CARTESIAN_POINT('Origin',(7.5,7.5,15.5));
#44047=CARTESIAN_POINT('',(8.75,7.5,15.5));
#44048=CARTESIAN_POINT('Origin',(8.75,16.75,15.5));
#44049=CARTESIAN_POINT('Origin',(7.5,0.,15.4));
#44050=CARTESIAN_POINT('Origin',(7.5,0.,15.3));
#44051=CARTESIAN_POINT('Origin',(7.5,0.,11.));
#44052=CARTESIAN_POINT('Origin',(7.5,0.,11.2));
#44053=CARTESIAN_POINT('Origin',(7.5,0.,11.1));
#44054=CARTESIAN_POINT('',(0.,0.,0.));
#44055=CARTESIAN_POINT('Origin',(9.35,0.,5.5));
#44056=CARTESIAN_POINT('',(5.65,-2.2655965784226E-16,5.5));
#44057=CARTESIAN_POINT('Origin',(7.5,0.,5.5));
#44058=CARTESIAN_POINT('Origin',(7.5,0.,5.575));
#44059=CARTESIAN_POINT('',(5.5,-2.44929359829471E-16,5.65));
#44060=CARTESIAN_POINT('Origin',(7.5,0.,5.65));
#44061=CARTESIAN_POINT('',(5.575,-2.35744508835866E-16,5.575));
#44062=CARTESIAN_POINT('Origin',(7.5,0.,10.4));
#44063=CARTESIAN_POINT('',(5.5,-2.44929359829471E-16,15.15));
#44064=CARTESIAN_POINT('Origin',(7.5,0.,15.15));
#44065=CARTESIAN_POINT('',(5.5,-2.44929359829471E-16,10.4));
#44066=CARTESIAN_POINT('Origin',(7.5,0.,15.225));
#44067=CARTESIAN_POINT('',(5.65,-2.2655965784226E-16,15.3));
#44068=CARTESIAN_POINT('Origin',(7.5,0.,15.3));
#44069=CARTESIAN_POINT('',(5.575,-2.35744508835866E-16,15.225));
#44070=CARTESIAN_POINT('Origin',(7.5,0.,15.3));
#44071=CARTESIAN_POINT('',(0.,0.,0.));
#44072=CARTESIAN_POINT('Ctrl Pts',(8.35603499314338,15.8,85.4390826561945));
#44073=CARTESIAN_POINT('Ctrl Pts',(8.35603499314338,15.9372797480275,85.4390826561945));
#44074=CARTESIAN_POINT('Ctrl Pts',(8.39668257439119,16.1218710106354,85.4444904181629));
#44075=CARTESIAN_POINT('Ctrl Pts',(8.48962600103117,16.2884083933886,85.4549757803719));
#44076=CARTESIAN_POINT('Ctrl Pts',(8.51904255235788,16.333616011952,85.4581256707728));
#44077=CARTESIAN_POINT('Ctrl Pts',(8.53434287032992,16.3557032208687,85.4597347029858));
#44078=CARTESIAN_POINT('Ctrl Pts',(8.55014120211907,16.3772240255913,85.4613625335412));
#44079=CARTESIAN_POINT('Ctrl Pts',(8.60474859865648,16.4472645215626,85.4668665636608));
#44080=CARTESIAN_POINT('Ctrl Pts',(8.66423709283022,16.5065301286674,85.472314639594));
#44081=CARTESIAN_POINT('Ctrl Pts',(8.73421571262732,16.5611896429675,85.477810600089));
#44082=CARTESIAN_POINT('Ctrl Pts',(8.76289021098275,16.5822842616593,85.4799785377766));
#44083=CARTESIAN_POINT('Ctrl Pts',(8.80015375962284,16.6073660501337,85.4826344158676));
#44084=CARTESIAN_POINT('Ctrl Pts',(8.84680287582055,16.6350364303463,85.4856715584966));
#44085=CARTESIAN_POINT('Ctrl Pts',(8.91126359072523,16.6684953457075,85.489460606674));
#44086=CARTESIAN_POINT('Ctrl Pts',(8.97879268762966,16.6964087072018,85.4927632839475));
#44087=CARTESIAN_POINT('Ctrl Pts',(9.04794555696647,16.7183902183462,85.4954326308204));
#44088=CARTESIAN_POINT('Ctrl Pts',(9.22435588573701,16.7630993137503,85.5009743602204));
#44089=CARTESIAN_POINT('Ctrl Pts',(9.37978678214075,16.7631990287376,85.5009941213014));
#44090=CARTESIAN_POINT('Ctrl Pts',(9.52362841368894,16.7304680703605,85.4969281164271));
#44091=CARTESIAN_POINT('Ctrl Pts',(9.52948187007311,16.7291027348195,85.4967587924218));
#44092=CARTESIAN_POINT('Ctrl Pts',(9.53972603545934,16.7266396251387,85.4964537623072));
#44093=CARTESIAN_POINT('Ctrl Pts',(9.55140693128475,16.7236542968834,85.4960853644285));
#44094=CARTESIAN_POINT('Ctrl Pts',(9.56305629792811,16.7204997032745,85.4956975301883));
#44095=CARTESIAN_POINT('Ctrl Pts',(9.5746828868594,16.7172323247418,85.4952968805524));
#44096=CARTESIAN_POINT('Ctrl Pts',(9.6065596797669,16.7077838948382,85.4941429373237));
#44097=CARTESIAN_POINT('Ctrl Pts',(9.65813475370038,16.6898037484486,85.4919764613753));
#44098=CARTESIAN_POINT('Ctrl Pts',(9.72483636139708,16.6606586538393,85.4885662989555));
#44099=CARTESIAN_POINT('Ctrl Pts',(9.81035193883595,16.6152393568737,85.4834442118835));
#44100=CARTESIAN_POINT('Ctrl Pts',(9.88952955214136,16.5608297157303,85.477681416797));
#44101=CARTESIAN_POINT('Ctrl Pts',(9.96015984107354,16.4995598748089,85.4717656307727));
#44102=CARTESIAN_POINT('Ctrl Pts',(10.0566824559075,16.4030718438372,85.4630358281122));
#44103=CARTESIAN_POINT('Ctrl Pts',(10.140445547261,16.2824959491676,85.4539873067033));
#44104=CARTESIAN_POINT('Ctrl Pts',(10.1985441116753,16.1489861273042,85.4471485778523));
#44105=CARTESIAN_POINT('Ctrl Pts',(10.222497181123,16.0801829715165,85.4442465721495));
#44106=CARTESIAN_POINT('Ctrl Pts',(10.2411110001271,16.0101477612633,85.441938174718));
#44107=CARTESIAN_POINT('Ctrl Pts',(10.2671411860703,15.8682847284844,85.4386400439914));
#44108=CARTESIAN_POINT('Ctrl Pts',(10.2676702177296,15.7087996732268,85.4385975861224));
#44109=CARTESIAN_POINT('Ctrl Pts',(10.2253511275564,15.5187131618124,85.4439361201402));
#44110=CARTESIAN_POINT('Ctrl Pts',(10.1635097686491,15.3605723341138,85.4513910623746));
#44111=CARTESIAN_POINT('Ctrl Pts',(10.0582364282556,15.1952877308291,85.4629318702328));
#44112=CARTESIAN_POINT('Ctrl Pts',(9.93758658799873,15.0752327539855,85.4740118542376));
#44113=CARTESIAN_POINT('Ctrl Pts',(9.82095295951565,14.9912740599348,85.4827275167418));
#44114=CARTESIAN_POINT('Ctrl Pts',(9.7257726708022,14.938502416334,85.48864489927));
#44115=CARTESIAN_POINT('Ctrl Pts',(9.64154714023013,14.9035142378301,85.4927752312384));
#44116=CARTESIAN_POINT('Ctrl Pts',(9.58527096084076,14.8856853198025,85.4949434208681));
#44117=CARTESIAN_POINT('Ctrl Pts',(9.55910119355026,14.8783947067353,85.4958378446216));
#44118=CARTESIAN_POINT('Ctrl Pts',(9.54597200279266,14.8749411777993,85.4962632794556));
#44119=CARTESIAN_POINT('Ctrl Pts',(9.53283457660932,14.8716784688763,85.4966665696332));
#44120=CARTESIAN_POINT('Ctrl Pts',(9.45354917166566,14.8532449033689,85.4989535397092));
#44121=CARTESIAN_POINT('Ctrl Pts',(9.31002212387416,14.8376927917007,85.5009593430419));
#44122=CARTESIAN_POINT('Ctrl Pts',(9.15304234143535,14.8547157047969,85.4987606437473));
#44123=CARTESIAN_POINT('Ctrl Pts',(9.04735019561901,14.8816229494821,85.4954334077506));
#44124=CARTESIAN_POINT('Ctrl Pts',(8.97819116088274,14.903593487749,85.4927637202553));
#44125=CARTESIAN_POINT('Ctrl Pts',(8.89391110377091,14.9384727132614,85.4886374013684));
#44126=CARTESIAN_POINT('Ctrl Pts',(8.81450469736164,14.9826783322091,85.4836911519947));
#44127=CARTESIAN_POINT('Ctrl Pts',(8.75499655724527,15.0226900205634,85.4794515057453));
#44128=CARTESIAN_POINT('Ctrl Pts',(8.66971693517491,15.0875063099098,85.4728628549599));
#44129=CARTESIAN_POINT('Ctrl Pts',(8.60739958396077,15.1498071578507,85.4671368089765));
#44130=CARTESIAN_POINT('Ctrl Pts',(8.55799266459696,15.2123260535644,85.4621833875471));
#44131=CARTESIAN_POINT('Ctrl Pts',(8.54720257389172,15.2263954689324,85.4610892717717));
#44132=CARTESIAN_POINT('Ctrl Pts',(8.52873347530619,15.2515214314165,85.4591853935954));
#44133=CARTESIAN_POINT('Ctrl Pts',(8.49372813179311,15.3037099876317,85.4554712250094));
#44134=CARTESIAN_POINT('Ctrl Pts',(8.39640281859525,15.4781780558787,85.4444905178981));
#44135=CARTESIAN_POINT('Ctrl Pts',(8.35603499314338,15.6627202519725,85.4390826561945));
#44136=CARTESIAN_POINT('Ctrl Pts',(8.35603499314338,15.8,85.4390826561945));
#44137=CARTESIAN_POINT('Ctrl Pts',(8.40568999542892,15.8,85.3949461660668));
#44138=CARTESIAN_POINT('Ctrl Pts',(8.40568999542892,15.9308326910989,85.3949461660668));
#44139=CARTESIAN_POINT('Ctrl Pts',(8.44474272963522,16.1067243580164,85.3998613101596));
#44140=CARTESIAN_POINT('Ctrl Pts',(8.53356913858795,16.2648067705402,85.4093648382305));
#44141=CARTESIAN_POINT('Ctrl Pts',(8.56164483771783,16.3076765997574,85.4122177047785));
#44142=CARTESIAN_POINT('Ctrl Pts',(8.57624129470615,16.3286119068441,85.4136746517426));
#44143=CARTESIAN_POINT('Ctrl Pts',(8.59130554481547,16.349001315578,85.4151482154668));
#44144=CARTESIAN_POINT('Ctrl Pts',(8.64334979487582,16.4153281666897,85.420129275667));
#44145=CARTESIAN_POINT('Ctrl Pts',(8.69993120799356,16.4713215409808,85.4250535045443));
#44146=CARTESIAN_POINT('Ctrl Pts',(8.76632846975484,16.5228636831985,85.4300144910158));
#44147=CARTESIAN_POINT('Ctrl Pts',(8.79352158354697,16.5427454911753,85.4319708237179));
#44148=CARTESIAN_POINT('Ctrl Pts',(8.82883414057959,16.5663683097786,85.4343664168167));
#44149=CARTESIAN_POINT('Ctrl Pts',(8.87299808292085,16.5924050133844,85.4371043307198));
#44150=CARTESIAN_POINT('Ctrl Pts',(8.93396931795387,16.6238611980788,85.4405182224936));
#44151=CARTESIAN_POINT('Ctrl Pts',(8.9977612650961,16.650069132683,85.4434914376289));
#44152=CARTESIAN_POINT('Ctrl Pts',(9.06301962035174,16.6706899553159,85.4458931740141));
#44153=CARTESIAN_POINT('Ctrl Pts',(9.22939703062867,16.7126018503172,85.450877074459));
#44154=CARTESIAN_POINT('Ctrl Pts',(9.37567654308211,16.7126937732917,85.450894746136));
#44155=CARTESIAN_POINT('Ctrl Pts',(9.5113086780914,16.6820130652668,85.447238215881));
#44156=CARTESIAN_POINT('Ctrl Pts',(9.51682828834093,16.6807331755622,85.4470859379221));
#44157=CARTESIAN_POINT('Ctrl Pts',(9.52648877180839,16.6784240983265,85.4468116069232));
#44158=CARTESIAN_POINT('Ctrl Pts',(9.53750552568468,16.6756251154288,85.4464802597071));
#44159=CARTESIAN_POINT('Ctrl Pts',(9.5484940380417,16.6726670462954,85.4461314016811));
#44160=CARTESIAN_POINT('Ctrl Pts',(9.55946209396692,16.6696029422388,85.4457709954931));
#44161=CARTESIAN_POINT('Ctrl Pts',(9.58953773286542,16.6607411172119,85.4447328699376));
#44162=CARTESIAN_POINT('Ctrl Pts',(9.63822376367679,16.6438696842517,85.4427832798092));
#44163=CARTESIAN_POINT('Ctrl Pts',(9.70125198646232,16.6164958184463,85.4397126409855));
#44164=CARTESIAN_POINT('Ctrl Pts',(9.7821498111748,16.5737901734561,85.435097370155));
#44165=CARTESIAN_POINT('Ctrl Pts',(9.85719664323122,16.5225446594837,85.4298991149593));
#44166=CARTESIAN_POINT('Ctrl Pts',(9.92427648325852,16.4647182760809,85.4245561933527));
#44167=CARTESIAN_POINT('Ctrl Pts',(10.0160651871645,16.3735429235342,85.4166660324392));
#44168=CARTESIAN_POINT('Ctrl Pts',(10.0960218795394,16.2592652524798,85.4084709487996));
#44169=CARTESIAN_POINT('Ctrl Pts',(10.1516154183529,16.1323600396269,85.4022682199982));
#44170=CARTESIAN_POINT('Ctrl Pts',(10.174555475083,16.0669058752731,85.3996349002206));
#44171=CARTESIAN_POINT('Ctrl Pts',(10.1923954028737,16.0002310501117,85.3975393727227));
#44172=CARTESIAN_POINT('Ctrl Pts',(10.2173610140913,15.8651024456785,85.3945442463104));
#44173=CARTESIAN_POINT('Ctrl Pts',(10.21786262709,15.7130489813637,85.3945060111475));
#44174=CARTESIAN_POINT('Ctrl Pts',(10.1772803096206,15.5320202482537,85.3993536913281));
#44175=CARTESIAN_POINT('Ctrl Pts',(10.1180642105147,15.3816292809796,85.4061177055654));
#44176=CARTESIAN_POINT('Ctrl Pts',(10.0175327140903,15.2248716877216,85.4165730172062));
#44177=CARTESIAN_POINT('Ctrl Pts',(9.90277676210439,15.1114513230244,85.4265874895966));
#44178=CARTESIAN_POINT('Ctrl Pts',(9.79218928037887,15.0323392040438,85.4344512288155));
#44179=CARTESIAN_POINT('Ctrl Pts',(9.7021216365312,14.982710988249,85.4397838923364));
#44180=CARTESIAN_POINT('Ctrl Pts',(9.62255624266952,14.9498587840303,85.4435022587664));
#44181=CARTESIAN_POINT('Ctrl Pts',(9.5694496368992,14.9331342462661,85.4454530300753));
#44182=CARTESIAN_POINT('Ctrl Pts',(9.54476270274329,14.9262973372286,85.4462576016557));
#44183=CARTESIAN_POINT('Ctrl Pts',(9.53237917313348,14.9230591782846,85.4466402647976));
#44184=CARTESIAN_POINT('Ctrl Pts',(9.51998948264082,14.9200003032379,85.4470029819006));
#44185=CARTESIAN_POINT('Ctrl Pts',(9.44522624547653,14.9027206181603,85.4490596970557));
#44186=CARTESIAN_POINT('Ctrl Pts',(9.31001995354237,14.888162924871,85.4508618929458));
#44187=CARTESIAN_POINT('Ctrl Pts',(9.16214069815493,14.9040969243232,85.4488863553164));
#44188=CARTESIAN_POINT('Ctrl Pts',(9.06245933788975,14.9293229082359,85.4458938636106));
#44189=CARTESIAN_POINT('Ctrl Pts',(8.9971950546273,14.9499329681114,85.4434918584837));
#44190=CARTESIAN_POINT('Ctrl Pts',(8.9175790894704,14.9826813768387,85.4397771417074));
#44191=CARTESIAN_POINT('Ctrl Pts',(8.84243666780698,15.0242555638747,85.4353195904802));
#44192=CARTESIAN_POINT('Ctrl Pts',(8.78604443295927,15.0619394025398,85.431495454472));
#44193=CARTESIAN_POINT('Ctrl Pts',(8.70514823333775,15.1230441827598,85.4255490150097));
#44194=CARTESIAN_POINT('Ctrl Pts',(8.64587417668115,15.1819052888515,85.4203735430612));
#44195=CARTESIAN_POINT('Ctrl Pts',(8.59879194533658,15.2411027726911,85.4158910836619));
#44196=CARTESIAN_POINT('Ctrl Pts',(8.58850699900074,15.2544279222765,85.4149008595262));
#44197=CARTESIAN_POINT('Ctrl Pts',(8.57089587702538,15.2782326333794,85.4131773950912));
#44198=CARTESIAN_POINT('Ctrl Pts',(8.53749381124016,15.3277115849179,85.4098139059006));
#44199=CARTESIAN_POINT('Ctrl Pts',(8.44447962066645,15.4933224411837,85.3998614319814));
#44200=CARTESIAN_POINT('Ctrl Pts',(8.40568999542892,15.6691673089011,85.3949461660668));
#44201=CARTESIAN_POINT('Ctrl Pts',(8.40568999542892,15.8,85.3949461660668));
#44202=CARTESIAN_POINT('Ctrl Pts',(8.45534499771446,15.8,85.3508096759391));
#44203=CARTESIAN_POINT('Ctrl Pts',(8.45534499771446,15.9243856341704,85.3508096759391));
#44204=CARTESIAN_POINT('Ctrl Pts',(8.49280288487924,16.0915777053974,85.3552322021562));
#44205=CARTESIAN_POINT('Ctrl Pts',(8.57751227614473,16.2412051476919,85.3637538960892));
#44206=CARTESIAN_POINT('Ctrl Pts',(8.60424712307778,16.2817371875628,85.3663097387841));
#44207=CARTESIAN_POINT('Ctrl Pts',(8.61813971908238,16.3015205928195,85.3676146004995));
#44208=CARTESIAN_POINT('Ctrl Pts',(8.63246988751186,16.3207786055647,85.3689338973923));
#44209=CARTESIAN_POINT('Ctrl Pts',(8.68195099109516,16.3833918118167,85.3733919876731));
#44210=CARTESIAN_POINT('Ctrl Pts',(8.7356253231569,16.4361129532943,85.3777923694946));
#44211=CARTESIAN_POINT('Ctrl Pts',(8.79844122688236,16.4845377234294,85.3822183819425));
#44212=CARTESIAN_POINT('Ctrl Pts',(8.82415295611118,16.5032067206913,85.3839631096591));
#44213=CARTESIAN_POINT('Ctrl Pts',(8.85751452153635,16.5253705694234,85.3860984177658));
#44214=CARTESIAN_POINT('Ctrl Pts',(8.89919329002115,16.5497735964226,85.3885371029431));
#44215=CARTESIAN_POINT('Ctrl Pts',(8.95667504518251,16.5792270504501,85.3915758383132));
#44216=CARTESIAN_POINT('Ctrl Pts',(9.01672984256254,16.6037295581642,85.3942195913102));
#44217=CARTESIAN_POINT('Ctrl Pts',(9.07809368373701,16.6229896922856,85.3963537172078));
#44218=CARTESIAN_POINT('Ctrl Pts',(9.23443817552033,16.6621043868841,85.4007797886977));
#44219=CARTESIAN_POINT('Ctrl Pts',(9.37156630402344,16.6621885178458,85.4007953709705));
#44220=CARTESIAN_POINT('Ctrl Pts',(9.49898894249385,16.633558060173,85.397548315335));
#44221=CARTESIAN_POINT('Ctrl Pts',(9.50417470660875,16.6323636163049,85.3974130834225));
#44222=CARTESIAN_POINT('Ctrl Pts',(9.51325150815744,16.6302085715143,85.3971694515393));
#44223=CARTESIAN_POINT('Ctrl Pts',(9.5236041200846,16.6275959339742,85.3968751549858));
#44224=CARTESIAN_POINT('Ctrl Pts',(9.53393177815528,16.6248343893163,85.3965652731739));
#44225=CARTESIAN_POINT('Ctrl Pts',(9.54424130107443,16.6219735597358,85.3962451104339));
#44226=CARTESIAN_POINT('Ctrl Pts',(9.57251578596394,16.6136983395856,85.3953228025516));
#44227=CARTESIAN_POINT('Ctrl Pts',(9.61831277365319,16.5979356200548,85.3935900982431));
#44228=CARTESIAN_POINT('Ctrl Pts',(9.67766761152756,16.5723329830534,85.3908589830154));
#44229=CARTESIAN_POINT('Ctrl Pts',(9.75394768351365,16.5323409900384,85.3867505284264));
#44230=CARTESIAN_POINT('Ctrl Pts',(9.82486373432107,16.4842596032372,85.3821168131216));
#44231=CARTESIAN_POINT('Ctrl Pts',(9.8883931254435,16.4298766773529,85.3773467559326));
#44232=CARTESIAN_POINT('Ctrl Pts',(9.97544791842136,16.3440140032313,85.3702962367661));
#44233=CARTESIAN_POINT('Ctrl Pts',(10.0515982118178,16.236034555792,85.362954590896));
#44234=CARTESIAN_POINT('Ctrl Pts',(10.1046867250305,16.1157339519497,85.3573878621441));
#44235=CARTESIAN_POINT('Ctrl Pts',(10.126613769043,16.0536287790298,85.3550232282919));
#44236=CARTESIAN_POINT('Ctrl Pts',(10.1436798056203,15.9903143389601,85.3531405707274));
#44237=CARTESIAN_POINT('Ctrl Pts',(10.1675808421122,15.8619201628725,85.3504484486294));
#44238=CARTESIAN_POINT('Ctrl Pts',(10.1680550364504,15.7172982895006,85.3504144361727));
#44239=CARTESIAN_POINT('Ctrl Pts',(10.1292094916849,15.5453273346951,85.3547712625161));
#44240=CARTESIAN_POINT('Ctrl Pts',(10.0726186523802,15.4026862278453,85.3608443487561));
#44241=CARTESIAN_POINT('Ctrl Pts',(9.97682899992489,15.2544556446141,85.3702141641797));
#44242=CARTESIAN_POINT('Ctrl Pts',(9.86796693621007,15.1476698920632,85.3791631249556));
#44243=CARTESIAN_POINT('Ctrl Pts',(9.76342560124209,15.0734043481528,85.3861749408892));
#44244=CARTESIAN_POINT('Ctrl Pts',(9.6784706022602,15.026919560164,85.3909228854027));
#44245=CARTESIAN_POINT('Ctrl Pts',(9.60356534510891,14.9962033302305,85.3942292862944));
#44246=CARTESIAN_POINT('Ctrl Pts',(9.55362831295764,14.9805831727297,85.3959626392824));
#44247=CARTESIAN_POINT('Ctrl Pts',(9.53042421193632,14.974199967722,85.3966773586898));
#44248=CARTESIAN_POINT('Ctrl Pts',(9.5187863434743,14.97117717877,85.3970172501395));
#44249=CARTESIAN_POINT('Ctrl Pts',(9.50714438867232,14.9683221375996,85.3973393941678));
#44250=CARTESIAN_POINT('Ctrl Pts',(9.43690331928739,14.9521963329518,85.3991658544022));
#44251=CARTESIAN_POINT('Ctrl Pts',(9.31001778321058,14.9386330580413,85.4007644428496));
#44252=CARTESIAN_POINT('Ctrl Pts',(9.17123905487452,14.9534781438495,85.3990120668856));
#44253=CARTESIAN_POINT('Ctrl Pts',(9.07756848016049,14.9770228669897,85.3963543194706));
#44254=CARTESIAN_POINT('Ctrl Pts',(9.01619894837186,14.9962724484738,85.394219996712));
#44255=CARTESIAN_POINT('Ctrl Pts',(8.9412470751699,15.026890040416,85.3909168820463));
#44256=CARTESIAN_POINT('Ctrl Pts',(8.87036863825231,15.0658327955402,85.3869480289657));
#44257=CARTESIAN_POINT('Ctrl Pts',(8.81709230867327,15.1011887845163,85.3835394031987));
#44258=CARTESIAN_POINT('Ctrl Pts',(8.74057953150059,15.1585820556098,85.3782351750594));
#44259=CARTESIAN_POINT('Ctrl Pts',(8.68434876940152,15.2140034198523,85.3736102771458));
#44260=CARTESIAN_POINT('Ctrl Pts',(8.63959122607621,15.2698794918178,85.3695987797766));
#44261=CARTESIAN_POINT('Ctrl Pts',(8.62981142410976,15.2824603756206,85.3687124472807));
#44262=CARTESIAN_POINT('Ctrl Pts',(8.61305827874456,15.3049438353424,85.367169396587));
#44263=CARTESIAN_POINT('Ctrl Pts',(8.58125949068721,15.3517131822041,85.3641565867918));
#44264=CARTESIAN_POINT('Ctrl Pts',(8.49255642273764,15.5084668264888,85.3552323460647));
#44265=CARTESIAN_POINT('Ctrl Pts',(8.45534499771446,15.6756143658296,85.3508096759391));
#44266=CARTESIAN_POINT('Ctrl Pts',(8.45534499771446,15.8,85.3508096759391));
#44267=CARTESIAN_POINT('Ctrl Pts',(8.505,15.8,85.3066731858115));
#44268=CARTESIAN_POINT('Ctrl Pts',(8.505,15.9179385772418,85.3066731858115));
#44269=CARTESIAN_POINT('Ctrl Pts',(8.54086304012327,16.0764310527784,85.3106030941529));
#44270=CARTESIAN_POINT('Ctrl Pts',(8.62145541370151,16.2176035248435,85.3181429539479));
#44271=CARTESIAN_POINT('Ctrl Pts',(8.64684940843773,16.2557977753682,85.3204017727898));
#44272=CARTESIAN_POINT('Ctrl Pts',(8.66003814345861,16.2744292787949,85.3215545492563));
#44273=CARTESIAN_POINT('Ctrl Pts',(8.67363423020825,16.2925558955514,85.3227195793178));
#44274=CARTESIAN_POINT('Ctrl Pts',(8.7205521873145,16.3514554569438,85.3266546996792));
#44275=CARTESIAN_POINT('Ctrl Pts',(8.77131943832023,16.4009043656078,85.3305312344449));
#44276=CARTESIAN_POINT('Ctrl Pts',(8.83055398400987,16.4462117636603,85.3344222728693));
#44277=CARTESIAN_POINT('Ctrl Pts',(8.8547843286754,16.4636679502074,85.3359553956004));
#44278=CARTESIAN_POINT('Ctrl Pts',(8.8861949024931,16.4843728290683,85.3378304187148));
#44279=CARTESIAN_POINT('Ctrl Pts',(8.92538849712145,16.5071421794607,85.3399698751664));
#44280=CARTESIAN_POINT('Ctrl Pts',(8.97938077241115,16.5345929028214,85.3426334541328));
#44281=CARTESIAN_POINT('Ctrl Pts',(9.03569842002898,16.5573899836454,85.3449477449916));
#44282=CARTESIAN_POINT('Ctrl Pts',(9.09316774712228,16.5752894292553,85.3468142604014));
#44283=CARTESIAN_POINT('Ctrl Pts',(9.23947932041198,16.611606923451,85.3506825029363));
#44284=CARTESIAN_POINT('Ctrl Pts',(9.36745606496479,16.6116832623999,85.3506959958052));
#44285=CARTESIAN_POINT('Ctrl Pts',(9.4866692068963,16.5851030550793,85.3478584147889));
#44286=CARTESIAN_POINT('Ctrl Pts',(9.49152112487657,16.5839940570477,85.3477402289228));
#44287=CARTESIAN_POINT('Ctrl Pts',(9.50001424450649,16.581993044702,85.3475272961553));
#44288=CARTESIAN_POINT('Ctrl Pts',(9.50970271448452,16.5795667525196,85.3472700502645));
#44289=CARTESIAN_POINT('Ctrl Pts',(9.51936951826886,16.5770017323372,85.3469991446667));
#44290=CARTESIAN_POINT('Ctrl Pts',(9.52902050818195,16.5743441772328,85.3467192253746));
#44291=CARTESIAN_POINT('Ctrl Pts',(9.55549383906246,16.5666555619593,85.3459127351656));
#44292=CARTESIAN_POINT('Ctrl Pts',(9.59840178362959,16.5520015558579,85.344396916677));
#44293=CARTESIAN_POINT('Ctrl Pts',(9.6540832365928,16.5281701476604,85.3420053250454));
#44294=CARTESIAN_POINT('Ctrl Pts',(9.72574555585249,16.4908918066207,85.3384036866979));
#44295=CARTESIAN_POINT('Ctrl Pts',(9.79253082541093,16.4459745469907,85.3343345112839));
#44296=CARTESIAN_POINT('Ctrl Pts',(9.85250976762847,16.3950350786248,85.3301373185125));
#44297=CARTESIAN_POINT('Ctrl Pts',(9.93483064967827,16.3144850829283,85.3239264410931));
#44298=CARTESIAN_POINT('Ctrl Pts',(10.0071745440962,16.2128038591041,85.3174382329924));
#44299=CARTESIAN_POINT('Ctrl Pts',(10.057758031708,16.0991078642724,85.3125075042899));
#44300=CARTESIAN_POINT('Ctrl Pts',(10.078672063003,16.0403516827864,85.3104115563631));
#44301=CARTESIAN_POINT('Ctrl Pts',(10.0949642083669,15.9803976278085,85.3087417687321));
#44302=CARTESIAN_POINT('Ctrl Pts',(10.1178006701332,15.8587378800666,85.3063526509483));
#44303=CARTESIAN_POINT('Ctrl Pts',(10.1182474458107,15.7215475976374,85.3063228611977));
#44304=CARTESIAN_POINT('Ctrl Pts',(10.0811386737492,15.5586344211364,85.310188833704));
#44305=CARTESIAN_POINT('Ctrl Pts',(10.0271730942457,15.4237431747111,85.3155709919468));
#44306=CARTESIAN_POINT('Ctrl Pts',(9.93612528575951,15.2840396015067,85.3238553111532));
#44307=CARTESIAN_POINT('Ctrl Pts',(9.83315711031573,15.1838884611021,85.3317387603146));
#44308=CARTESIAN_POINT('Ctrl Pts',(9.7346619221053,15.1144694922618,85.3378986529629));
#44309=CARTESIAN_POINT('Ctrl Pts',(9.6548195679892,15.0711281320789,85.342061878469));
#44310=CARTESIAN_POINT('Ctrl Pts',(9.5845744475483,15.0425478764307,85.3449563138224));
#44311=CARTESIAN_POINT('Ctrl Pts',(9.53780698901607,15.0280320991933,85.3464722484895));
#44312=CARTESIAN_POINT('Ctrl Pts',(9.51608572112935,15.0221025982153,85.3470971157239));
#44313=CARTESIAN_POINT('Ctrl Pts',(9.50519351381511,15.0192951792553,85.3473942354814));
#44314=CARTESIAN_POINT('Ctrl Pts',(9.49429929470381,15.0166439719612,85.3476758064351));
#44315=CARTESIAN_POINT('Ctrl Pts',(9.42858039309825,15.0016720477432,85.3492720117487));
#44316=CARTESIAN_POINT('Ctrl Pts',(9.31001561287879,14.9891031912116,85.3506669927535));
#44317=CARTESIAN_POINT('Ctrl Pts',(9.1803374115941,15.0028593633758,85.3491377784547));
#44318=CARTESIAN_POINT('Ctrl Pts',(9.09267762243124,15.0247228257435,85.3468147753307));
#44319=CARTESIAN_POINT('Ctrl Pts',(9.03520284211642,15.0426119288362,85.3449481349403));
#44320=CARTESIAN_POINT('Ctrl Pts',(8.96491506086939,15.0710987039933,85.3420566223853));
#44321=CARTESIAN_POINT('Ctrl Pts',(8.89830060869765,15.1074100272057,85.3385764674512));
#44322=CARTESIAN_POINT('Ctrl Pts',(8.84814018438728,15.1404381664927,85.3355833519254));
#44323=CARTESIAN_POINT('Ctrl Pts',(8.77601082966343,15.1941199284598,85.3309213351092));
#44324=CARTESIAN_POINT('Ctrl Pts',(8.7228233621219,15.246101550853,85.3268470112305));
#44325=CARTESIAN_POINT('Ctrl Pts',(8.68039050681583,15.2986562109445,85.3233064758915));
#44326=CARTESIAN_POINT('Ctrl Pts',(8.67111584921878,15.3104928289646,85.3225240350353));
#44327=CARTESIAN_POINT('Ctrl Pts',(8.65522068046374,15.3316550373053,85.3211613980828));
#44328=CARTESIAN_POINT('Ctrl Pts',(8.62502517013426,15.3757147794904,85.3184992676831));
#44329=CARTESIAN_POINT('Ctrl Pts',(8.54063322480884,15.5236112117938,85.310603260148));
#44330=CARTESIAN_POINT('Ctrl Pts',(8.505,15.6820614227582,85.3066731858115));
#44331=CARTESIAN_POINT('Ctrl Pts',(8.505,15.8,85.3066731858115));
#44332=CARTESIAN_POINT('',(8.35603499314338,15.8,85.4390826561945));
#44333=CARTESIAN_POINT('',(8.505,15.8,85.3066731858115));
#44334=CARTESIAN_POINT('',(8.35603499314338,15.8,85.4390826561945));
#44335=CARTESIAN_POINT('Ctrl Pts',(8.505,15.8,85.3066731858115));
#44336=CARTESIAN_POINT('Ctrl Pts',(8.505,15.9179385772418,85.3066731858115));
#44337=CARTESIAN_POINT('Ctrl Pts',(8.54086304012327,16.0764310527784,85.3106030941529));
#44338=CARTESIAN_POINT('Ctrl Pts',(8.62145541370151,16.2176035248435,85.3181429539479));
#44339=CARTESIAN_POINT('Ctrl Pts',(8.64684940843773,16.2557977753682,85.3204017727898));
#44340=CARTESIAN_POINT('Ctrl Pts',(8.66003814345861,16.2744292787949,85.3215545492563));
#44341=CARTESIAN_POINT('Ctrl Pts',(8.67363423020825,16.2925558955514,85.3227195793178));
#44342=CARTESIAN_POINT('Ctrl Pts',(8.7205521873145,16.3514554569438,85.3266546996792));
#44343=CARTESIAN_POINT('Ctrl Pts',(8.77131943832023,16.4009043656078,85.3305312344449));
#44344=CARTESIAN_POINT('Ctrl Pts',(8.83055398400987,16.4462117636603,85.3344222728693));
#44345=CARTESIAN_POINT('Ctrl Pts',(8.8547843286754,16.4636679502074,85.3359553956004));
#44346=CARTESIAN_POINT('Ctrl Pts',(8.8861949024931,16.4843728290683,85.3378304187148));
#44347=CARTESIAN_POINT('Ctrl Pts',(8.92538849712145,16.5071421794607,85.3399698751664));
#44348=CARTESIAN_POINT('Ctrl Pts',(8.97938077241115,16.5345929028214,85.3426334541328));
#44349=CARTESIAN_POINT('Ctrl Pts',(9.03569842002898,16.5573899836454,85.3449477449916));
#44350=CARTESIAN_POINT('Ctrl Pts',(9.09316774712228,16.5752894292553,85.3468142604014));
#44351=CARTESIAN_POINT('Ctrl Pts',(9.23947932041198,16.611606923451,85.3506825029363));
#44352=CARTESIAN_POINT('Ctrl Pts',(9.36745606496479,16.6116832623999,85.3506959958052));
#44353=CARTESIAN_POINT('Ctrl Pts',(9.4866692068963,16.5851030550793,85.3478584147889));
#44354=CARTESIAN_POINT('Ctrl Pts',(9.49152112487657,16.5839940570477,85.3477402289228));
#44355=CARTESIAN_POINT('Ctrl Pts',(9.50001424450649,16.581993044702,85.3475272961553));
#44356=CARTESIAN_POINT('Ctrl Pts',(9.50970271448452,16.5795667525196,85.3472700502645));
#44357=CARTESIAN_POINT('Ctrl Pts',(9.51936951826886,16.5770017323372,85.3469991446667));
#44358=CARTESIAN_POINT('Ctrl Pts',(9.52902050818195,16.5743441772328,85.3467192253746));
#44359=CARTESIAN_POINT('Ctrl Pts',(9.55549383906246,16.5666555619593,85.3459127351656));
#44360=CARTESIAN_POINT('Ctrl Pts',(9.59840178362959,16.5520015558579,85.344396916677));
#44361=CARTESIAN_POINT('Ctrl Pts',(9.6540832365928,16.5281701476604,85.3420053250454));
#44362=CARTESIAN_POINT('Ctrl Pts',(9.72574555585249,16.4908918066207,85.3384036866979));
#44363=CARTESIAN_POINT('Ctrl Pts',(9.79253082541093,16.4459745469907,85.3343345112839));
#44364=CARTESIAN_POINT('Ctrl Pts',(9.85250976762847,16.3950350786248,85.3301373185125));
#44365=CARTESIAN_POINT('Ctrl Pts',(9.93483064967827,16.3144850829283,85.3239264410931));
#44366=CARTESIAN_POINT('Ctrl Pts',(10.0071745440962,16.2128038591041,85.3174382329924));
#44367=CARTESIAN_POINT('Ctrl Pts',(10.057758031708,16.0991078642724,85.3125075042899));
#44368=CARTESIAN_POINT('Ctrl Pts',(10.078672063003,16.0403516827864,85.3104115563631));
#44369=CARTESIAN_POINT('Ctrl Pts',(10.0949642083669,15.9803976278085,85.3087417687321));
#44370=CARTESIAN_POINT('Ctrl Pts',(10.1178006701332,15.8587378800666,85.3063526509483));
#44371=CARTESIAN_POINT('Ctrl Pts',(10.1182474458107,15.7215475976374,85.3063228611977));
#44372=CARTESIAN_POINT('Ctrl Pts',(10.0811386737492,15.5586344211364,85.310188833704));
#44373=CARTESIAN_POINT('Ctrl Pts',(10.0271730942457,15.4237431747111,85.3155709919468));
#44374=CARTESIAN_POINT('Ctrl Pts',(9.93612528575951,15.2840396015067,85.3238553111532));
#44375=CARTESIAN_POINT('Ctrl Pts',(9.83315711031573,15.1838884611021,85.3317387603146));
#44376=CARTESIAN_POINT('Ctrl Pts',(9.7346619221053,15.1144694922618,85.3378986529629));
#44377=CARTESIAN_POINT('Ctrl Pts',(9.6548195679892,15.0711281320789,85.342061878469));
#44378=CARTESIAN_POINT('Ctrl Pts',(9.5845744475483,15.0425478764307,85.3449563138224));
#44379=CARTESIAN_POINT('Ctrl Pts',(9.53780698901607,15.0280320991933,85.3464722484895));
#44380=CARTESIAN_POINT('Ctrl Pts',(9.51608572112935,15.0221025982153,85.3470971157239));
#44381=CARTESIAN_POINT('Ctrl Pts',(9.50519351381511,15.0192951792553,85.3473942354814));
#44382=CARTESIAN_POINT('Ctrl Pts',(9.49429929470381,15.0166439719612,85.3476758064351));
#44383=CARTESIAN_POINT('Ctrl Pts',(9.42858039309825,15.0016720477432,85.3492720117487));
#44384=CARTESIAN_POINT('Ctrl Pts',(9.31001561287879,14.9891031912116,85.3506669927535));
#44385=CARTESIAN_POINT('Ctrl Pts',(9.1803374115941,15.0028593633758,85.3491377784547));
#44386=CARTESIAN_POINT('Ctrl Pts',(9.09267762243124,15.0247228257435,85.3468147753307));
#44387=CARTESIAN_POINT('Ctrl Pts',(9.03520284211642,15.0426119288362,85.3449481349403));
#44388=CARTESIAN_POINT('Ctrl Pts',(8.96491506086939,15.0710987039933,85.3420566223853));
#44389=CARTESIAN_POINT('Ctrl Pts',(8.89830060869765,15.1074100272057,85.3385764674512));
#44390=CARTESIAN_POINT('Ctrl Pts',(8.84814018438728,15.1404381664927,85.3355833519254));
#44391=CARTESIAN_POINT('Ctrl Pts',(8.77601082966343,15.1941199284598,85.3309213351092));
#44392=CARTESIAN_POINT('Ctrl Pts',(8.7228233621219,15.246101550853,85.3268470112305));
#44393=CARTESIAN_POINT('Ctrl Pts',(8.68039050681583,15.2986562109445,85.3233064758915));
#44394=CARTESIAN_POINT('Ctrl Pts',(8.67111584921878,15.3104928289646,85.3225240350353));
#44395=CARTESIAN_POINT('Ctrl Pts',(8.65522068046374,15.3316550373053,85.3211613980828));
#44396=CARTESIAN_POINT('Ctrl Pts',(8.62502517013426,15.3757147794904,85.3184992676831));
#44397=CARTESIAN_POINT('Ctrl Pts',(8.54063322480884,15.5236112117938,85.310603260148));
#44398=CARTESIAN_POINT('Ctrl Pts',(8.505,15.6820614227582,85.3066731858115));
#44399=CARTESIAN_POINT('Ctrl Pts',(8.505,15.8,85.3066731858115));
#44400=CARTESIAN_POINT('Ctrl Pts',(8.35603499314338,15.8,85.4390826561945));
#44401=CARTESIAN_POINT('Ctrl Pts',(8.35603499314338,15.6627202519725,85.4390826561945));
#44402=CARTESIAN_POINT('Ctrl Pts',(8.39640281859525,15.4781780558787,85.4444905178981));
#44403=CARTESIAN_POINT('Ctrl Pts',(8.49372813179311,15.3037099876317,85.4554712250094));
#44404=CARTESIAN_POINT('Ctrl Pts',(8.52873347530619,15.2515214314165,85.4591853935954));
#44405=CARTESIAN_POINT('Ctrl Pts',(8.54720257389172,15.2263954689324,85.4610892717717));
#44406=CARTESIAN_POINT('Ctrl Pts',(8.55799266459696,15.2123260535644,85.4621833875471));
#44407=CARTESIAN_POINT('Ctrl Pts',(8.60739958396077,15.1498071578507,85.4671368089765));
#44408=CARTESIAN_POINT('Ctrl Pts',(8.66971693517491,15.0875063099098,85.4728628549599));
#44409=CARTESIAN_POINT('Ctrl Pts',(8.75499655724527,15.0226900205634,85.4794515057453));
#44410=CARTESIAN_POINT('Ctrl Pts',(8.81450469736164,14.9826783322091,85.4836911519947));
#44411=CARTESIAN_POINT('Ctrl Pts',(8.89391110377091,14.9384727132614,85.4886374013684));
#44412=CARTESIAN_POINT('Ctrl Pts',(8.97819116088274,14.903593487749,85.4927637202553));
#44413=CARTESIAN_POINT('Ctrl Pts',(9.04735019561901,14.8816229494821,85.4954334077506));
#44414=CARTESIAN_POINT('Ctrl Pts',(9.15304234143535,14.8547157047969,85.4987606437473));
#44415=CARTESIAN_POINT('Ctrl Pts',(9.31002212387416,14.8376927917007,85.5009593430419));
#44416=CARTESIAN_POINT('Ctrl Pts',(9.45354917166566,14.8532449033689,85.4989535397092));
#44417=CARTESIAN_POINT('Ctrl Pts',(9.53283457660932,14.8716784688763,85.4966665696332));
#44418=CARTESIAN_POINT('Ctrl Pts',(9.54597200279266,14.8749411777993,85.4962632794556));
#44419=CARTESIAN_POINT('Ctrl Pts',(9.55910119355026,14.8783947067353,85.4958378446216));
#44420=CARTESIAN_POINT('Ctrl Pts',(9.58527096084076,14.8856853198025,85.4949434208681));
#44421=CARTESIAN_POINT('Ctrl Pts',(9.64154714023013,14.9035142378301,85.4927752312384));
#44422=CARTESIAN_POINT('Ctrl Pts',(9.7257726708022,14.938502416334,85.48864489927));
#44423=CARTESIAN_POINT('Ctrl Pts',(9.82095295951565,14.9912740599348,85.4827275167418));
#44424=CARTESIAN_POINT('Ctrl Pts',(9.93758658799873,15.0752327539855,85.4740118542376));
#44425=CARTESIAN_POINT('Ctrl Pts',(10.0582364282556,15.1952877308291,85.4629318702328));
#44426=CARTESIAN_POINT('Ctrl Pts',(10.1635097686491,15.3605723341138,85.4513910623746));
#44427=CARTESIAN_POINT('Ctrl Pts',(10.2253511275564,15.5187131618124,85.4439361201402));
#44428=CARTESIAN_POINT('Ctrl Pts',(10.2676702177296,15.7087996732268,85.4385975861224));
#44429=CARTESIAN_POINT('Ctrl Pts',(10.2671411860703,15.8682847284844,85.4386400439914));
#44430=CARTESIAN_POINT('Ctrl Pts',(10.2411110001271,16.0101477612633,85.441938174718));
#44431=CARTESIAN_POINT('Ctrl Pts',(10.222497181123,16.0801829715165,85.4442465721495));
#44432=CARTESIAN_POINT('Ctrl Pts',(10.1985441116753,16.1489861273042,85.4471485778523));
#44433=CARTESIAN_POINT('Ctrl Pts',(10.140445547261,16.2824959491676,85.4539873067033));
#44434=CARTESIAN_POINT('Ctrl Pts',(10.0566824559075,16.4030718438372,85.4630358281122));
#44435=CARTESIAN_POINT('Ctrl Pts',(9.96015984107354,16.4995598748089,85.4717656307727));
#44436=CARTESIAN_POINT('Ctrl Pts',(9.88952955214136,16.5608297157303,85.477681416797));
#44437=CARTESIAN_POINT('Ctrl Pts',(9.81035193883595,16.6152393568737,85.4834442118835));
#44438=CARTESIAN_POINT('Ctrl Pts',(9.72483636139708,16.6606586538393,85.4885662989555));
#44439=CARTESIAN_POINT('Ctrl Pts',(9.65813475370038,16.6898037484486,85.4919764613753));
#44440=CARTESIAN_POINT('Ctrl Pts',(9.6065596797669,16.7077838948382,85.4941429373237));
#44441=CARTESIAN_POINT('Ctrl Pts',(9.5746828868594,16.7172323247418,85.4952968805524));
#44442=CARTESIAN_POINT('Ctrl Pts',(9.56305629792811,16.7204997032745,85.4956975301883));
#44443=CARTESIAN_POINT('Ctrl Pts',(9.55140693128475,16.7236542968834,85.4960853644285));
#44444=CARTESIAN_POINT('Ctrl Pts',(9.53972603545934,16.7266396251387,85.4964537623072));
#44445=CARTESIAN_POINT('Ctrl Pts',(9.52948187007311,16.7291027348195,85.4967587924218));
#44446=CARTESIAN_POINT('Ctrl Pts',(9.52362841368894,16.7304680703605,85.4969281164271));
#44447=CARTESIAN_POINT('Ctrl Pts',(9.37978678214075,16.7631990287376,85.5009941213014));
#44448=CARTESIAN_POINT('Ctrl Pts',(9.22435588573701,16.7630993137503,85.5009743602204));
#44449=CARTESIAN_POINT('Ctrl Pts',(9.04794555696647,16.7183902183462,85.4954326308204));
#44450=CARTESIAN_POINT('Ctrl Pts',(8.97879268762966,16.6964087072018,85.4927632839475));
#44451=CARTESIAN_POINT('Ctrl Pts',(8.91126359072523,16.6684953457075,85.489460606674));
#44452=CARTESIAN_POINT('Ctrl Pts',(8.84680287582055,16.6350364303463,85.4856715584966));
#44453=CARTESIAN_POINT('Ctrl Pts',(8.80015375962284,16.6073660501337,85.4826344158676));
#44454=CARTESIAN_POINT('Ctrl Pts',(8.76289021098275,16.5822842616593,85.4799785377766));
#44455=CARTESIAN_POINT('Ctrl Pts',(8.73421571262732,16.5611896429675,85.477810600089));
#44456=CARTESIAN_POINT('Ctrl Pts',(8.66423709283022,16.5065301286674,85.472314639594));
#44457=CARTESIAN_POINT('Ctrl Pts',(8.60474859865648,16.4472645215626,85.4668665636608));
#44458=CARTESIAN_POINT('Ctrl Pts',(8.55014120211907,16.3772240255913,85.4613625335412));
#44459=CARTESIAN_POINT('Ctrl Pts',(8.53434287032992,16.3557032208687,85.4597347029858));
#44460=CARTESIAN_POINT('Ctrl Pts',(8.51904255235788,16.333616011952,85.4581256707728));
#44461=CARTESIAN_POINT('Ctrl Pts',(8.48962600103117,16.2884083933886,85.4549757803719));
#44462=CARTESIAN_POINT('Ctrl Pts',(8.39668257439119,16.1218710106354,85.4444904181629));
#44463=CARTESIAN_POINT('Ctrl Pts',(8.35603499314338,15.9372797480275,85.4390826561945));
#44464=CARTESIAN_POINT('Ctrl Pts',(8.35603499314338,15.8,85.4390826561945));
#44465=CARTESIAN_POINT('Origin',(9.31,15.8,83.24125));
#44466=CARTESIAN_POINT('',(9.30971443151743,14.9950000506518,81.1524999870659));
#44467=CARTESIAN_POINT('',(8.50493382511065,15.8000495525908,81.0427739960352));
#44468=CARTESIAN_POINT('Ctrl Pts',(9.30971443151743,14.9950000506518,81.1524999870659));
#44469=CARTESIAN_POINT('Ctrl Pts',(9.47284767131029,14.9949421801988,81.1525147644529));
#44470=CARTESIAN_POINT('Ctrl Pts',(9.79584033527272,15.0993874455422,81.1239737564541));
#44471=CARTESIAN_POINT('Ctrl Pts',(10.0425595102383,15.4113740238506,81.0633302501805));
#44472=CARTESIAN_POINT('Ctrl Pts',(10.1189117455193,15.6998872287926,81.0414272750389));
#44473=CARTESIAN_POINT('Ctrl Pts',(10.1152364214667,15.99695011648,81.0423153895362));
#44474=CARTESIAN_POINT('Ctrl Pts',(10.0204956825243,16.2088719014764,81.0701904801504));
#44475=CARTESIAN_POINT('Ctrl Pts',(9.9044103854419,16.3436108471324,81.0944871436364));
#44476=CARTESIAN_POINT('Ctrl Pts',(9.88786634588363,16.361141904578,81.0977809418426));
#44477=CARTESIAN_POINT('Ctrl Pts',(9.80100095605804,16.4455527332759,81.1142474637718));
#44478=CARTESIAN_POINT('Ctrl Pts',(9.62439492967267,16.5644831932575,81.1417563388649));
#44479=CARTESIAN_POINT('Ctrl Pts',(9.38524990047136,16.6101492764359,81.1538705707198));
#44480=CARTESIAN_POINT('Ctrl Pts',(9.23365810330067,16.6027009170661,81.1519184980892));
#44481=CARTESIAN_POINT('Ctrl Pts',(9.12951062622373,16.5878157822367,81.1481620130899));
#44482=CARTESIAN_POINT('Ctrl Pts',(8.9511729466788,16.5345389475329,81.1348278227182));
#44483=CARTESIAN_POINT('Ctrl Pts',(8.8191656566872,16.4455872622242,81.1143735731117));
#44484=CARTESIAN_POINT('Ctrl Pts',(8.63368064477052,16.265506383372,81.0793273667541));
#44485=CARTESIAN_POINT('Ctrl Pts',(8.52785160642035,16.0691577161987,81.0488154213655));
#44486=CARTESIAN_POINT('Ctrl Pts',(8.50496051869156,15.8580350113622,81.0427179128319));
#44487=CARTESIAN_POINT('Ctrl Pts',(8.50493382511065,15.8000495525908,81.0427739960352));
#44488=CARTESIAN_POINT('Ctrl Pts',(8.50493382511065,15.8000495525908,81.0427739960352));
#44489=CARTESIAN_POINT('Ctrl Pts',(8.50489001938542,15.7048920282917,81.042866031847));
#44490=CARTESIAN_POINT('Ctrl Pts',(8.5487676875157,15.456580448563,81.0552684209999));
#44491=CARTESIAN_POINT('Ctrl Pts',(8.75653315952666,15.1754693805007,81.1086537222845));
#44492=CARTESIAN_POINT('Ctrl Pts',(9.05576289094108,15.0222450031167,81.1453157035286));
#44493=CARTESIAN_POINT('Ctrl Pts',(9.22496960714143,14.9950301133256,81.1524923104755));
#44494=CARTESIAN_POINT('Ctrl Pts',(9.30971443151743,14.9950000506518,81.1524999870659));
#44495=CARTESIAN_POINT('',(8.505,15.8,83.24125));
#44496=CARTESIAN_POINT('Origin',(9.31,18.775,78.));
#44497=CARTESIAN_POINT('',(1.81,14.25,78.));
#44498=CARTESIAN_POINT('Origin',(9.31,14.25,78.));
#44499=CARTESIAN_POINT('',(1.81,17.5,78.));
#44500=CARTESIAN_POINT('',(1.81,18.775,78.));
#44501=CARTESIAN_POINT('',(1.81,20.5,78.));
#44502=CARTESIAN_POINT('Ctrl Pts',(1.81,17.5,78.));
#44503=CARTESIAN_POINT('Ctrl Pts',(1.81,17.5,77.905556478434));
#44504=CARTESIAN_POINT('Ctrl Pts',(1.81183067420966,17.5090634188645,77.8079678203077));
#44505=CARTESIAN_POINT('Ctrl Pts',(1.81931072941389,17.5471495606178,77.6140027878517));
#44506=CARTESIAN_POINT('Ctrl Pts',(1.82495532590085,17.5761632619054,77.5176244577088));
#44507=CARTESIAN_POINT('Ctrl Pts',(1.84624979272205,17.6910934876829,77.2405577082036));
#44508=CARTESIAN_POINT('Ctrl Pts',(1.86639493542522,17.806452793408,77.0722268630324));
#44509=CARTESIAN_POINT('Ctrl Pts',(1.90436372347101,18.0722343097285,76.8064453467119));
#44510=CARTESIAN_POINT('Ctrl Pts',(1.92468773810844,18.2405619924549,76.6910918735274));
#44511=CARTESIAN_POINT('Ctrl Pts',(1.94629082256958,18.5176204988066,76.5761648226022));
#44512=CARTESIAN_POINT('Ctrl Pts',(1.95203778940752,18.6139962349031,76.547151319492));
#44513=CARTESIAN_POINT('Ctrl Pts',(1.9596606794129,18.8079605728532,76.5090643698119));
#44514=CARTESIAN_POINT('Ctrl Pts',(1.96153077165046,18.9055511860275,76.5));
#44515=CARTESIAN_POINT('Ctrl Pts',(1.96153077165046,19.0944488139725,76.5));
#44516=CARTESIAN_POINT('Ctrl Pts',(1.9596606794129,19.1920394271468,76.5090643698119));
#44517=CARTESIAN_POINT('Ctrl Pts',(1.95203778940752,19.3860037650969,76.547151319492));
#44518=CARTESIAN_POINT('Ctrl Pts',(1.94629082256958,19.4823795011934,76.5761648226022));
#44519=CARTESIAN_POINT('Ctrl Pts',(1.92468773810844,19.7594380075451,76.6910918735274));
#44520=CARTESIAN_POINT('Ctrl Pts',(1.90436372347101,19.9277656902715,76.8064453467119));
#44521=CARTESIAN_POINT('Ctrl Pts',(1.86639493542522,20.193547206592,77.0722268630324));
#44522=CARTESIAN_POINT('Ctrl Pts',(1.84624979272205,20.3089065123171,77.2405577082036));
#44523=CARTESIAN_POINT('Ctrl Pts',(1.82495532590085,20.4238367380946,77.5176244577088));
#44524=CARTESIAN_POINT('Ctrl Pts',(1.81931072941389,20.4528504393822,77.6140027878517));
#44525=CARTESIAN_POINT('Ctrl Pts',(1.81183067420965,20.4909365811355,77.8079678203077));
#44526=CARTESIAN_POINT('Ctrl Pts',(1.81,20.5,77.905556478434));
#44527=CARTESIAN_POINT('Ctrl Pts',(1.81,20.5,78.));
#44528=CARTESIAN_POINT('',(1.81,23.3,78.));
#44529=CARTESIAN_POINT('',(1.81,18.775,78.));
#44530=CARTESIAN_POINT('Origin',(9.31,23.3,78.));
#44531=CARTESIAN_POINT('',(1.96153077165046,19.,79.5));
#44532=CARTESIAN_POINT('Ctrl Pts',(1.81,20.5,78.));
#44533=CARTESIAN_POINT('Ctrl Pts',(1.81,20.5,78.094443521566));
#44534=CARTESIAN_POINT('Ctrl Pts',(1.81183067420966,20.4909365811355,78.1920321796923));
#44535=CARTESIAN_POINT('Ctrl Pts',(1.81931072941389,20.4528504393822,78.3859972121483));
#44536=CARTESIAN_POINT('Ctrl Pts',(1.82495532590085,20.4238367380946,78.4823755422912));
#44537=CARTESIAN_POINT('Ctrl Pts',(1.84624979272205,20.3089065123171,78.7594422917964));
#44538=CARTESIAN_POINT('Ctrl Pts',(1.86639493542522,20.193547206592,78.9277731369676));
#44539=CARTESIAN_POINT('Ctrl Pts',(1.90436372347101,19.9277656902715,79.1935546532881));
#44540=CARTESIAN_POINT('Ctrl Pts',(1.92468773810844,19.7594380075451,79.3089081264726));
#44541=CARTESIAN_POINT('Ctrl Pts',(1.94629082256958,19.4823795011934,79.4238351773978));
#44542=CARTESIAN_POINT('Ctrl Pts',(1.95203778940752,19.3860037650969,79.452848680508));
#44543=CARTESIAN_POINT('Ctrl Pts',(1.9596606794129,19.1920394271468,79.4909356301881));
#44544=CARTESIAN_POINT('Ctrl Pts',(1.96153077165046,19.0944488139725,79.5));
#44545=CARTESIAN_POINT('Ctrl Pts',(1.96153077165046,19.,79.5));
#44546=CARTESIAN_POINT('Ctrl Pts',(1.96153077165046,19.,79.5));
#44547=CARTESIAN_POINT('Ctrl Pts',(1.96153077165046,18.9055511860275,79.5));
#44548=CARTESIAN_POINT('Ctrl Pts',(1.9596606794129,18.8079605728532,79.4909356301881));
#44549=CARTESIAN_POINT('Ctrl Pts',(1.95203778940752,18.6139962349031,79.452848680508));
#44550=CARTESIAN_POINT('Ctrl Pts',(1.94629082256958,18.5176204988066,79.4238351773978));
#44551=CARTESIAN_POINT('Ctrl Pts',(1.92468773810844,18.2405619924549,79.3089081264726));
#44552=CARTESIAN_POINT('Ctrl Pts',(1.90436372347101,18.0722343097285,79.1935546532881));
#44553=CARTESIAN_POINT('Ctrl Pts',(1.86639493542522,17.806452793408,78.9277731369676));
#44554=CARTESIAN_POINT('Ctrl Pts',(1.84624979272205,17.6910934876829,78.7594422917964));
#44555=CARTESIAN_POINT('Ctrl Pts',(1.82495532590085,17.5761632619054,78.4823755422912));
#44556=CARTESIAN_POINT('Ctrl Pts',(1.81931072941389,17.5471495606178,78.3859972121483));
#44557=CARTESIAN_POINT('Ctrl Pts',(1.81183067420966,17.5090634188645,78.1920321796923));
#44558=CARTESIAN_POINT('Ctrl Pts',(1.81,17.5,78.0944435215661));
#44559=CARTESIAN_POINT('Ctrl Pts',(1.81,17.5,78.));
#44560=CARTESIAN_POINT('',(16.6584692283495,19.,76.5));
#44561=CARTESIAN_POINT('Ctrl Pts',(16.6584692283495,19.,76.5));
#44562=CARTESIAN_POINT('Ctrl Pts',(16.6584692283495,18.9055511860275,76.5));
#44563=CARTESIAN_POINT('Ctrl Pts',(16.6603393205871,18.8079605728532,76.5090643698119));
#44564=CARTESIAN_POINT('Ctrl Pts',(16.6679622105925,18.6139962349031,76.547151319492));
#44565=CARTESIAN_POINT('Ctrl Pts',(16.6737091774304,18.5176204988066,76.5761648226022));
#44566=CARTESIAN_POINT('Ctrl Pts',(16.6953122618916,18.2405619924549,76.6910918735274));
#44567=CARTESIAN_POINT('Ctrl Pts',(16.715636276529,18.0722343097285,76.8064453467119));
#44568=CARTESIAN_POINT('Ctrl Pts',(16.7536050645748,17.806452793408,77.0722268630324));
#44569=CARTESIAN_POINT('Ctrl Pts',(16.773750207278,17.6910934876829,77.2405577082036));
#44570=CARTESIAN_POINT('Ctrl Pts',(16.7950446740992,17.5761632619054,77.5176244577088));
#44571=CARTESIAN_POINT('Ctrl Pts',(16.8006892705861,17.5471495606178,77.6140027878517));
#44572=CARTESIAN_POINT('Ctrl Pts',(16.8081693257903,17.5090634188645,77.8079678203077));
#44573=CARTESIAN_POINT('Ctrl Pts',(16.81,17.5,77.905556478434));
#44574=CARTESIAN_POINT('Ctrl Pts',(16.81,17.5,78.094443521566));
#44575=CARTESIAN_POINT('Ctrl Pts',(16.8081693257903,17.5090634188645,78.1920321796923));
#44576=CARTESIAN_POINT('Ctrl Pts',(16.8006892705861,17.5471495606178,78.3859972121484));
#44577=CARTESIAN_POINT('Ctrl Pts',(16.7950446740992,17.5761632619054,78.4823755422912));
#44578=CARTESIAN_POINT('Ctrl Pts',(16.773750207278,17.6910934876829,78.7594422917964));
#44579=CARTESIAN_POINT('Ctrl Pts',(16.7536050645748,17.806452793408,78.9277731369676));
#44580=CARTESIAN_POINT('Ctrl Pts',(16.715636276529,18.0722343097285,79.1935546532881));
#44581=CARTESIAN_POINT('Ctrl Pts',(16.6953122618916,18.2405619924549,79.3089081264726));
#44582=CARTESIAN_POINT('Ctrl Pts',(16.6737091774304,18.5176204988066,79.4238351773978));
#44583=CARTESIAN_POINT('Ctrl Pts',(16.6679622105925,18.6139962349031,79.452848680508));
#44584=CARTESIAN_POINT('Ctrl Pts',(16.6603393205871,18.8079605728532,79.4909356301881));
#44585=CARTESIAN_POINT('Ctrl Pts',(16.6584692283495,18.9055511860275,79.5));
#44586=CARTESIAN_POINT('Ctrl Pts',(16.6584692283495,19.0944488139725,79.5));
#44587=CARTESIAN_POINT('Ctrl Pts',(16.6603393205871,19.1920394271468,79.4909356301881));
#44588=CARTESIAN_POINT('Ctrl Pts',(16.6679622105925,19.3860037650969,79.452848680508));
#44589=CARTESIAN_POINT('Ctrl Pts',(16.6737091774304,19.4823795011934,79.4238351773978));
#44590=CARTESIAN_POINT('Ctrl Pts',(16.6953122618916,19.7594380075451,79.3089081264726));
#44591=CARTESIAN_POINT('Ctrl Pts',(16.715636276529,19.9277656902715,79.1935546532881));
#44592=CARTESIAN_POINT('Ctrl Pts',(16.7536050645748,20.193547206592,78.9277731369676));
#44593=CARTESIAN_POINT('Ctrl Pts',(16.7737502072779,20.3089065123171,78.7594422917965));
#44594=CARTESIAN_POINT('Ctrl Pts',(16.7950446740991,20.4238367380946,78.4823755422912));
#44595=CARTESIAN_POINT('Ctrl Pts',(16.8006892705861,20.4528504393822,78.3859972121483));
#44596=CARTESIAN_POINT('Ctrl Pts',(16.8081693257903,20.4909365811355,78.1920321796923));
#44597=CARTESIAN_POINT('Ctrl Pts',(16.81,20.5,78.094443521566));
#44598=CARTESIAN_POINT('Ctrl Pts',(16.81,20.5,77.905556478434));
#44599=CARTESIAN_POINT('Ctrl Pts',(16.8081693257903,20.4909365811355,77.8079678203077));
#44600=CARTESIAN_POINT('Ctrl Pts',(16.8006892705861,20.4528504393822,77.6140027878517));
#44601=CARTESIAN_POINT('Ctrl Pts',(16.7950446740992,20.4238367380946,77.5176244577088));
#44602=CARTESIAN_POINT('Ctrl Pts',(16.773750207278,20.3089065123172,77.2405577082036));
#44603=CARTESIAN_POINT('Ctrl Pts',(16.7536050645748,20.193547206592,77.0722268630324));
#44604=CARTESIAN_POINT('Ctrl Pts',(16.715636276529,19.9277656902715,76.8064453467119));
#44605=CARTESIAN_POINT('Ctrl Pts',(16.6953122618916,19.7594380075451,76.6910918735274));
#44606=CARTESIAN_POINT('Ctrl Pts',(16.6737091774304,19.4823795011934,76.5761648226022));
#44607=CARTESIAN_POINT('Ctrl Pts',(16.6679622105925,19.3860037650969,76.547151319492));
#44608=CARTESIAN_POINT('Ctrl Pts',(16.6603393205871,19.1920394271468,76.5090643698119));
#44609=CARTESIAN_POINT('Ctrl Pts',(16.6584692283495,19.0944488139725,76.5));
#44610=CARTESIAN_POINT('Ctrl Pts',(16.6584692283495,19.,76.5));
#44611=CARTESIAN_POINT('',(14.2832727198514,19.,83.6139610306789));
#44612=CARTESIAN_POINT('Ctrl Pts',(14.2832727198514,19.,83.6139610306789));
#44613=CARTESIAN_POINT('Ctrl Pts',(14.2832727198514,18.9055511860275,83.6139610306789));
#44614=CARTESIAN_POINT('Ctrl Pts',(14.2763577914438,18.8079605728532,83.62011276297));
#44615=CARTESIAN_POINT('Ctrl Pts',(14.2471849704709,18.6139962349031,83.645757854205));
#44616=CARTESIAN_POINT('Ctrl Pts',(14.2249320231437,18.5176204988066,83.6652416250364));
#44617=CARTESIAN_POINT('Ctrl Pts',(14.1362038196909,18.2405619924549,83.7414139704425));
#44618=CARTESIAN_POINT('Ctrl Pts',(14.0464667888171,18.0722343097285,83.8166918200176));
#44619=CARTESIAN_POINT('Ctrl Pts',(13.8352776378501,17.806452793408,83.9824645131764));
#44620=CARTESIAN_POINT('Ctrl Pts',(13.699571421043,17.6910934876829,84.0840761411059));
#44621=CARTESIAN_POINT('Ctrl Pts',(13.4702718108381,17.5761632619054,84.2410510650857));
#44622=CARTESIAN_POINT('Ctrl Pts',(13.3896280268035,17.5471495606178,84.2941285941089));
#44623=CARTESIAN_POINT('Ctrl Pts',(13.2253894088528,17.5090634188645,84.3975890281656));
#44624=CARTESIAN_POINT('Ctrl Pts',(13.1417904888991,17.5,84.4479687676003));
#44625=CARTESIAN_POINT('Ctrl Pts',(12.9782095111009,17.5,84.5424122891663));
#44626=CARTESIAN_POINT('Ctrl Pts',(12.8927799169376,17.5090634188645,84.5896212078578));
#44627=CARTESIAN_POINT('Ctrl Pts',(12.7210612437826,17.5471495606178,84.6801258062573));
#44628=CARTESIAN_POINT('Ctrl Pts',(12.6347728632611,17.5761632619054,84.7234266073769));
#44629=CARTESIAN_POINT('Ctrl Pts',(12.384178786235,17.6910934876829,84.8435184329023));
#44630=CARTESIAN_POINT('Ctrl Pts',(12.2283274267246,17.806452793408,84.9102376501441));
#44631=CARTESIAN_POINT('Ctrl Pts',(11.9791694877118,18.0722343097285,85.0102464733058));
#44632=CARTESIAN_POINT('Ctrl Pts',(11.8691084422006,18.2405619924549,85.0503220969151));
#44633=CARTESIAN_POINT('Ctrl Pts',(11.7587771542868,18.5176204988066,85.0890768024343));
#44634=CARTESIAN_POINT('Ctrl Pts',(11.7307772401216,18.6139962349031,85.098606534713));
#44635=CARTESIAN_POINT('Ctrl Pts',(11.6939815291433,18.8079605728532,85.1110483931581));
#44636=CARTESIAN_POINT('Ctrl Pts',(11.6851965084981,18.9055511860275,85.1139610306789));
#44637=CARTESIAN_POINT('Ctrl Pts',(11.6851965084981,19.0944488139725,85.1139610306789));
#44638=CARTESIAN_POINT('Ctrl Pts',(11.6939815291433,19.1920394271468,85.1110483931581));
#44639=CARTESIAN_POINT('Ctrl Pts',(11.7307772401216,19.3860037650969,85.098606534713));
#44640=CARTESIAN_POINT('Ctrl Pts',(11.7587771542868,19.4823795011934,85.0890768024343));
#44641=CARTESIAN_POINT('Ctrl Pts',(11.8691084422006,19.7594380075451,85.0503220969151));
#44642=CARTESIAN_POINT('Ctrl Pts',(11.9791694877118,19.9277656902715,85.0102464733058));
#44643=CARTESIAN_POINT('Ctrl Pts',(12.2283274267246,20.193547206592,84.9102376501441));
#44644=CARTESIAN_POINT('Ctrl Pts',(12.384178786235,20.3089065123171,84.8435184329023));
#44645=CARTESIAN_POINT('Ctrl Pts',(12.6347728632611,20.4238367380946,84.7234266073769));
#44646=CARTESIAN_POINT('Ctrl Pts',(12.7210612437826,20.4528504393822,84.6801258062573));
#44647=CARTESIAN_POINT('Ctrl Pts',(12.8927799169376,20.4909365811355,84.5896212078578));
#44648=CARTESIAN_POINT('Ctrl Pts',(12.9782095111009,20.5,84.5424122891663));
#44649=CARTESIAN_POINT('Ctrl Pts',(13.1417904888991,20.5,84.4479687676003));
#44650=CARTESIAN_POINT('Ctrl Pts',(13.2253894088528,20.4909365811355,84.3975890281656));
#44651=CARTESIAN_POINT('Ctrl Pts',(13.3896280268035,20.4528504393822,84.2941285941089));
#44652=CARTESIAN_POINT('Ctrl Pts',(13.4702718108381,20.4238367380946,84.2410510650857));
#44653=CARTESIAN_POINT('Ctrl Pts',(13.699571421043,20.3089065123171,84.0840761411059));
#44654=CARTESIAN_POINT('Ctrl Pts',(13.8352776378501,20.193547206592,83.9824645131764));
#44655=CARTESIAN_POINT('Ctrl Pts',(14.0464667888171,19.9277656902715,83.8166918200176));
#44656=CARTESIAN_POINT('Ctrl Pts',(14.1362038196909,19.7594380075451,83.7414139704425));
#44657=CARTESIAN_POINT('Ctrl Pts',(14.2249320231437,19.4823795011934,83.6652416250364));
#44658=CARTESIAN_POINT('Ctrl Pts',(14.2471849704709,19.3860037650969,83.645757854205));
#44659=CARTESIAN_POINT('Ctrl Pts',(14.2763577914438,19.1920394271468,83.62011276297));
#44660=CARTESIAN_POINT('Ctrl Pts',(14.2832727198514,19.0944488139725,83.6139610306789));
#44661=CARTESIAN_POINT('Ctrl Pts',(14.2832727198514,19.,83.6139610306789));
#44662=CARTESIAN_POINT('',(6.93480349150189,19.,85.1139610306789));
#44663=CARTESIAN_POINT('Ctrl Pts',(6.93480349150189,19.,85.1139610306789));
#44664=CARTESIAN_POINT('Ctrl Pts',(6.93480349150189,18.9055511860275,85.1139610306789));
#44665=CARTESIAN_POINT('Ctrl Pts',(6.92601847085671,18.8079605728532,85.1110483931581));
#44666=CARTESIAN_POINT('Ctrl Pts',(6.88922275987842,18.6139962349031,85.098606534713));
#44667=CARTESIAN_POINT('Ctrl Pts',(6.86122284571324,18.5176204988066,85.0890768024343));
#44668=CARTESIAN_POINT('Ctrl Pts',(6.75089155779936,18.2405619924549,85.0503220969151));
#44669=CARTESIAN_POINT('Ctrl Pts',(6.64083051228816,18.0722343097285,85.0102464733058));
#44670=CARTESIAN_POINT('Ctrl Pts',(6.39167257327537,17.806452793408,84.9102376501441));
#44671=CARTESIAN_POINT('Ctrl Pts',(6.23582121376502,17.6910934876829,84.8435184329023));
#44672=CARTESIAN_POINT('Ctrl Pts',(5.98522713673891,17.5761632619054,84.7234266073769));
#44673=CARTESIAN_POINT('Ctrl Pts',(5.89893875621735,17.5471495606178,84.6801258062573));
#44674=CARTESIAN_POINT('Ctrl Pts',(5.72722008306242,17.5090634188645,84.5896212078578));
#44675=CARTESIAN_POINT('Ctrl Pts',(5.64179048889907,17.5,84.5424122891663));
#44676=CARTESIAN_POINT('Ctrl Pts',(5.47820951110094,17.5,84.4479687676003));
#44677=CARTESIAN_POINT('Ctrl Pts',(5.39461059114724,17.5090634188645,84.3975890281656));
#44678=CARTESIAN_POINT('Ctrl Pts',(5.23037197319652,17.5471495606178,84.2941285941089));
#44679=CARTESIAN_POINT('Ctrl Pts',(5.14972818916194,17.5761632619054,84.2410510650857));
#44680=CARTESIAN_POINT('Ctrl Pts',(4.92042857895703,17.6910934876829,84.0840761411059));
#44681=CARTESIAN_POINT('Ctrl Pts',(4.78472236214986,17.806452793408,83.9824645131764));
#44682=CARTESIAN_POINT('Ctrl Pts',(4.57353321118285,18.0722343097285,83.8166918200176));
#44683=CARTESIAN_POINT('Ctrl Pts',(4.48379618030908,18.2405619924549,83.7414139704425));
#44684=CARTESIAN_POINT('Ctrl Pts',(4.39506797685635,18.5176204988066,83.6652416250364));
#44685=CARTESIAN_POINT('Ctrl Pts',(4.3728150295291,18.6139962349031,83.645757854205));
#44686=CARTESIAN_POINT('Ctrl Pts',(4.34364220855619,18.8079605728532,83.62011276297));
#44687=CARTESIAN_POINT('Ctrl Pts',(4.33672728014858,18.9055511860275,83.6139610306789));
#44688=CARTESIAN_POINT('Ctrl Pts',(4.33672728014858,19.0944488139725,83.6139610306789));
#44689=CARTESIAN_POINT('Ctrl Pts',(4.34364220855619,19.1920394271468,83.62011276297));
#44690=CARTESIAN_POINT('Ctrl Pts',(4.3728150295291,19.3860037650969,83.645757854205));
#44691=CARTESIAN_POINT('Ctrl Pts',(4.39506797685635,19.4823795011934,83.6652416250364));
#44692=CARTESIAN_POINT('Ctrl Pts',(4.48379618030908,19.7594380075451,83.7414139704425));
#44693=CARTESIAN_POINT('Ctrl Pts',(4.57353321118285,19.9277656902715,83.8166918200176));
#44694=CARTESIAN_POINT('Ctrl Pts',(4.78472236214986,20.193547206592,83.9824645131764));
#44695=CARTESIAN_POINT('Ctrl Pts',(4.92042857895703,20.3089065123171,84.0840761411059));
#44696=CARTESIAN_POINT('Ctrl Pts',(5.14972818916194,20.4238367380946,84.2410510650857));
#44697=CARTESIAN_POINT('Ctrl Pts',(5.23037197319652,20.4528504393822,84.2941285941089));
#44698=CARTESIAN_POINT('Ctrl Pts',(5.39461059114724,20.4909365811355,84.3975890281656));
#44699=CARTESIAN_POINT('Ctrl Pts',(5.47820951110094,20.5,84.4479687676003));
#44700=CARTESIAN_POINT('Ctrl Pts',(5.64179048889906,20.5,84.5424122891663));
#44701=CARTESIAN_POINT('Ctrl Pts',(5.72722008306241,20.4909365811355,84.5896212078578));
#44702=CARTESIAN_POINT('Ctrl Pts',(5.89893875621735,20.4528504393822,84.6801258062573));
#44703=CARTESIAN_POINT('Ctrl Pts',(5.98522713673891,20.4238367380946,84.7234266073769));
#44704=CARTESIAN_POINT('Ctrl Pts',(6.23582121376502,20.3089065123171,84.8435184329023));
#44705=CARTESIAN_POINT('Ctrl Pts',(6.39167257327537,20.193547206592,84.9102376501441));
#44706=CARTESIAN_POINT('Ctrl Pts',(6.64083051228816,19.9277656902715,85.0102464733058));
#44707=CARTESIAN_POINT('Ctrl Pts',(6.75089155779936,19.7594380075451,85.0503220969151));
#44708=CARTESIAN_POINT('Ctrl Pts',(6.86122284571324,19.4823795011934,85.0890768024343));
#44709=CARTESIAN_POINT('Ctrl Pts',(6.88922275987842,19.3860037650969,85.098606534713));
#44710=CARTESIAN_POINT('Ctrl Pts',(6.92601847085671,19.1920394271468,85.1110483931581));
#44711=CARTESIAN_POINT('Ctrl Pts',(6.93480349150189,19.0944488139725,85.1139610306789));
#44712=CARTESIAN_POINT('Ctrl Pts',(6.93480349150189,19.,85.1139610306789));
#44713=CARTESIAN_POINT('',(4.33672728014858,19.,72.3860389693211));
#44714=CARTESIAN_POINT('Ctrl Pts',(4.33672728014858,19.,72.3860389693211));
#44715=CARTESIAN_POINT('Ctrl Pts',(4.33672728014858,18.9055511860275,72.3860389693211));
#44716=CARTESIAN_POINT('Ctrl Pts',(4.34364220855619,18.8079605728532,72.37988723703));
#44717=CARTESIAN_POINT('Ctrl Pts',(4.3728150295291,18.6139962349031,72.354242145795));
#44718=CARTESIAN_POINT('Ctrl Pts',(4.39506797685635,18.5176204988066,72.3347583749636));
#44719=CARTESIAN_POINT('Ctrl Pts',(4.48379618030908,18.2405619924549,72.2585860295575));
#44720=CARTESIAN_POINT('Ctrl Pts',(4.57353321118286,18.0722343097285,72.1833081799824));
#44721=CARTESIAN_POINT('Ctrl Pts',(4.78472236214986,17.806452793408,72.0175354868236));
#44722=CARTESIAN_POINT('Ctrl Pts',(4.92042857895703,17.6910934876829,71.9159238588941));
#44723=CARTESIAN_POINT('Ctrl Pts',(5.14972818916194,17.5761632619054,71.7589489349143));
#44724=CARTESIAN_POINT('Ctrl Pts',(5.23037197319652,17.5471495606178,71.7058714058911));
#44725=CARTESIAN_POINT('Ctrl Pts',(5.39461059114724,17.5090634188645,71.6024109718344));
#44726=CARTESIAN_POINT('Ctrl Pts',(5.47820951110094,17.5,71.5520312323997));
#44727=CARTESIAN_POINT('Ctrl Pts',(5.64179048889907,17.5,71.4575877108337));
#44728=CARTESIAN_POINT('Ctrl Pts',(5.72722008306241,17.5090634188645,71.4103787921422));
#44729=CARTESIAN_POINT('Ctrl Pts',(5.89893875621735,17.5471495606178,71.3198741937427));
#44730=CARTESIAN_POINT('Ctrl Pts',(5.98522713673891,17.5761632619054,71.2765733926231));
#44731=CARTESIAN_POINT('Ctrl Pts',(6.23582121376502,17.6910934876829,71.1564815670977));
#44732=CARTESIAN_POINT('Ctrl Pts',(6.39167257327537,17.806452793408,71.0897623498559));
#44733=CARTESIAN_POINT('Ctrl Pts',(6.64083051228816,18.0722343097285,70.9897535266942));
#44734=CARTESIAN_POINT('Ctrl Pts',(6.75089155779937,18.2405619924549,70.9496779030849));
#44735=CARTESIAN_POINT('Ctrl Pts',(6.86122284571324,18.5176204988066,70.9109231975657));
#44736=CARTESIAN_POINT('Ctrl Pts',(6.88922275987843,18.6139962349031,70.901393465287));
#44737=CARTESIAN_POINT('Ctrl Pts',(6.92601847085672,18.8079605728532,70.8889516068419));
#44738=CARTESIAN_POINT('Ctrl Pts',(6.93480349150189,18.9055511860275,70.8860389693211));
#44739=CARTESIAN_POINT('Ctrl Pts',(6.93480349150189,19.0944488139725,70.8860389693211));
#44740=CARTESIAN_POINT('Ctrl Pts',(6.92601847085672,19.1920394271468,70.8889516068419));
#44741=CARTESIAN_POINT('Ctrl Pts',(6.88922275987843,19.3860037650969,70.901393465287));
#44742=CARTESIAN_POINT('Ctrl Pts',(6.86122284571324,19.4823795011934,70.9109231975657));
#44743=CARTESIAN_POINT('Ctrl Pts',(6.75089155779936,19.7594380075451,70.9496779030849));
#44744=CARTESIAN_POINT('Ctrl Pts',(6.64083051228816,19.9277656902715,70.9897535266942));
#44745=CARTESIAN_POINT('Ctrl Pts',(6.39167257327537,20.193547206592,71.0897623498559));
#44746=CARTESIAN_POINT('Ctrl Pts',(6.23582121376502,20.3089065123171,71.1564815670977));
#44747=CARTESIAN_POINT('Ctrl Pts',(5.9852271367389,20.4238367380946,71.2765733926231));
#44748=CARTESIAN_POINT('Ctrl Pts',(5.89893875621735,20.4528504393822,71.3198741937427));
#44749=CARTESIAN_POINT('Ctrl Pts',(5.72722008306241,20.4909365811355,71.4103787921422));
#44750=CARTESIAN_POINT('Ctrl Pts',(5.64179048889907,20.5,71.4575877108337));
#44751=CARTESIAN_POINT('Ctrl Pts',(5.47820951110094,20.5,71.5520312323997));
#44752=CARTESIAN_POINT('Ctrl Pts',(5.39461059114724,20.4909365811355,71.6024109718344));
#44753=CARTESIAN_POINT('Ctrl Pts',(5.23037197319652,20.4528504393822,71.7058714058911));
#44754=CARTESIAN_POINT('Ctrl Pts',(5.14972818916194,20.4238367380946,71.7589489349143));
#44755=CARTESIAN_POINT('Ctrl Pts',(4.92042857895703,20.3089065123171,71.9159238588941));
#44756=CARTESIAN_POINT('Ctrl Pts',(4.78472236214986,20.193547206592,72.0175354868236));
#44757=CARTESIAN_POINT('Ctrl Pts',(4.57353321118286,19.9277656902715,72.1833081799824));
#44758=CARTESIAN_POINT('Ctrl Pts',(4.48379618030908,19.7594380075451,72.2585860295575));
#44759=CARTESIAN_POINT('Ctrl Pts',(4.39506797685635,19.4823795011934,72.3347583749636));
#44760=CARTESIAN_POINT('Ctrl Pts',(4.3728150295291,19.3860037650969,72.354242145795));
#44761=CARTESIAN_POINT('Ctrl Pts',(4.34364220855619,19.1920394271468,72.37988723703));
#44762=CARTESIAN_POINT('Ctrl Pts',(4.33672728014858,19.0944488139725,72.3860389693211));
#44763=CARTESIAN_POINT('Ctrl Pts',(4.33672728014858,19.,72.3860389693211));
#44764=CARTESIAN_POINT('',(11.6851965084981,19.,70.8860389693211));
#44765=CARTESIAN_POINT('Ctrl Pts',(11.6851965084981,19.,70.8860389693211));
#44766=CARTESIAN_POINT('Ctrl Pts',(11.6851965084981,18.9055511860275,70.8860389693211));
#44767=CARTESIAN_POINT('Ctrl Pts',(11.6939815291433,18.8079605728532,70.8889516068419));
#44768=CARTESIAN_POINT('Ctrl Pts',(11.7307772401216,18.6139962349031,70.901393465287));
#44769=CARTESIAN_POINT('Ctrl Pts',(11.7587771542868,18.5176204988066,70.9109231975657));
#44770=CARTESIAN_POINT('Ctrl Pts',(11.8691084422006,18.2405619924549,70.9496779030849));
#44771=CARTESIAN_POINT('Ctrl Pts',(11.9791694877118,18.0722343097285,70.9897535266942));
#44772=CARTESIAN_POINT('Ctrl Pts',(12.2283274267246,17.806452793408,71.0897623498559));
#44773=CARTESIAN_POINT('Ctrl Pts',(12.384178786235,17.6910934876829,71.1564815670977));
#44774=CARTESIAN_POINT('Ctrl Pts',(12.6347728632611,17.5761632619054,71.2765733926231));
#44775=CARTESIAN_POINT('Ctrl Pts',(12.7210612437826,17.5471495606178,71.3198741937427));
#44776=CARTESIAN_POINT('Ctrl Pts',(12.8927799169376,17.5090634188645,71.4103787921422));
#44777=CARTESIAN_POINT('Ctrl Pts',(12.9782095111009,17.5,71.4575877108337));
#44778=CARTESIAN_POINT('Ctrl Pts',(13.1417904888991,17.5,71.5520312323997));
#44779=CARTESIAN_POINT('Ctrl Pts',(13.2253894088528,17.5090634188645,71.6024109718344));
#44780=CARTESIAN_POINT('Ctrl Pts',(13.3896280268035,17.5471495606178,71.7058714058911));
#44781=CARTESIAN_POINT('Ctrl Pts',(13.4702718108381,17.5761632619054,71.7589489349143));
#44782=CARTESIAN_POINT('Ctrl Pts',(13.699571421043,17.6910934876829,71.9159238588941));
#44783=CARTESIAN_POINT('Ctrl Pts',(13.8352776378501,17.806452793408,72.0175354868236));
#44784=CARTESIAN_POINT('Ctrl Pts',(14.0464667888171,18.0722343097285,72.1833081799824));
#44785=CARTESIAN_POINT('Ctrl Pts',(14.1362038196909,18.2405619924549,72.2585860295575));
#44786=CARTESIAN_POINT('Ctrl Pts',(14.2249320231436,18.5176204988066,72.3347583749636));
#44787=CARTESIAN_POINT('Ctrl Pts',(14.2471849704709,18.6139962349031,72.354242145795));
#44788=CARTESIAN_POINT('Ctrl Pts',(14.2763577914438,18.8079605728532,72.37988723703));
#44789=CARTESIAN_POINT('Ctrl Pts',(14.2832727198514,18.9055511860275,72.3860389693211));
#44790=CARTESIAN_POINT('Ctrl Pts',(14.2832727198514,19.0944488139725,72.3860389693211));
#44791=CARTESIAN_POINT('Ctrl Pts',(14.2763577914438,19.1920394271468,72.37988723703));
#44792=CARTESIAN_POINT('Ctrl Pts',(14.2471849704709,19.3860037650969,72.354242145795));
#44793=CARTESIAN_POINT('Ctrl Pts',(14.2249320231436,19.4823795011934,72.3347583749636));
#44794=CARTESIAN_POINT('Ctrl Pts',(14.1362038196909,19.7594380075451,72.2585860295575));
#44795=CARTESIAN_POINT('Ctrl Pts',(14.0464667888171,19.9277656902715,72.1833081799824));
#44796=CARTESIAN_POINT('Ctrl Pts',(13.8352776378501,20.193547206592,72.0175354868236));
#44797=CARTESIAN_POINT('Ctrl Pts',(13.699571421043,20.3089065123171,71.9159238588941));
#44798=CARTESIAN_POINT('Ctrl Pts',(13.4702718108381,20.4238367380946,71.7589489349143));
#44799=CARTESIAN_POINT('Ctrl Pts',(13.3896280268035,20.4528504393822,71.7058714058911));
#44800=CARTESIAN_POINT('Ctrl Pts',(13.2253894088528,20.4909365811355,71.6024109718344));
#44801=CARTESIAN_POINT('Ctrl Pts',(13.1417904888991,20.5,71.5520312323997));
#44802=CARTESIAN_POINT('Ctrl Pts',(12.9782095111009,20.5,71.4575877108337));
#44803=CARTESIAN_POINT('Ctrl Pts',(12.8927799169376,20.4909365811355,71.4103787921422));
#44804=CARTESIAN_POINT('Ctrl Pts',(12.7210612437826,20.4528504393822,71.3198741937427));
#44805=CARTESIAN_POINT('Ctrl Pts',(12.6347728632611,20.4238367380946,71.2765733926231));
#44806=CARTESIAN_POINT('Ctrl Pts',(12.384178786235,20.3089065123171,71.1564815670977));
#44807=CARTESIAN_POINT('Ctrl Pts',(12.2283274267246,20.193547206592,71.0897623498559));
#44808=CARTESIAN_POINT('Ctrl Pts',(11.9791694877118,19.9277656902715,70.9897535266942));
#44809=CARTESIAN_POINT('Ctrl Pts',(11.8691084422006,19.7594380075451,70.9496779030849));
#44810=CARTESIAN_POINT('Ctrl Pts',(11.7587771542868,19.4823795011934,70.9109231975657));
#44811=CARTESIAN_POINT('Ctrl Pts',(11.7307772401216,19.3860037650969,70.901393465287));
#44812=CARTESIAN_POINT('Ctrl Pts',(11.6939815291433,19.1920394271468,70.8889516068419));
#44813=CARTESIAN_POINT('Ctrl Pts',(11.6851965084981,19.0944488139725,70.8860389693211));
#44814=CARTESIAN_POINT('Ctrl Pts',(11.6851965084981,19.,70.8860389693211));
#44815=CARTESIAN_POINT('Ctrl Pts',(9.30967733958527,14.8450000545077,81.0024999826628));
#44816=CARTESIAN_POINT('Ctrl Pts',(9.49399963863882,14.8449377785778,81.0025197906594));
#44817=CARTESIAN_POINT('Ctrl Pts',(9.8599726667903,14.9548208468277,80.9647069817074));
#44818=CARTESIAN_POINT('Ctrl Pts',(10.1635903263261,15.313863273745,80.8797718802955));
#44819=CARTESIAN_POINT('Ctrl Pts',(10.2636542832646,15.6732395795295,80.8470492838448));
#44820=CARTESIAN_POINT('Ctrl Pts',(10.2585828488274,16.0491061870486,80.8485595236358));
#44821=CARTESIAN_POINT('Ctrl Pts',(10.1358339345559,16.3074452995727,80.8893379358817));
#44822=CARTESIAN_POINT('Ctrl Pts',(9.99531238077664,16.4635283817546,80.9233309936752));
#44823=CARTESIAN_POINT('Ctrl Pts',(9.97541394843821,16.4837399726203,80.927922801608));
#44824=CARTESIAN_POINT('Ctrl Pts',(9.8715454189663,16.5803680094737,80.9507853431027));
#44825=CARTESIAN_POINT('Ctrl Pts',(9.66533594109898,16.7118893446204,80.988220546323));
#44826=CARTESIAN_POINT('Ctrl Pts',(9.39513127992021,16.760496532074,81.0043748388839));
#44827=CARTESIAN_POINT('Ctrl Pts',(9.22386882135598,16.7525596923286,81.0017749459923));
#44828=CARTESIAN_POINT('Ctrl Pts',(9.10596245168451,16.7364763479619,80.9967260931912));
#44829=CARTESIAN_POINT('Ctrl Pts',(8.90305460225939,16.6788818244957,80.9788324346323));
#44830=CARTESIAN_POINT('Ctrl Pts',(8.74872208287691,16.5802588408379,80.9509216345009));
#44831=CARTESIAN_POINT('Ctrl Pts',(8.52753199996129,16.3746224120349,80.9025147999549));
#44832=CARTESIAN_POINT('Ctrl Pts',(8.32895235429463,16.0324014611137,80.8376717466604));
#44833=CARTESIAN_POINT('Ctrl Pts',(8.37228193702135,15.425412033927,80.8539764039352));
#44834=CARTESIAN_POINT('Ctrl Pts',(8.67833944769248,15.0414439730474,80.9436419813148));
#44835=CARTESIAN_POINT('Ctrl Pts',(9.02217645440192,14.8743106493543,80.9926787754169));
#44836=CARTESIAN_POINT('Ctrl Pts',(9.21392517477995,14.8450324057486,81.00248969276));
#44837=CARTESIAN_POINT('Ctrl Pts',(9.30967733958527,14.8450000545077,81.0024999826628));
#44838=CARTESIAN_POINT('Ctrl Pts',(9.30968970356266,14.8950000532224,81.0524999841305));
#44839=CARTESIAN_POINT('Ctrl Pts',(9.48694528401203,14.8947370356301,81.0524949998533));
#44840=CARTESIAN_POINT('Ctrl Pts',(9.83862077660686,15.0031144336227,81.0177967437848));
#44841=CARTESIAN_POINT('Ctrl Pts',(10.1232202750603,15.3462669734862,80.9409650825406));
#44842=CARTESIAN_POINT('Ctrl Pts',(10.2153941656315,15.6820641892916,80.9118514108146));
#44843=CARTESIAN_POINT('Ctrl Pts',(10.2108309919214,16.0317404696965,80.9131375839316));
#44844=CARTESIAN_POINT('Ctrl Pts',(10.0973923997464,16.2744031824593,80.9496392785122));
#44845=CARTESIAN_POINT('Ctrl Pts',(9.96503976415596,16.4235992138869,80.9803887350985));
#44846=CARTESIAN_POINT('Ctrl Pts',(9.94625219275646,16.4428812429394,80.984549686419));
#44847=CARTESIAN_POINT('Ctrl Pts',(9.84806730694828,16.5354259082215,81.0052823264233));
#44848=CARTESIAN_POINT('Ctrl Pts',(9.65171070267945,16.6627611502429,81.039406645323));
#44849=CARTESIAN_POINT('Ctrl Pts',(9.39189564693647,16.7104082463205,81.0542222672945));
#44850=CARTESIAN_POINT('Ctrl Pts',(9.22714789308243,16.7026045728515,81.0518450119684));
#44851=CARTESIAN_POINT('Ctrl Pts',(9.11386983193031,16.6869539104283,81.0472385997827));
#44852=CARTESIAN_POINT('Ctrl Pts',(8.91905457715012,16.6307128161155,81.0308207592159));
#44853=CARTESIAN_POINT('Ctrl Pts',(8.77233148999154,16.5354389845187,81.0054772661211));
#44854=CARTESIAN_POINT('Ctrl Pts',(8.56280532687061,16.3380842628862,80.9614017072328));
#44855=CARTESIAN_POINT('Ctrl Pts',(8.37950980214853,16.0152517876383,80.9035554548782));
#44856=CARTESIAN_POINT('Ctrl Pts',(8.41869689342038,15.4524118992523,80.9178658102062));
#44857=CARTESIAN_POINT('Ctrl Pts',(8.7042245777961,15.0861817681023,80.9985551299171));
#44858=CARTESIAN_POINT('Ctrl Pts',(9.03346590578496,14.9235641805984,81.0436043674832));
#44859=CARTESIAN_POINT('Ctrl Pts',(9.21745201882799,14.895086151504,81.0524111931971));
#44860=CARTESIAN_POINT('Ctrl Pts',(9.30968970356266,14.8950000532224,81.0524999841305));
#44861=CARTESIAN_POINT('Ctrl Pts',(9.30970206754004,14.9450000519371,81.1024999855982));
#44862=CARTESIAN_POINT('Ctrl Pts',(9.47990202593708,14.9451429231465,81.102539555259));
#44863=CARTESIAN_POINT('Ctrl Pts',(9.81719222545616,15.0510938587472,81.0708839943767));
#44864=CARTESIAN_POINT('Ctrl Pts',(10.082929561504,15.3789703241095,81.0021370479354));
#44865=CARTESIAN_POINT('Ctrl Pts',(10.1671718631524,15.6910626190305,80.9766251480691));
#44866=CARTESIAN_POINT('Ctrl Pts',(10.1629882783727,16.0143158338321,80.9777373292404));
#44867=CARTESIAN_POINT('Ctrl Pts',(10.0589372173338,16.2419140185898,81.0098891375199));
#44868=CARTESIAN_POINT('Ctrl Pts',(9.93468300206258,16.3835400150001,81.0374294022131));
#44869=CARTESIAN_POINT('Ctrl Pts',(9.91702810156538,16.4020006342589,81.0411540570315));
#44870=CARTESIAN_POINT('Ctrl Pts',(9.82447906807606,16.4904948345281,81.0597504804512));
#44871=CARTESIAN_POINT('Ctrl Pts',(9.6380201680922,16.613611387635,81.0905702398648));
#44872=CARTESIAN_POINT('Ctrl Pts',(9.3884855334551,16.6602375621895,81.1040231423092));
#44873=CARTESIAN_POINT('Ctrl Pts',(9.23037903157421,16.6526560365432,81.1018484321131));
#44874=CARTESIAN_POINT('Ctrl Pts',(9.12160324597793,16.6373382197703,81.0976495064985));
#44875=CARTESIAN_POINT('Ctrl Pts',(8.93517297178808,16.5827079559131,81.0828394981346));
#44876=CARTESIAN_POINT('Ctrl Pts',(8.79555624957257,16.4904071185435,81.0598179414916));
#44877=CARTESIAN_POINT('Ctrl Pts',(8.5984073178612,16.3020445325207,81.0204404594761));
#44878=CARTESIAN_POINT('Ctrl Pts',(8.42959604077383,15.9978112453145,80.969179699637));
#44879=CARTESIAN_POINT('Ctrl Pts',(8.4652692759342,15.479755280664,80.9818504274788));
#44880=CARTESIAN_POINT('Ctrl Pts',(8.73064802942305,15.1307315854457,81.0537405736822));
#44881=CARTESIAN_POINT('Ctrl Pts',(9.04447343955803,14.9729914718726,81.0943901114622));
#44882=CARTESIAN_POINT('Ctrl Pts',(9.22144276309338,14.9449763675702,81.1025708100384));
#44883=CARTESIAN_POINT('Ctrl Pts',(9.30970206754004,14.9450000519371,81.1024999855982));
#44884=CARTESIAN_POINT('Ctrl Pts',(9.30971443151743,14.9950000506518,81.1524999870659));
#44885=CARTESIAN_POINT('Ctrl Pts',(9.47284767131029,14.9949421801988,81.1525147644529));
#44886=CARTESIAN_POINT('Ctrl Pts',(9.79584033527272,15.0993874455422,81.1239737564541));
#44887=CARTESIAN_POINT('Ctrl Pts',(10.0425595102383,15.4113740238506,81.0633302501805));
#44888=CARTESIAN_POINT('Ctrl Pts',(10.1189117455193,15.6998872287926,81.0414272750389));
#44889=CARTESIAN_POINT('Ctrl Pts',(10.1152364214667,15.99695011648,81.0423153895362));
#44890=CARTESIAN_POINT('Ctrl Pts',(10.0204956825243,16.2088719014764,81.0701904801504));
#44891=CARTESIAN_POINT('Ctrl Pts',(9.9044103854419,16.3436108471324,81.0944871436364));
#44892=CARTESIAN_POINT('Ctrl Pts',(9.88786634588363,16.361141904578,81.0977809418426));
#44893=CARTESIAN_POINT('Ctrl Pts',(9.80100095605804,16.4455527332759,81.1142474637718));
#44894=CARTESIAN_POINT('Ctrl Pts',(9.62439492967267,16.5644831932575,81.1417563388649));
#44895=CARTESIAN_POINT('Ctrl Pts',(9.38524990047136,16.6101492764359,81.1538705707198));
#44896=CARTESIAN_POINT('Ctrl Pts',(9.23365810330067,16.6027009170661,81.1519184980892));
#44897=CARTESIAN_POINT('Ctrl Pts',(9.12951062622373,16.5878157822367,81.1481620130899));
#44898=CARTESIAN_POINT('Ctrl Pts',(8.9511729466788,16.5345389475329,81.1348278227182));
#44899=CARTESIAN_POINT('Ctrl Pts',(8.8191656566872,16.4455872622242,81.1143735731117));
#44900=CARTESIAN_POINT('Ctrl Pts',(8.63368064477052,16.265506383372,81.0793273667541));
#44901=CARTESIAN_POINT('Ctrl Pts',(8.48015348862773,15.9806615718392,81.0350634078547));
#44902=CARTESIAN_POINT('Ctrl Pts',(8.51168423233323,15.5067551459893,81.0457398337499));
#44903=CARTESIAN_POINT('Ctrl Pts',(8.75653315952666,15.1754693805007,81.1086537222845));
#44904=CARTESIAN_POINT('Ctrl Pts',(9.05576289094108,15.0222450031167,81.1453157035286));
#44905=CARTESIAN_POINT('Ctrl Pts',(9.22496960714143,14.9950301133256,81.1524923104755));
#44906=CARTESIAN_POINT('Ctrl Pts',(9.30971443151743,14.9950000506518,81.1524999870659));
#44907=CARTESIAN_POINT('',(9.30967733958527,14.8450000545077,81.0024999826628));
#44908=CARTESIAN_POINT('',(9.30967733958527,14.8450000545077,81.0024999826628));
#44909=CARTESIAN_POINT('',(8.76439716203066,16.5827816051055,80.9526008949626));
#44910=CARTESIAN_POINT('Ctrl Pts',(9.30967733958527,14.8450000545077,81.0024999826628));
#44911=CARTESIAN_POINT('Ctrl Pts',(9.21392517477995,14.8450324057486,81.00248969276));
#44912=CARTESIAN_POINT('Ctrl Pts',(9.02217645440192,14.8743106493543,80.9926787754169));
#44913=CARTESIAN_POINT('Ctrl Pts',(8.67833944769248,15.0414439730474,80.9436419813148));
#44914=CARTESIAN_POINT('Ctrl Pts',(8.37228193702135,15.425412033927,80.8539764039352));
#44915=CARTESIAN_POINT('Ctrl Pts',(8.32895235429463,16.0324014611137,80.8376717466604));
#44916=CARTESIAN_POINT('Ctrl Pts',(8.52753199996129,16.3746224120349,80.9025147999549));
#44917=CARTESIAN_POINT('Ctrl Pts',(8.69606757651563,16.5313068964027,80.9393983422089));
#44918=CARTESIAN_POINT('Ctrl Pts',(8.72917682559677,16.5580725998915,80.9461192566062));
#44919=CARTESIAN_POINT('Ctrl Pts',(8.76439716203066,16.5827816051055,80.9526008949626));
#44920=CARTESIAN_POINT('',(9.8558137849654,16.5828640996264,80.9524659608699));
#44921=CARTESIAN_POINT('Ctrl Pts',(8.76439716203066,16.5827816051055,80.9526008949626));
#44922=CARTESIAN_POINT('Ctrl Pts',(8.82529403548109,16.6255041147677,80.9638078154724));
#44923=CARTESIAN_POINT('Ctrl Pts',(8.94554131631809,16.6909414961979,80.9825791736412));
#44924=CARTESIAN_POINT('Ctrl Pts',(9.10596245168451,16.7364763479619,80.9967260931912));
#44925=CARTESIAN_POINT('Ctrl Pts',(9.22386882135598,16.7525596923286,81.0017749459923));
#44926=CARTESIAN_POINT('Ctrl Pts',(9.39513127992021,16.760496532074,81.0043748388839));
#44927=CARTESIAN_POINT('Ctrl Pts',(9.62133087647619,16.7198054272509,80.9908514065198));
#44928=CARTESIAN_POINT('Ctrl Pts',(9.79484346501603,16.6255969681486,80.9637281582169));
#44929=CARTESIAN_POINT('Ctrl Pts',(9.8558137849654,16.5828640996264,80.9524659608699));
#44930=CARTESIAN_POINT('Ctrl Pts',(9.8558137849654,16.5828640996264,80.9524659608699));
#44931=CARTESIAN_POINT('Ctrl Pts',(9.8910765999414,16.5581491032586,80.9459523525831));
#44932=CARTESIAN_POINT('Ctrl Pts',(9.92422356777855,16.5313619618221,80.9391903357486));
#44933=CARTESIAN_POINT('Ctrl Pts',(9.97541394843821,16.4837399726203,80.927922801608));
#44934=CARTESIAN_POINT('Ctrl Pts',(9.99531238077664,16.4635283817546,80.9233309936752));
#44935=CARTESIAN_POINT('Ctrl Pts',(10.1358339345559,16.3074452995727,80.8893379358817));
#44936=CARTESIAN_POINT('Ctrl Pts',(10.2585828488274,16.0491061870486,80.8485595236358));
#44937=CARTESIAN_POINT('Ctrl Pts',(10.2636542832646,15.6732395795295,80.8470492838448));
#44938=CARTESIAN_POINT('Ctrl Pts',(10.1635903263261,15.313863273745,80.8797718802955));
#44939=CARTESIAN_POINT('Ctrl Pts',(9.8599726667903,14.9548208468277,80.9647069817074));
#44940=CARTESIAN_POINT('Ctrl Pts',(9.49399963863882,14.8449377785778,81.0025197906594));
#44941=CARTESIAN_POINT('Ctrl Pts',(9.30967733958527,14.8450000545077,81.0024999826628));
#44942=CARTESIAN_POINT('Origin',(9.31,18.775,78.));
#44943=CARTESIAN_POINT('',(6.3075,14.15,78.));
#44944=CARTESIAN_POINT('Origin',(9.31,14.15,78.));
#44945=CARTESIAN_POINT('',(6.3075,23.4,78.));
#44946=CARTESIAN_POINT('',(6.3075,18.775,78.));
#44947=CARTESIAN_POINT('Origin',(9.31,23.4,78.));
#44948=CARTESIAN_POINT('Origin',(9.31,19.,78.));
#44949=CARTESIAN_POINT('',(9.31,19.,97.2));
#44950=CARTESIAN_POINT('Origin',(9.31,19.,99.));
#44951=CARTESIAN_POINT('',(1.0383798211071,19.,95.3268664107545));
#44952=CARTESIAN_POINT('Origin',(9.31,19.,78.));
#44953=CARTESIAN_POINT('',(-1.55969639024622,19.,93.8268664107545));
#44954=CARTESIAN_POINT('Ctrl Pts',(-1.55969639024622,19.,93.8268664107545));
#44955=CARTESIAN_POINT('Ctrl Pts',(-1.55969639024622,19.1298398798308,93.8268664107545));
#44956=CARTESIAN_POINT('Ctrl Pts',(-1.55286934050649,19.2576342464927,93.8486597278194));
#44957=CARTESIAN_POINT('Ctrl Pts',(-1.52254836481685,19.5361665210634,93.9423766588895));
#44958=CARTESIAN_POINT('Ctrl Pts',(-1.49582215684855,19.6785504797858,94.0239193323177));
#44959=CARTESIAN_POINT('Ctrl Pts',(-1.41151331058044,19.9800578502247,94.2616163590086));
#44960=CARTESIAN_POINT('Ctrl Pts',(-1.34726058145713,20.1214477955687,94.4315221156896));
#44961=CARTESIAN_POINT('Ctrl Pts',(-1.18695676759168,20.3384257002779,94.7741079267736));
#44962=CARTESIAN_POINT('Ctrl Pts',(-1.08872043557327,20.4154002764241,94.9509005045226));
#44963=CARTESIAN_POINT('Ctrl Pts',(-0.91501820464108,20.4756548309858,95.1525146204047));
#44964=CARTESIAN_POINT('Ctrl Pts',(-0.860662478856494,20.4878793574952,
95.20581219399));
#44965=CARTESIAN_POINT('Ctrl Pts',(-0.758171101748774,20.4989413461778,
95.2849671751815));
#44966=CARTESIAN_POINT('Ctrl Pts',(-0.714349205355399,20.5007261344951,
95.3135640992347));
#44967=CARTESIAN_POINT('Ctrl Pts',(-0.617576626276311,20.4986621094877,
95.3656661602697));
#44968=CARTESIAN_POINT('Ctrl Pts',(-0.5654286151719,20.4943583996059,95.3878690863923));
#44969=CARTESIAN_POINT('Ctrl Pts',(-0.413657365059915,20.4735716734213,
95.4385197926724));
#44970=CARTESIAN_POINT('Ctrl Pts',(-0.31263191661929,20.4502685845107,95.4563416379516));
#44971=CARTESIAN_POINT('Ctrl Pts',(-0.0789744689677987,20.3775229034925,
95.4774958870508));
#44972=CARTESIAN_POINT('Ctrl Pts',(0.061044700769779,20.3188989837733,95.4741371363919));
#44973=CARTESIAN_POINT('Ctrl Pts',(0.393973711379464,20.1330764472051,95.4477411901324));
#44974=CARTESIAN_POINT('Ctrl Pts',(0.58454770192275,19.9855206415407,95.4165926999351));
#44975=CARTESIAN_POINT('Ctrl Pts',(0.847937571353683,19.6626095831238,95.3677669972487));
#44976=CARTESIAN_POINT('Ctrl Pts',(0.936366028690045,19.5066066529301,95.3489694894714));
#44977=CARTESIAN_POINT('Ctrl Pts',(1.02128074726238,19.2262024684657,95.3306789801616));
#44978=CARTESIAN_POINT('Ctrl Pts',(1.03837982110709,19.1137113861875,95.3268664107545));
#44979=CARTESIAN_POINT('Ctrl Pts',(1.03837982110709,19.,95.3268664107545));
#44980=CARTESIAN_POINT('',(-9.83131656913913,19.,79.5));
#44981=CARTESIAN_POINT('Origin',(9.31,19.,78.));
#44982=CARTESIAN_POINT('',(-9.83131656913913,19.,76.5));
#44983=CARTESIAN_POINT('Ctrl Pts',(-9.83131656913913,19.,76.5));
#44984=CARTESIAN_POINT('Ctrl Pts',(-9.83131656913913,19.1245217970218,76.5));
#44985=CARTESIAN_POINT('Ctrl Pts',(-9.84554380418068,19.2486348123039,76.5154677646786));
#44986=CARTESIAN_POINT('Ctrl Pts',(-9.90682498456632,19.5152363108006,76.5833051354963));
#44987=CARTESIAN_POINT('Ctrl Pts',(-9.95871278232153,19.6513770277057,76.6411156315615));
#44988=CARTESIAN_POINT('Ctrl Pts',(-10.1026555664131,19.9291519129669,76.8087481691482));
#44989=CARTESIAN_POINT('Ctrl Pts',(-10.2014133131777,20.0630977664656,76.9273940576885));
#44990=CARTESIAN_POINT('Ctrl Pts',(-10.4149894821051,20.2954859145557,77.2185345135431));
#44991=CARTESIAN_POINT('Ctrl Pts',(-10.5280386633462,20.3847092201747,77.3927468017688));
#44992=CARTESIAN_POINT('Ctrl Pts',(-10.6573116577679,20.4769000895387,77.7049195202664));
#44993=CARTESIAN_POINT('Ctrl Pts',(-10.6848483892464,20.4935592903711,77.8229433494293));
#44994=CARTESIAN_POINT('Ctrl Pts',(-10.7001274699635,20.5032447555465,78.0385628545257));
#44995=CARTESIAN_POINT('Ctrl Pts',(-10.6896585844537,20.4969058005831,78.1429558632871));
#44996=CARTESIAN_POINT('Ctrl Pts',(-10.6331076337369,20.4596343864514,78.3660543960096));
#44997=CARTESIAN_POINT('Ctrl Pts',(-10.5835751290906,20.4257618686536,78.4798599905703));
#44998=CARTESIAN_POINT('Ctrl Pts',(-10.4408937377185,20.3131243051215,78.7457519131079));
#44999=CARTESIAN_POINT('Ctrl Pts',(-10.3291283199371,20.2132427857327,78.9037637004356));
#45000=CARTESIAN_POINT('Ctrl Pts',(-10.1184813956406,19.9505788790836,79.1742528903653));
#45001=CARTESIAN_POINT('Ctrl Pts',(-10.0216936341199,19.7964852740788,79.2865908485361));
#45002=CARTESIAN_POINT('Ctrl Pts',(-9.89489746957705,19.4764502513109,79.4303757672511));
#45003=CARTESIAN_POINT('Ctrl Pts',(-9.85522800261023,19.3240506827592,79.4737983676688));
#45004=CARTESIAN_POINT('Ctrl Pts',(-9.83395109612093,19.1071959085279,79.4971214837868));
#45005=CARTESIAN_POINT('Ctrl Pts',(-9.83131656913913,19.0536635113807,79.5));
#45006=CARTESIAN_POINT('Ctrl Pts',(-9.83131656913913,19.,79.5));
#45007=CARTESIAN_POINT('',(-1.55969639024623,19.,62.1731335892455));
#45008=CARTESIAN_POINT('Origin',(9.31,19.,78.));
#45009=CARTESIAN_POINT('',(1.03837982110709,19.,60.6731335892455));
#45010=CARTESIAN_POINT('Ctrl Pts',(1.03837982110709,19.,60.6731335892455));
#45011=CARTESIAN_POINT('Ctrl Pts',(1.03837982110709,19.1298398798308,60.6731335892455));
#45012=CARTESIAN_POINT('Ctrl Pts',(1.01609273002626,19.2576342464927,60.6681493292206));
#45013=CARTESIAN_POINT('Ctrl Pts',(0.919770999110034,19.5361665210635,60.6475495989003));
#45014=CARTESIAN_POINT('Ctrl Pts',(0.835789868444578,19.6785504797858,60.6299238372336));
#45015=CARTESIAN_POINT('Ctrl Pts',(0.587783781791739,19.9800578502252,60.58408892652));
#45016=CARTESIAN_POINT('Ctrl Pts',(0.408514715694908,20.1214477955691,60.5547805438627));
#45017=CARTESIAN_POINT('Ctrl Pts',(0.0316747933878957,20.338425700278,60.5223148134518));
#45018=CARTESIAN_POINT('Ctrl Pts',(-0.170550236152408,20.4154002764241,
60.5189936836799));
#45019=CARTESIAN_POINT('Ctrl Pts',(-0.432004297734002,20.4756548309859,
60.5686171704201));
#45020=CARTESIAN_POINT('Ctrl Pts',(-0.505339213311197,20.4878793574952,
60.5890418229981));
#45021=CARTESIAN_POINT('Ctrl Pts',(-0.625135126412895,20.4989413461778,
60.6382244686464));
#45022=CARTESIAN_POINT('Ctrl Pts',(-0.671811737309813,20.5007261344951,
60.6618768821385));
#45023=CARTESIAN_POINT('Ctrl Pts',(-0.765319735295206,20.4986621094877,
60.7196333634933));
#45024=CARTESIAN_POINT('Ctrl Pts',(-0.810622038907963,20.4943583996059,
60.7536934028052));
#45025=CARTESIAN_POINT('Ctrl Pts',(-0.930372462322086,20.4735716734213,
60.8598058078263));
#45026=CARTESIAN_POINT('Ctrl Pts',(-0.996319357296532,20.4502685845106,
60.9383854899651));
#45027=CARTESIAN_POINT('Ctrl Pts',(-1.13146819824008,20.3775229034925,61.1301616508649));
#45028=CARTESIAN_POINT('Ctrl Pts',(-1.19856901971327,20.3188989837734,61.2531011842039));
#45029=CARTESIAN_POINT('Ctrl Pts',(-1.3421739650006,20.133076447205,61.5546241381787));
#45030=CARTESIAN_POINT('Ctrl Pts',(-1.41048557647178,19.9855206415405,61.7352403003884));
#45031=CARTESIAN_POINT('Ctrl Pts',(-1.49989621230313,19.6626095831239,61.9877554697581));
#45032=CARTESIAN_POINT('Ctrl Pts',(-1.52783132170843,19.5066066529302,62.0737355141175));
#45033=CARTESIAN_POINT('Ctrl Pts',(-1.55444863528416,19.2262024684657,62.1564190722112));
#45034=CARTESIAN_POINT('Ctrl Pts',(-1.55969639024623,19.1137113861875,62.1731335892455));
#45035=CARTESIAN_POINT('Ctrl Pts',(-1.55969639024623,19.,62.1731335892455));
#45036=CARTESIAN_POINT('',(17.5816201788929,19.,60.6731335892455));
#45037=CARTESIAN_POINT('Origin',(9.31,19.,78.));
#45038=CARTESIAN_POINT('',(20.1796963902462,19.,62.1731335892455));
#45039=CARTESIAN_POINT('Ctrl Pts',(20.1796963902462,19.,62.1731335892455));
#45040=CARTESIAN_POINT('Ctrl Pts',(20.1796963902462,19.1298398798308,62.1731335892455));
#45041=CARTESIAN_POINT('Ctrl Pts',(20.1728693405065,19.2576342464928,62.1513402721806));
#45042=CARTESIAN_POINT('Ctrl Pts',(20.1425483648168,19.5361665210635,62.0576233411105));
#45043=CARTESIAN_POINT('Ctrl Pts',(20.1158221568485,19.6785504797858,61.9760806676823));
#45044=CARTESIAN_POINT('Ctrl Pts',(20.0315133105802,19.9800578502254,61.7383836409908));
#45045=CARTESIAN_POINT('Ctrl Pts',(19.9672605814568,20.1214477955692,61.5684778843096));
#45046=CARTESIAN_POINT('Ctrl Pts',(19.8069567675917,20.3384257002779,61.2258920732264));
#45047=CARTESIAN_POINT('Ctrl Pts',(19.7087204355733,20.4154002764241,61.0490994954775));
#45048=CARTESIAN_POINT('Ctrl Pts',(19.535018204641,20.4756548309859,60.8474853795952));
#45049=CARTESIAN_POINT('Ctrl Pts',(19.4806624788565,20.4878793574952,60.79418780601));
#45050=CARTESIAN_POINT('Ctrl Pts',(19.3781711017488,20.4989413461778,60.7150328248185));
#45051=CARTESIAN_POINT('Ctrl Pts',(19.3343492053554,20.5007261344951,60.6864359007653));
#45052=CARTESIAN_POINT('Ctrl Pts',(19.2375766262763,20.4986621094877,60.6343338397303));
#45053=CARTESIAN_POINT('Ctrl Pts',(19.1854286151718,20.4943583996059,60.6121309136077));
#45054=CARTESIAN_POINT('Ctrl Pts',(19.0336573650599,20.4735716734213,60.5614802073276));
#45055=CARTESIAN_POINT('Ctrl Pts',(18.9326319166192,20.4502685845106,60.5436583620484));
#45056=CARTESIAN_POINT('Ctrl Pts',(18.6989744689681,20.3775229034925,60.5225041129492));
#45057=CARTESIAN_POINT('Ctrl Pts',(18.5589552992305,20.3188989837735,60.5258628636081));
#45058=CARTESIAN_POINT('Ctrl Pts',(18.2260262886202,20.1330764472049,60.5522588098677));
#45059=CARTESIAN_POINT('Ctrl Pts',(18.035452298077,19.9855206415404,60.583407300065));
#45060=CARTESIAN_POINT('Ctrl Pts',(17.7720624286463,19.6626095831238,60.6322330027514));
#45061=CARTESIAN_POINT('Ctrl Pts',(17.68363397131,19.5066066529301,60.6510305105286));
#45062=CARTESIAN_POINT('Ctrl Pts',(17.5987192527376,19.2262024684657,60.6693210198384));
#45063=CARTESIAN_POINT('Ctrl Pts',(17.5816201788929,19.1137113861875,60.6731335892455));
#45064=CARTESIAN_POINT('Ctrl Pts',(17.5816201788929,19.,60.6731335892455));
#45065=CARTESIAN_POINT('',(28.4513165691391,19.,76.5));
#45066=CARTESIAN_POINT('Origin',(9.31,19.,78.));
#45067=CARTESIAN_POINT('',(28.4513165691391,19.,79.5));
#45068=CARTESIAN_POINT('Ctrl Pts',(28.4513165691391,19.,79.5));
#45069=CARTESIAN_POINT('Ctrl Pts',(28.4513165691391,19.1245217970218,79.5));
#45070=CARTESIAN_POINT('Ctrl Pts',(28.4655438041807,19.248634812304,79.4845322353214));
#45071=CARTESIAN_POINT('Ctrl Pts',(28.5268249845663,19.5152363108006,79.4166948645036));
#45072=CARTESIAN_POINT('Ctrl Pts',(28.5787127823215,19.6513770277057,79.3588843684386));
#45073=CARTESIAN_POINT('Ctrl Pts',(28.7226555664131,19.9291519129669,79.1912518308518));
#45074=CARTESIAN_POINT('Ctrl Pts',(28.8214133131777,20.0630977664656,79.0726059423115));
#45075=CARTESIAN_POINT('Ctrl Pts',(29.0349894821052,20.2954859145559,78.7814654864567));
#45076=CARTESIAN_POINT('Ctrl Pts',(29.1480386633463,20.3847092201747,78.607253198231));
#45077=CARTESIAN_POINT('Ctrl Pts',(29.2773116577678,20.4769000895386,78.2950804797337));
#45078=CARTESIAN_POINT('Ctrl Pts',(29.3048483892464,20.4935592903711,78.1770566505708));
#45079=CARTESIAN_POINT('Ctrl Pts',(29.3201274699635,20.5032447555465,77.9614371454743));
#45080=CARTESIAN_POINT('Ctrl Pts',(29.3096585844537,20.4969058005831,77.8570441367129));
#45081=CARTESIAN_POINT('Ctrl Pts',(29.2531076337369,20.4596343864514,77.6339456039904));
#45082=CARTESIAN_POINT('Ctrl Pts',(29.2035751290906,20.4257618686536,77.5201400094297));
#45083=CARTESIAN_POINT('Ctrl Pts',(29.0608937377183,20.3131243051213,77.2542480868917));
#45084=CARTESIAN_POINT('Ctrl Pts',(28.9491283199369,20.2132427857324,77.0962362995642));
#45085=CARTESIAN_POINT('Ctrl Pts',(28.7384813956406,19.9505788790835,76.8257471096347));
#45086=CARTESIAN_POINT('Ctrl Pts',(28.6416936341199,19.7964852740788,76.7134091514639));
#45087=CARTESIAN_POINT('Ctrl Pts',(28.5148974695771,19.4764502513109,76.5696242327489));
#45088=CARTESIAN_POINT('Ctrl Pts',(28.4752280026102,19.3240506827592,76.5262016323312));
#45089=CARTESIAN_POINT('Ctrl Pts',(28.4539510961209,19.1071959085279,76.5028785162132));
#45090=CARTESIAN_POINT('Ctrl Pts',(28.4513165691391,19.0536635113807,76.5));
#45091=CARTESIAN_POINT('Ctrl Pts',(28.4513165691391,19.,76.5));
#45092=CARTESIAN_POINT('',(20.1796963902462,19.,93.8268664107545));
#45093=CARTESIAN_POINT('Origin',(9.31,19.,78.));
#45094=CARTESIAN_POINT('',(17.5816201788929,19.,95.3268664107545));
#45095=CARTESIAN_POINT('Ctrl Pts',(17.5816201788929,19.,95.3268664107545));
#45096=CARTESIAN_POINT('Ctrl Pts',(17.5816201788929,19.1298398798308,95.3268664107545));
#45097=CARTESIAN_POINT('Ctrl Pts',(17.6039072699737,19.2576342464928,95.3318506707794));
#45098=CARTESIAN_POINT('Ctrl Pts',(17.70022900089,19.5361665210636,95.3524504010997));
#45099=CARTESIAN_POINT('Ctrl Pts',(17.7842101315555,19.6785504797859,95.3700761627664));
#45100=CARTESIAN_POINT('Ctrl Pts',(18.0322162182082,19.9800578502251,95.41591107348));
#45101=CARTESIAN_POINT('Ctrl Pts',(18.211485284305,20.121447795569,95.4452194561373));
#45102=CARTESIAN_POINT('Ctrl Pts',(18.5883252066121,20.338425700278,95.4776851865482));
#45103=CARTESIAN_POINT('Ctrl Pts',(18.7905502361524,20.4154002764241,95.4810063163201));
#45104=CARTESIAN_POINT('Ctrl Pts',(19.0520042977342,20.4756548309859,95.4313828295798));
#45105=CARTESIAN_POINT('Ctrl Pts',(19.1253392133113,20.4878793574952,95.4109581770019));
#45106=CARTESIAN_POINT('Ctrl Pts',(19.2451351264128,20.4989413461777,95.3617755313536));
#45107=CARTESIAN_POINT('Ctrl Pts',(19.2918117373098,20.5007261344951,95.3381231178615));
#45108=CARTESIAN_POINT('Ctrl Pts',(19.3853197352953,20.4986621094877,95.2803666365067));
#45109=CARTESIAN_POINT('Ctrl Pts',(19.4306220389081,20.4943583996059,95.2463065971947));
#45110=CARTESIAN_POINT('Ctrl Pts',(19.5503724623221,20.4735716734213,95.1401941921737));
#45111=CARTESIAN_POINT('Ctrl Pts',(19.6163193572965,20.4502685845106,95.0616145100349));
#45112=CARTESIAN_POINT('Ctrl Pts',(19.75146819824,20.3775229034925,94.8698383491352));
#45113=CARTESIAN_POINT('Ctrl Pts',(19.8185690197132,20.3188989837735,94.7468988157962));
#45114=CARTESIAN_POINT('Ctrl Pts',(19.9621739650008,20.1330764472048,94.4453758618209));
#45115=CARTESIAN_POINT('Ctrl Pts',(20.0304855764719,19.9855206415402,94.2647596996113));
#45116=CARTESIAN_POINT('Ctrl Pts',(20.1198962123032,19.6626095831237,94.0122445302418));
#45117=CARTESIAN_POINT('Ctrl Pts',(20.1478313217084,19.50660665293,93.9262644858825));
#45118=CARTESIAN_POINT('Ctrl Pts',(20.1744486352842,19.2262024684656,93.8435809277888));
#45119=CARTESIAN_POINT('Ctrl Pts',(20.1796963902462,19.1137113861874,93.8268664107545));
#45120=CARTESIAN_POINT('Ctrl Pts',(20.1796963902462,19.,93.8268664107545));
#45121=CARTESIAN_POINT('Origin',(9.31,19.,78.));
#45122=CARTESIAN_POINT('',(19.3125062814467,17.5,95.3248490824925));
#45123=CARTESIAN_POINT('Ctrl Pts',(19.3125062814467,17.5,95.3248490824925));
#45124=CARTESIAN_POINT('Ctrl Pts',(19.2653612797053,17.5,95.3520682619388));
#45125=CARTESIAN_POINT('Ctrl Pts',(19.2163882916827,17.502946735144,95.3749120396601));
#45126=CARTESIAN_POINT('Ctrl Pts',(19.0831906327501,17.5181479027027,95.424536757463));
#45127=CARTESIAN_POINT('Ctrl Pts',(18.9982617981722,17.5348232538744,95.4440603634893));
#45128=CARTESIAN_POINT('Ctrl Pts',(18.8009075569721,17.5875127881648,95.4720531545667));
#45129=CARTESIAN_POINT('Ctrl Pts',(18.6875380327356,17.6285240662611,95.4750565548865));
#45130=CARTESIAN_POINT('Ctrl Pts',(18.3942021353586,17.7623087481876,95.4666942719671));
#45131=CARTESIAN_POINT('Ctrl Pts',(18.2058843837797,17.8796864892639,95.4425232119164));
#45132=CARTESIAN_POINT('Ctrl Pts',(17.8971879945484,18.1666272894372,95.3925756323412));
#45133=CARTESIAN_POINT('Ctrl Pts',(17.7745791487004,18.3256026756653,95.3678345274791));
#45134=CARTESIAN_POINT('Ctrl Pts',(17.6273835423512,18.6468724886465,95.3370780178918));
#45135=CARTESIAN_POINT('Ctrl Pts',(17.5890720003775,18.7971695012231,95.3285089232078));
#45136=CARTESIAN_POINT('Ctrl Pts',(17.5819451644934,18.9686255097769,95.3269380887608));
#45137=CARTESIAN_POINT('Ctrl Pts',(17.5816201788929,18.984327656238,95.3268664107545));
#45138=CARTESIAN_POINT('Ctrl Pts',(17.5816201788929,19.,95.3268664107545));
#45139=CARTESIAN_POINT('Ctrl Pts',(20.1796963902462,19.,93.8268664107545));
#45140=CARTESIAN_POINT('Ctrl Pts',(20.1796963902462,18.9648000704088,93.8268664107545));
#45141=CARTESIAN_POINT('Ctrl Pts',(20.1791901743517,18.9294832054732,93.8284669499666));
#45142=CARTESIAN_POINT('Ctrl Pts',(20.1738795413826,18.7461724891623,93.8452165866068));
#45143=CARTESIAN_POINT('Ctrl Pts',(20.1608254414315,18.6040823417908,93.8866376596314));
#45144=CARTESIAN_POINT('Ctrl Pts',(20.1142713209593,18.3102983306061,94.0274111126068));
#45145=CARTESIAN_POINT('Ctrl Pts',(20.0777756307246,18.1669858887453,94.1349945295655));
#45146=CARTESIAN_POINT('Ctrl Pts',(19.9621359407356,17.8610717494632,94.441071667855));
#45147=CARTESIAN_POINT('Ctrl Pts',(19.8731660176324,17.7272792212461,94.6533728241667));
#45148=CARTESIAN_POINT('Ctrl Pts',(19.6971324340933,17.5873420162312,94.9529469331406));
#45149=CARTESIAN_POINT('Ctrl Pts',(19.6195169618968,17.5470806517564,95.0646162294015));
#45150=CARTESIAN_POINT('Ctrl Pts',(19.4787984488119,17.5125581835725,95.2059766108471));
#45151=CARTESIAN_POINT('Ctrl Pts',(19.4302635208502,17.5052303115316,95.2473360103154));
#45152=CARTESIAN_POINT('Ctrl Pts',(19.3561746798665,17.5006516995771,95.2984438337642));
#45153=CARTESIAN_POINT('Ctrl Pts',(19.3346302397217,17.5,95.3120758092269));
#45154=CARTESIAN_POINT('Ctrl Pts',(19.3125062814467,17.5,95.3248490824925));
#45155=CARTESIAN_POINT('',(29.3150125628934,17.5,78.));
#45156=CARTESIAN_POINT('Ctrl Pts',(29.3150125628934,17.5,78.));
#45157=CARTESIAN_POINT('Ctrl Pts',(29.3150125628934,17.5,78.1047390770919));
#45158=CARTESIAN_POINT('Ctrl Pts',(29.2974013907771,17.5108310402064,78.2071426028014));
#45159=CARTESIAN_POINT('Ctrl Pts',(29.226922072288,17.5583420169659,78.4339131995391));
#45160=CARTESIAN_POINT('Ctrl Pts',(29.1673418462476,17.6007431024611,78.5542198710694));
#45161=CARTESIAN_POINT('Ctrl Pts',(29.0020601635,17.7393206831897,78.83476146908));
#45162=CARTESIAN_POINT('Ctrl Pts',(28.8769173400547,17.8614426921814,79.0006494510307));
#45163=CARTESIAN_POINT('Ctrl Pts',(28.6701915527651,18.1597175199196,79.2546083244645));
#45164=CARTESIAN_POINT('Ctrl Pts',(28.5867105343723,18.3173213761021,79.3494913085985));
#45165=CARTESIAN_POINT('Ctrl Pts',(28.4853157633783,18.637591898099,79.4629623925713));
#45166=CARTESIAN_POINT('Ctrl Pts',(28.457609981235,18.7870280562669,79.4931146708418));
#45167=CARTESIAN_POINT('Ctrl Pts',(28.4516322653758,18.9628275273603,79.4996547399714));
#45168=CARTESIAN_POINT('Ctrl Pts',(28.4513165691391,18.9814183151259,79.5));
#45169=CARTESIAN_POINT('Ctrl Pts',(28.4513165691391,19.,79.5));
#45170=CARTESIAN_POINT('Ctrl Pts',(28.4513165691391,19.,76.5));
#45171=CARTESIAN_POINT('Ctrl Pts',(28.4513165691391,18.9077230153478,76.5));
#45172=CARTESIAN_POINT('Ctrl Pts',(28.4591147250101,18.8150583449374,76.5085002722188));
#45173=CARTESIAN_POINT('Ctrl Pts',(28.4993679863007,18.5791911526486,76.5528200938006));
#45174=CARTESIAN_POINT('Ctrl Pts',(28.5423240325381,18.4425366457864,76.6002411233075));
#45175=CARTESIAN_POINT('Ctrl Pts',(28.6668807891092,18.1638733921006,76.742921963351));
#45176=CARTESIAN_POINT('Ctrl Pts',(28.7539057616696,18.0287684620774,76.8450091634613));
#45177=CARTESIAN_POINT('Ctrl Pts',(28.9714335308102,17.7609964409145,77.1256645774523));
#45178=CARTESIAN_POINT('Ctrl Pts',(29.1032005944038,17.650192730897,77.3135344313333));
#45179=CARTESIAN_POINT('Ctrl Pts',(29.2538951387463,17.5385627946699,77.6365203536188));
#45180=CARTESIAN_POINT('Ctrl Pts',(29.292937166705,17.5140590169286,77.7600350329524));
#45181=CARTESIAN_POINT('Ctrl Pts',(29.3126407860379,17.5014920111156,77.9228715529961));
#45182=CARTESIAN_POINT('Ctrl Pts',(29.3150125628934,17.5,77.9613132360328));
#45183=CARTESIAN_POINT('Ctrl Pts',(29.3150125628934,17.5,78.));
#45184=CARTESIAN_POINT('',(19.3125062814467,17.5,60.6751509175075));
#45185=CARTESIAN_POINT('Ctrl Pts',(19.3125062814467,17.5,60.6751509175075));
#45186=CARTESIAN_POINT('Ctrl Pts',(19.359651283188,17.5,60.7023700969538));
#45187=CARTESIAN_POINT('Ctrl Pts',(19.4039210690243,17.502946735144,60.7333600598199));
#45188=CARTESIAN_POINT('Ctrl Pts',(19.5134961647636,17.5181479027027,60.8239002572788));
#45189=CARTESIAN_POINT('Ctrl Pts',(19.5728685208448,17.5348232538744,60.8876889825239));
#45190=CARTESIAN_POINT('Ctrl Pts',(19.6957881096408,17.5875127881649,61.0446063734092));
#45191=CARTESIAN_POINT('Ctrl Pts',(19.7550738927337,17.6285240662612,61.1412855612531));
#45192=CARTESIAN_POINT('Ctrl Pts',(19.8944998919804,17.7623087481876,61.3995030416831));
#45193=CARTESIAN_POINT('Ctrl Pts',(19.9677260157295,17.879686489264,61.5746765285594));
#45194=CARTESIAN_POINT('Ctrl Pts',(20.0788183375755,18.1666272894372,61.8669892334777));
#45195=CARTESIAN_POINT('Ctrl Pts',(20.1186963351712,18.3256026756653,61.9855421611418));
#45196=CARTESIAN_POINT('Ctrl Pts',(20.1656582197115,18.6468724886465,62.1283955503593));
#45197=CARTESIAN_POINT('Ctrl Pts',(20.1773929370146,18.7971695012231,62.1658588663088));
#45198=CARTESIAN_POINT('Ctrl Pts',(20.1795959724204,18.968625509777,62.1728163044565));
#45199=CARTESIAN_POINT('Ctrl Pts',(20.1796963902462,18.984327656238,62.1731335892455));
#45200=CARTESIAN_POINT('Ctrl Pts',(20.1796963902462,19.,62.1731335892455));
#45201=CARTESIAN_POINT('Ctrl Pts',(17.5816201788929,19.,60.6731335892455));
#45202=CARTESIAN_POINT('Ctrl Pts',(17.5816201788929,18.9648000704089,60.6731335892455));
#45203=CARTESIAN_POINT('Ctrl Pts',(17.5832593944576,18.9294832054732,60.6727717154639));
#45204=CARTESIAN_POINT('Ctrl Pts',(17.6004203217768,18.7461724891624,60.6689960402053));
#45205=CARTESIAN_POINT('Ctrl Pts',(17.6428190732436,18.604082341791,60.6595906858741));
#45206=CARTESIAN_POINT('Ctrl Pts',(17.7880095199348,18.3102983306063,60.6295210103662));
#45207=CARTESIAN_POINT('Ctrl Pts',(17.8994273371643,18.1669858887454,60.6073354967588));
#45208=CARTESIAN_POINT('Ctrl Pts',(18.2223177594351,17.8610717494634,60.5544438368303));
#45209=CARTESIAN_POINT('Ctrl Pts',(18.4506609156053,17.7272792212462,60.5253434722546));
#45210=CARTESIAN_POINT('Ctrl Pts',(18.7981164960626,17.5873420162312,60.5280059730316));
#45211=CARTESIAN_POINT('Ctrl Pts',(18.9336326795454,17.5470806517564,60.5393882955501));
#45212=CARTESIAN_POINT('Ctrl Pts',(19.1264136175084,17.5125581835725,60.5905739119415));
#45213=CARTESIAN_POINT('Ctrl Pts',(19.1864993721141,17.5052303115316,60.6119266927931));
#45214=CARTESIAN_POINT('Ctrl Pts',(19.267804466045,17.5006516995771,60.6505355994976));
#45215=CARTESIAN_POINT('Ctrl Pts',(19.2903823231718,17.5,60.6623776442419));
#45216=CARTESIAN_POINT('Ctrl Pts',(19.3125062814467,17.5,60.6751509175075));
#45217=CARTESIAN_POINT('',(-0.692506281446699,17.5,60.6751509175075));
#45218=CARTESIAN_POINT('Ctrl Pts',(-0.692506281446699,17.5,60.6751509175075));
#45219=CARTESIAN_POINT('Ctrl Pts',(-0.645361279705448,17.5,60.6479317380612));
#45220=CARTESIAN_POINT('Ctrl Pts',(-0.596388291682915,17.502946735144,60.6250879603399));
#45221=CARTESIAN_POINT('Ctrl Pts',(-0.463190632750145,17.5181479027027,
60.575463242537));
#45222=CARTESIAN_POINT('Ctrl Pts',(-0.378261798172194,17.5348232538744,
60.5559396365107));
#45223=CARTESIAN_POINT('Ctrl Pts',(-0.180907556972113,17.5875127881648,
60.5279468454333));
#45224=CARTESIAN_POINT('Ctrl Pts',(-0.0675380327356137,17.6285240662611,
60.5249434451136));
#45225=CARTESIAN_POINT('Ctrl Pts',(0.225797864641484,17.7623087481876,60.5333057280329));
#45226=CARTESIAN_POINT('Ctrl Pts',(0.414115616220393,17.879686489264,60.5574767880836));
#45227=CARTESIAN_POINT('Ctrl Pts',(0.72281200545154,18.1666272894371,60.6074243676588));
#45228=CARTESIAN_POINT('Ctrl Pts',(0.845420851299561,18.3256026756652,60.6321654725209));
#45229=CARTESIAN_POINT('Ctrl Pts',(0.992616457648736,18.6468724886464,60.6629219821082));
#45230=CARTESIAN_POINT('Ctrl Pts',(1.03092799962253,18.797169501223,60.6714910767922));
#45231=CARTESIAN_POINT('Ctrl Pts',(1.0380548355066,18.9686255097769,60.6730619112392));
#45232=CARTESIAN_POINT('Ctrl Pts',(1.03837982110709,18.984327656238,60.6731335892455));
#45233=CARTESIAN_POINT('Ctrl Pts',(1.03837982110709,19.,60.6731335892455));
#45234=CARTESIAN_POINT('Ctrl Pts',(-1.55969639024623,19.,62.1731335892455));
#45235=CARTESIAN_POINT('Ctrl Pts',(-1.55969639024623,18.9648000704089,62.1731335892455));
#45236=CARTESIAN_POINT('Ctrl Pts',(-1.55919017435171,18.9294832054733,62.1715330500334));
#45237=CARTESIAN_POINT('Ctrl Pts',(-1.55387954138258,18.7461724891625,62.1547834133932));
#45238=CARTESIAN_POINT('Ctrl Pts',(-1.54082544143153,18.6040823417911,62.1133623403687));
#45239=CARTESIAN_POINT('Ctrl Pts',(-1.49427132095936,18.3102983306063,61.9725888873933));
#45240=CARTESIAN_POINT('Ctrl Pts',(-1.45777563072466,18.1669858887455,61.8650054704346));
#45241=CARTESIAN_POINT('Ctrl Pts',(-1.3421359407357,17.8610717494634,61.5589283321452));
#45242=CARTESIAN_POINT('Ctrl Pts',(-1.25316601763253,17.7272792212462,61.3466271758336));
#45243=CARTESIAN_POINT('Ctrl Pts',(-1.0771324340934,17.5873420162312,61.0470530668595));
#45244=CARTESIAN_POINT('Ctrl Pts',(-0.999516961896896,17.5470806517564,
60.9353837705987));
#45245=CARTESIAN_POINT('Ctrl Pts',(-0.85879844881205,17.5125581835725,60.794023389153));
#45246=CARTESIAN_POINT('Ctrl Pts',(-0.81026352085034,17.5052303115316,60.7526639896847));
#45247=CARTESIAN_POINT('Ctrl Pts',(-0.736174679866266,17.5006516995771,
60.7015561662356));
#45248=CARTESIAN_POINT('Ctrl Pts',(-0.714630239721583,17.5,60.687924190773));
#45249=CARTESIAN_POINT('Ctrl Pts',(-0.6925062814467,17.5,60.6751509175075));
#45250=CARTESIAN_POINT('',(-10.6950125628934,17.5,78.));
#45251=CARTESIAN_POINT('Ctrl Pts',(-10.6950125628934,17.5,78.));
#45252=CARTESIAN_POINT('Ctrl Pts',(-10.6950125628934,17.5,77.8952609229081));
#45253=CARTESIAN_POINT('Ctrl Pts',(-10.6774013907771,17.5108310402064,77.7928573971986));
#45254=CARTESIAN_POINT('Ctrl Pts',(-10.606922072288,17.5583420169659,77.5660868004609));
#45255=CARTESIAN_POINT('Ctrl Pts',(-10.5473418462476,17.6007431024612,77.4457801289306));
#45256=CARTESIAN_POINT('Ctrl Pts',(-10.3820601635002,17.7393206831896,77.1652385309203));
#45257=CARTESIAN_POINT('Ctrl Pts',(-10.2569173400549,17.8614426921811,76.9993505489696));
#45258=CARTESIAN_POINT('Ctrl Pts',(-10.0501915527651,18.1597175199196,76.7453916755355));
#45259=CARTESIAN_POINT('Ctrl Pts',(-9.96671053437231,18.3173213761021,76.6505086914015));
#45260=CARTESIAN_POINT('Ctrl Pts',(-9.86531576337833,18.637591898099,76.5370376074287));
#45261=CARTESIAN_POINT('Ctrl Pts',(-9.83760998123497,18.7870280562669,76.5068853291583));
#45262=CARTESIAN_POINT('Ctrl Pts',(-9.83163226537581,18.9628275273603,76.5003452600286));
#45263=CARTESIAN_POINT('Ctrl Pts',(-9.83131656913913,18.9814183151258,76.5));
#45264=CARTESIAN_POINT('Ctrl Pts',(-9.83131656913913,19.,76.5));
#45265=CARTESIAN_POINT('Ctrl Pts',(-9.83131656913913,19.,79.5));
#45266=CARTESIAN_POINT('Ctrl Pts',(-9.83131656913913,18.9077230153478,79.5));
#45267=CARTESIAN_POINT('Ctrl Pts',(-9.83911472501011,18.8150583449374,79.4914997277812));
#45268=CARTESIAN_POINT('Ctrl Pts',(-9.87936798630065,18.5791911526486,79.4471799061994));
#45269=CARTESIAN_POINT('Ctrl Pts',(-9.92232403253812,18.4425366457864,79.3997588766925));
#45270=CARTESIAN_POINT('Ctrl Pts',(-10.0468807891092,18.1638733921006,79.257078036649));
#45271=CARTESIAN_POINT('Ctrl Pts',(-10.1339057616696,18.0287684620774,79.1549908365387));
#45272=CARTESIAN_POINT('Ctrl Pts',(-10.3514335308102,17.7609964409145,78.8743354225477));
#45273=CARTESIAN_POINT('Ctrl Pts',(-10.4832005944038,17.650192730897,78.6864655686667));
#45274=CARTESIAN_POINT('Ctrl Pts',(-10.6338951387459,17.5385627946702,78.3634796463819));
#45275=CARTESIAN_POINT('Ctrl Pts',(-10.6729371667049,17.5140590169286,78.2399649670483));
#45276=CARTESIAN_POINT('Ctrl Pts',(-10.692640786038,17.5014920111156,78.0771284470038));
#45277=CARTESIAN_POINT('Ctrl Pts',(-10.6950125628934,17.5,78.0386867639672));
#45278=CARTESIAN_POINT('Ctrl Pts',(-10.6950125628934,17.5,78.));
#45279=CARTESIAN_POINT('',(-0.69250628144669,17.5,95.3248490824925));
#45280=CARTESIAN_POINT('Ctrl Pts',(-0.692506281446693,17.5,95.3248490824925));
#45281=CARTESIAN_POINT('Ctrl Pts',(-0.739651283187984,17.5,95.2976299030462));
#45282=CARTESIAN_POINT('Ctrl Pts',(-0.783921069024338,17.502946735144,95.2666399401801));
#45283=CARTESIAN_POINT('Ctrl Pts',(-0.893496164763615,17.5181479027027,
95.1760997427212));
#45284=CARTESIAN_POINT('Ctrl Pts',(-0.952868520844795,17.5348232538744,
95.1123110174761));
#45285=CARTESIAN_POINT('Ctrl Pts',(-1.0757881096407,17.5875127881648,94.9553936265909));
#45286=CARTESIAN_POINT('Ctrl Pts',(-1.1350738927336,17.6285240662611,94.858714438747));
#45287=CARTESIAN_POINT('Ctrl Pts',(-1.27449989198037,17.7623087481876,94.6004969583169));
#45288=CARTESIAN_POINT('Ctrl Pts',(-1.34772601572953,17.879686489264,94.4253234714407));
#45289=CARTESIAN_POINT('Ctrl Pts',(-1.45881833757545,18.166627289437,94.1330107665224));
#45290=CARTESIAN_POINT('Ctrl Pts',(-1.49869633517117,18.3256026756651,94.0144578388582));
#45291=CARTESIAN_POINT('Ctrl Pts',(-1.54565821971146,18.6468724886464,93.8716044496407));
#45292=CARTESIAN_POINT('Ctrl Pts',(-1.55739293701455,18.797169501223,93.8341411336913));
#45293=CARTESIAN_POINT('Ctrl Pts',(-1.55959597242036,18.9686255097769,93.8271836955436));
#45294=CARTESIAN_POINT('Ctrl Pts',(-1.55969639024622,18.984327656238,93.8268664107545));
#45295=CARTESIAN_POINT('Ctrl Pts',(-1.55969639024622,19.,93.8268664107545));
#45296=CARTESIAN_POINT('Ctrl Pts',(1.0383798211071,19.,95.3268664107545));
#45297=CARTESIAN_POINT('Ctrl Pts',(1.0383798211071,18.9648000704089,95.3268664107545));
#45298=CARTESIAN_POINT('Ctrl Pts',(1.03674060554243,18.9294832054732,95.327228284536));
#45299=CARTESIAN_POINT('Ctrl Pts',(1.01957967822326,18.7461724891624,95.3310039597947));
#45300=CARTESIAN_POINT('Ctrl Pts',(0.977180926756438,18.604082341791,95.3404093141259));
#45301=CARTESIAN_POINT('Ctrl Pts',(0.831990480065218,18.3102983306063,95.3704789896338));
#45302=CARTESIAN_POINT('Ctrl Pts',(0.720572662835746,18.1669858887455,95.3926645032412));
#45303=CARTESIAN_POINT('Ctrl Pts',(0.39768224056495,17.8610717494634,95.4455561631698));
#45304=CARTESIAN_POINT('Ctrl Pts',(0.169339084394697,17.7272792212462,95.4746565277455));
#45305=CARTESIAN_POINT('Ctrl Pts',(-0.178116496062518,17.5873420162312,
95.4719940269684));
#45306=CARTESIAN_POINT('Ctrl Pts',(-0.313632679545349,17.5470806517564,
95.4606117044499));
#45307=CARTESIAN_POINT('Ctrl Pts',(-0.506413617508378,17.5125581835725,
95.4094260880585));
#45308=CARTESIAN_POINT('Ctrl Pts',(-0.566499372114017,17.5052303115316,
95.388073307207));
#45309=CARTESIAN_POINT('Ctrl Pts',(-0.647804466045143,17.5006516995771,
95.3494644005024));
#45310=CARTESIAN_POINT('Ctrl Pts',(-0.670382323171821,17.5,95.3376223557581));
#45311=CARTESIAN_POINT('Ctrl Pts',(-0.692506281446687,17.5,95.3248490824925));
#45312=CARTESIAN_POINT('Origin',(16.36,19.,65.7890418066394));
#45313=CARTESIAN_POINT('',(15.0609618943234,19.,65.0390418066394));
#45314=CARTESIAN_POINT('Origin',(2.25999999999999,19.,65.7890418066394));
#45315=CARTESIAN_POINT('',(0.960961894323336,19.,66.5390418066394));
#45316=CARTESIAN_POINT('Origin',(-4.79,19.,78.));
#45317=CARTESIAN_POINT('',(-4.79,19.,79.5));
#45318=CARTESIAN_POINT('Origin',(2.26,19.,90.2109581933606));
#45319=CARTESIAN_POINT('',(3.55903810567666,19.,90.9609581933606));
#45320=CARTESIAN_POINT('Origin',(16.36,19.,90.2109581933606));
#45321=CARTESIAN_POINT('',(17.6590381056767,19.,89.4609581933606));
#45322=CARTESIAN_POINT('Origin',(23.41,19.,78.));
#45323=CARTESIAN_POINT('',(23.41,19.,76.5));
#45324=CARTESIAN_POINT('Origin',(9.31,23.45,78.));
#45325=CARTESIAN_POINT('',(6.2075,23.5,78.));
#45326=CARTESIAN_POINT('',(6.2575,23.45,78.));
#45327=CARTESIAN_POINT('Origin',(9.31,23.5,78.));
#45328=CARTESIAN_POINT('Origin',(16.61,23.5,78.));
#45329=CARTESIAN_POINT('',(2.01,23.5,78.));
#45330=CARTESIAN_POINT('Origin',(9.31,23.5,78.));
#45331=CARTESIAN_POINT('Origin',(9.31,23.4,78.));
#45332=CARTESIAN_POINT('',(1.91,23.4,78.));
#45333=CARTESIAN_POINT('Origin',(9.31,14.15,78.));
#45334=CARTESIAN_POINT('',(2.01,14.05,78.));
#45335=CARTESIAN_POINT('Origin',(9.31,14.05,78.));
#45336=CARTESIAN_POINT('',(1.91,14.15,78.));
#45337=CARTESIAN_POINT('Origin',(12.4125,14.05,78.));
#45338=CARTESIAN_POINT('',(6.2075,14.05,78.));
#45339=CARTESIAN_POINT('Origin',(9.31,14.05,78.));
#45340=CARTESIAN_POINT('Origin',(9.31,14.1,78.));
#45341=CARTESIAN_POINT('',(6.2575,14.1,78.));
#45342=CARTESIAN_POINT('',(0.,0.,0.));
#45343=CARTESIAN_POINT('Origin',(0.,0.,-0.915));
#45344=CARTESIAN_POINT('',(-0.989508121607439,2.46417016753209E-5,-1.67997427199779));
#45345=CARTESIAN_POINT('',(-0.989512555708751,1.62595781710845E-5,-1.71597572800221));
#45346=CARTESIAN_POINT('',(-0.989525,-1.21181862392628E-16,-0.915));
#45347=CARTESIAN_POINT('',(0.432569264169048,0.889983862027826,-1.760475));
#45348=CARTESIAN_POINT('Ctrl Pts',(-0.989508121607439,2.46417016753209E-5,
-1.67997427199779));
#45349=CARTESIAN_POINT('Ctrl Pts',(-0.989549791832843,0.0432915798739707,
-1.68171398035312));
#45350=CARTESIAN_POINT('Ctrl Pts',(-0.986763738908389,0.0865531766282412,
-1.68345368870845));
#45351=CARTESIAN_POINT('Ctrl Pts',(-0.981106280255709,0.129435929606698,
-1.68519339706378));
#45352=CARTESIAN_POINT('Ctrl Pts',(-0.959748207461145,0.291327163104516,
-1.69176115477542));
#45353=CARTESIAN_POINT('Ctrl Pts',(-0.897466338773216,0.447819046310428,
-1.69832891248706));
#45354=CARTESIAN_POINT('Ctrl Pts',(-0.801742294532236,0.580113943815296,
-1.7048966701987));
#45355=CARTESIAN_POINT('Ctrl Pts',(-0.706018250291256,0.712408841320163,
-1.71146442791034));
#45356=CARTESIAN_POINT('Ctrl Pts',(-0.576852030497224,0.820506753123986,
-1.71803218562198));
#45357=CARTESIAN_POINT('Ctrl Pts',(-0.429759709431166,0.891420527045617,
-1.72459994333363));
#45358=CARTESIAN_POINT('Ctrl Pts',(-0.282667388365107,0.962334300967249,
-1.73116770104527));
#45359=CARTESIAN_POINT('Ctrl Pts',(-0.117648966027021,0.99606393700669,
-1.73773545875691));
#45360=CARTESIAN_POINT('Ctrl Pts',(0.0454726780246543,0.988561401513198,
-1.74430321646855));
#45361=CARTESIAN_POINT('Ctrl Pts',(0.179357434066637,0.982403572856662,
-1.74969381097903));
#45362=CARTESIAN_POINT('Ctrl Pts',(0.311964411384094,0.948469386821795,
-1.75508440548952));
#45363=CARTESIAN_POINT('Ctrl Pts',(0.4325852656532,0.88999165664392,-1.760475));
#45364=CARTESIAN_POINT('',(-0.4325532626849,0.88997606741173,-1.760475));
#45365=CARTESIAN_POINT('Origin',(0.,0.,-1.760475));
#45366=CARTESIAN_POINT('Ctrl Pts',(-0.4325532626849,0.88997606741173,-1.760475));
#45367=CARTESIAN_POINT('Ctrl Pts',(-0.579457834201592,0.818576336520455,
-1.75390724228836));
#45368=CARTESIAN_POINT('Ctrl Pts',(-0.708275027509353,0.710144989051779,
-1.74733948457672));
#45369=CARTESIAN_POINT('Ctrl Pts',(-0.803577819756788,0.577570371582787,
-1.74077172686507));
#45370=CARTESIAN_POINT('Ctrl Pts',(-0.898880612004223,0.444995754113794,
-1.73420396915343));
#45371=CARTESIAN_POINT('Ctrl Pts',(-0.960669003191333,0.288277866644485,
-1.72763621144179));
#45372=CARTESIAN_POINT('Ctrl Pts',(-0.981513623068095,0.126312099804374,
-1.72106845373015));
#45373=CARTESIAN_POINT('Ctrl Pts',(-0.986901353888686,0.0844486377194643,
-1.7193708784875));
#45374=CARTESIAN_POINT('Ctrl Pts',(-0.989553742529366,0.0422345790642187,
-1.71767330324486));
#45375=CARTESIAN_POINT('Ctrl Pts',(-0.989512555708751,1.62595781710845E-5,
-1.71597572800221));
#45376=CARTESIAN_POINT('Origin',(0.,0.,-0.915));
#45377=CARTESIAN_POINT('',(-0.989602407284016,-7.73947795529306E-6,-1.42997427199779));
#45378=CARTESIAN_POINT('',(-0.989600974548901,-8.74702472718336E-6,-1.46597572800221));
#45379=CARTESIAN_POINT('',(-0.989525,-1.21181862392628E-16,-0.915));
#45380=CARTESIAN_POINT('Ctrl Pts',(-0.989602407284016,-7.73947795529306E-6,
-1.42997427199779));
#45381=CARTESIAN_POINT('Ctrl Pts',(-0.989536830744615,0.155635723124492,
-1.43623422114676));
#45382=CARTESIAN_POINT('Ctrl Pts',(-0.952173126552117,0.311309569170158,
-1.44249417029572));
#45383=CARTESIAN_POINT('Ctrl Pts',(-0.881409540624574,0.449933753797064,
-1.44875411944469));
#45384=CARTESIAN_POINT('Ctrl Pts',(-0.807166431596158,0.595374241561052,
-1.45532187715633));
#45385=CARTESIAN_POINT('Ctrl Pts',(-0.696158069103402,0.722047144202599,
-1.46188963486797));
#45386=CARTESIAN_POINT('Ctrl Pts',(-0.561719334295483,0.814735877727747,
-1.46845739257961));
#45387=CARTESIAN_POINT('Ctrl Pts',(-0.427280599487563,0.907424611252896,
-1.47502515029125));
#45388=CARTESIAN_POINT('Ctrl Pts',(-0.26941149236448,0.966129175661646,
-1.48159290800289));
#45389=CARTESIAN_POINT('Ctrl Pts',(-0.107076041692171,0.983797683784885,
-1.48816066571454));
#45390=CARTESIAN_POINT('Ctrl Pts',(0.0552594089801381,1.00146619190812,
-1.49472842342618));
#45391=CARTESIAN_POINT('Ctrl Pts',(0.222061203201673,0.978098643745851,
-1.50129618113782));
#45392=CARTESIAN_POINT('Ctrl Pts',(0.373292273023635,0.916502067392168,
-1.50786393884946));
#45393=CARTESIAN_POINT('Ctrl Pts',(0.524523342845598,0.854905491038486,
-1.5144316965611));
#45394=CARTESIAN_POINT('Ctrl Pts',(0.660183688267988,0.755079886493395,
-1.52099945427274));
#45395=CARTESIAN_POINT('Ctrl Pts',(0.763977108360576,0.629016803897046,
-1.52756721198439));
#45396=CARTESIAN_POINT('Ctrl Pts',(0.867770528453163,0.502953721300697,
-1.53413496969603));
#45397=CARTESIAN_POINT('Ctrl Pts',(0.939697023215948,0.350653160653091,
-1.54070272740767));
#45398=CARTESIAN_POINT('Ctrl Pts',(0.971116421385275,0.190410233050476,
-1.54727048511931));
#45399=CARTESIAN_POINT('Ctrl Pts',(1.0025358195546,0.0301673054478622,-1.55383824283095));
#45400=CARTESIAN_POINT('Ctrl Pts',(0.99344812113047,-0.13801798910976,-1.56040600054259));
#45401=CARTESIAN_POINT('Ctrl Pts',(0.944944986100939,-0.29394239770406,
-1.56697375825423));
#45402=CARTESIAN_POINT('Ctrl Pts',(0.896441851071408,-0.44986680629836,
-1.57354151596587));
#45403=CARTESIAN_POINT('Ctrl Pts',(0.808523279436478,-0.593530328929339,
-1.58010927367752));
#45404=CARTESIAN_POINT('Ctrl Pts',(0.691750490716862,-0.707675366998289,
-1.58667703138916));
#45405=CARTESIAN_POINT('Ctrl Pts',(0.574977701997246,-0.821820405067239,
-1.5932447891008));
#45406=CARTESIAN_POINT('Ctrl Pts',(0.429350696192944,-0.906446958574161,
-1.59981254681244));
#45407=CARTESIAN_POINT('Ctrl Pts',(0.272362919805735,-0.951389292968879,
-1.60638030452408));
#45408=CARTESIAN_POINT('Ctrl Pts',(0.115375143418526,-0.996331627363596,
-1.61294806223572));
#45409=CARTESIAN_POINT('Ctrl Pts',(-0.0529734035515899,-1.00158974264611,
-1.61951581994736));
#45410=CARTESIAN_POINT('Ctrl Pts',(-0.212459850119537,-0.966531945468779,
-1.62608357765901));
#45411=CARTESIAN_POINT('Ctrl Pts',(-0.371946296687484,-0.93147414829145,
-1.63265133537065));
#45412=CARTESIAN_POINT('Ctrl Pts',(-0.522570642853263,-0.856100438654279,
-1.63921909308229));
#45413=CARTESIAN_POINT('Ctrl Pts',(-0.646239135575092,-0.749465207577936,
-1.64578685079393));
#45414=CARTESIAN_POINT('Ctrl Pts',(-0.76990762829692,-0.642829976501594,
-1.65235460850557));
#45415=CARTESIAN_POINT('Ctrl Pts',(-0.866620267574799,-0.504933223986081,
-1.65892236621721));
#45416=CARTESIAN_POINT('Ctrl Pts',(-0.924759448763137,-0.352339555833462,
-1.66549012392885));
#45417=CARTESIAN_POINT('Ctrl Pts',(-0.967498363418187,-0.240165843944588,
-1.67031817328517));
#45418=CARTESIAN_POINT('Ctrl Pts',(-0.989392478140921,-0.120050031936858,
-1.67514622264148));
#45419=CARTESIAN_POINT('Ctrl Pts',(-0.989508121607439,2.46417016753209E-5,
-1.67997427199779));
#45420=CARTESIAN_POINT('Ctrl Pts',(-0.989512555708751,1.62595781710845E-5,
-1.71597572800221));
#45421=CARTESIAN_POINT('Ctrl Pts',(-0.989394394624236,-0.121104097426263,
-1.71110554553322));
#45422=CARTESIAN_POINT('Ctrl Pts',(-0.96710644517705,-0.24225952369773,
-1.70623536306422));
#45423=CARTESIAN_POINT('Ctrl Pts',(-0.923634939065364,-0.355272041749406,
-1.70136518059523));
#45424=CARTESIAN_POINT('Ctrl Pts',(-0.865010786619457,-0.507676770252159,
-1.69479742288359));
#45425=CARTESIAN_POINT('Ctrl Pts',(-0.767861633161228,-0.64527258104675,
-1.68822966517194));
#45426=CARTESIAN_POINT('Ctrl Pts',(-0.643855273201409,-0.751516138272709,
-1.6816619074603));
#45427=CARTESIAN_POINT('Ctrl Pts',(-0.519848913241591,-0.857759695498667,
-1.67509414974866));
#45428=CARTESIAN_POINT('Ctrl Pts',(-0.368985346780182,-0.932650999155991,
-1.66852639203702));
#45429=CARTESIAN_POINT('Ctrl Pts',(-0.209388203118329,-0.967201097307302,
-1.66195863432538));
#45430=CARTESIAN_POINT('Ctrl Pts',(-0.0497910594564758,-1.00175119545861,
-1.65539087661374));
#45431=CARTESIAN_POINT('Ctrl Pts',(0.118539661405822,-0.995960088103908,
-1.6488231189021));
#45432=CARTESIAN_POINT('Ctrl Pts',(0.27538380659921,-0.950519709731925,
-1.64225536119046));
#45433=CARTESIAN_POINT('Ctrl Pts',(0.432227951792598,-0.905079331359941,
-1.63568760347881));
#45434=CARTESIAN_POINT('Ctrl Pts',(0.577585521317075,-0.819989681970679,
-1.62911984576717));
#45435=CARTESIAN_POINT('Ctrl Pts',(0.693995143032626,-0.705474038967786,
-1.62255208805553));
#45436=CARTESIAN_POINT('Ctrl Pts',(0.810404764748177,-0.590958395964892,
-1.61598433034389));
#45437=CARTESIAN_POINT('Ctrl Pts',(0.897866438654801,-0.447016759348368,
-1.60941657263225));
#45438=CARTESIAN_POINT('Ctrl Pts',(0.945873977571743,-0.290939168622987,
-1.60284881492061));
#45439=CARTESIAN_POINT('Ctrl Pts',(0.993881516488684,-0.134861577897606,
-1.59628105720897));
#45440=CARTESIAN_POINT('Ctrl Pts',(1.00243492041594,0.0333519669366303,
-1.58971329949732));
#45441=CARTESIAN_POINT('Ctrl Pts',(0.970506636916252,0.193494330149772,
-1.58314554178568));
#45442=CARTESIAN_POINT('Ctrl Pts',(0.938578353416562,0.353636693362912,
-1.57657778407404));
#45443=CARTESIAN_POINT('Ctrl Pts',(0.866168382489923,0.505707874954959,
-1.5700100263624));
#45444=CARTESIAN_POINT('Ctrl Pts',(0.761975010695729,0.631440565385368,
-1.56344226865076));
#45445=CARTESIAN_POINT('Ctrl Pts',(0.657781638901535,0.757173255815777,
-1.55687451093912));
#45446=CARTESIAN_POINT('Ctrl Pts',(0.521804866239785,0.856567455084549,
-1.55030675322748));
#45447=CARTESIAN_POINT('Ctrl Pts',(0.370378885396273,0.917683310519167,
-1.54373899551583));
#45448=CARTESIAN_POINT('Ctrl Pts',(0.218952904552762,0.978799165953784,
-1.53717123780419));
#45449=CARTESIAN_POINT('Ctrl Pts',(0.0520777155274912,1.00163667755425,
-1.53060348009255));
#45450=CARTESIAN_POINT('Ctrl Pts',(-0.110200787535187,0.983452551133096,
-1.52403572238091));
#45451=CARTESIAN_POINT('Ctrl Pts',(-0.272479290597865,0.965268424711947,
-1.51746796466927));
#45452=CARTESIAN_POINT('Ctrl Pts',(-0.430161107697951,0.906062660269186,
-1.51090020695763));
#45453=CARTESIAN_POINT('Ctrl Pts',(-0.564304713162749,0.812947319648577,
-1.50433244924599));
#45454=CARTESIAN_POINT('Ctrl Pts',(-0.698448318627548,0.719831979027969,
-1.49776469153435));
#45455=CARTESIAN_POINT('Ctrl Pts',(-0.809053712457058,0.592807062229512,
-1.4911969338227));
#45456=CARTESIAN_POINT('Ctrl Pts',(-0.88283441765268,0.447131455127287,
-1.48462917611106));
#45457=CARTESIAN_POINT('Ctrl Pts',(-0.952683957187391,0.309217700432873,
-1.47841136007478));
#45458=CARTESIAN_POINT('Ctrl Pts',(-0.989528433074503,0.154587790262781,
-1.47219354403849));
#45459=CARTESIAN_POINT('Ctrl Pts',(-0.989600974548901,-8.74702472718336E-6,
-1.46597572800221));
#45460=CARTESIAN_POINT('Origin',(0.,0.,-0.915));
#45461=CARTESIAN_POINT('',(-0.989468413969488,-1.8577996640623E-5,-1.17997427199779));
#45462=CARTESIAN_POINT('',(-0.989466234208983,-1.79285505235583E-5,-1.21597572800221));
#45463=CARTESIAN_POINT('',(-0.989525,-1.21181862392628E-16,-0.915));
#45464=CARTESIAN_POINT('Ctrl Pts',(-0.989468413969488,-1.8577996640623E-5,
-1.17997427199779));
#45465=CARTESIAN_POINT('Ctrl Pts',(-0.989396562633886,0.104757608424716,
-1.18418670422875));
#45466=CARTESIAN_POINT('Ctrl Pts',(-0.972819916344485,0.209555998775421,
-1.18839913645971));
#45467=CARTESIAN_POINT('Ctrl Pts',(-0.940111910177114,0.309051383145319,
-1.19261156869068));
#45468=CARTESIAN_POINT('Ctrl Pts',(-0.889115657190716,0.464178288965946,
-1.19917932640232));
#45469=CARTESIAN_POINT('Ctrl Pts',(-0.798905564248481,0.606414079010267,
-1.20574708411396));
#45470=CARTESIAN_POINT('Ctrl Pts',(-0.680318120066929,0.718672676946543,
-1.2123148418256));
#45471=CARTESIAN_POINT('Ctrl Pts',(-0.561730675885377,0.830931274882821,
-1.21888259953724));
#45472=CARTESIAN_POINT('Ctrl Pts',(-0.414765880464508,0.913212680711054,
-1.22545035724888));
#45473=CARTESIAN_POINT('Ctrl Pts',(-0.257077881975125,0.955632839368786,
-1.23201811496052));
#45474=CARTESIAN_POINT('Ctrl Pts',(-0.0993898834857447,0.998052998026518,
-1.23858587267216));
#45475=CARTESIAN_POINT('Ctrl Pts',(0.0690213180721501,1.00061190951375,
-1.24515363038381));
#45476=CARTESIAN_POINT('Ctrl Pts',(0.227925324681052,0.963002184551002,
-1.25172138809545));
#45477=CARTESIAN_POINT('Ctrl Pts',(0.386829331289954,0.925392459588256,
-1.25828914580709));
#45478=CARTESIAN_POINT('Ctrl Pts',(0.536226142949864,0.847614098175531,
-1.26485690351873));
#45479=CARTESIAN_POINT('Ctrl Pts',(0.658169465504165,0.73901022710025,-1.27142466123037));
#45480=CARTESIAN_POINT('Ctrl Pts',(0.780112788058465,0.630406356024968,
-1.27799241894201));
#45481=CARTESIAN_POINT('Ctrl Pts',(0.874602621507156,0.490976975287128,
-1.28456017665365));
#45482=CARTESIAN_POINT('Ctrl Pts',(0.930288373243623,0.337471041259424,
-1.2911279343653));
#45483=CARTESIAN_POINT('Ctrl Pts',(0.98597412498009,0.18396510723172,-1.29769569207694));
#45484=CARTESIAN_POINT('Ctrl Pts',(1.00285579500433,0.0163826199141512,
-1.30426344978858));
#45485=CARTESIAN_POINT('Ctrl Pts',(0.978905472461058,-0.145145571984733,
-1.31083120750022));
#45486=CARTESIAN_POINT('Ctrl Pts',(0.954955149917781,-0.306673763883617,
-1.31739896521186));
#45487=CARTESIAN_POINT('Ctrl Pts',(0.890172834806985,-0.462147660363816,
-1.3239667229235));
#45488=CARTESIAN_POINT('Ctrl Pts',(0.79234050366626,-0.592890957369197,
-1.33053448063514));
#45489=CARTESIAN_POINT('Ctrl Pts',(0.694508172525535,-0.723634254374579,
-1.33710223834679));
#45490=CARTESIAN_POINT('Ctrl Pts',(0.563625825354881,-0.829646951905141,
-1.34366999605843));
#45491=CARTESIAN_POINT('Ctrl Pts',(0.415415705996909,-0.898194273135755,
-1.35023775377007));
#45492=CARTESIAN_POINT('Ctrl Pts',(0.267205586638937,-0.966741594366368,
-1.35680551148171));
#45493=CARTESIAN_POINT('Ctrl Pts',(0.101667695093648,-0.997823539297033,
-1.36337326919335));
#45494=CARTESIAN_POINT('Ctrl Pts',(-0.0613127270280904,-0.98770638885309,
-1.36994102690499));
#45495=CARTESIAN_POINT('Ctrl Pts',(-0.224293149149829,-0.977589238409147,
-1.37650878461663));
#45496=CARTESIAN_POINT('Ctrl Pts',(-0.384716101848015,-0.926272992590596,
-1.38307654232827));
#45497=CARTESIAN_POINT('Ctrl Pts',(-0.523310775614874,-0.839922016149752,
-1.38964430003991));
#45498=CARTESIAN_POINT('Ctrl Pts',(-0.661905449381735,-0.753571039708906,
-1.39621205775156));
#45499=CARTESIAN_POINT('Ctrl Pts',(-0.778671844217267,-0.632185332645765,
-1.4027798154632));
#45500=CARTESIAN_POINT('Ctrl Pts',(-0.859583395256424,-0.490346354807054,
-1.40934757317484));
#45501=CARTESIAN_POINT('Ctrl Pts',(-0.940494946295581,-0.348507376968345,
-1.41591533088648));
#45502=CARTESIAN_POINT('Ctrl Pts',(-0.985551653538363,-0.186215128354065,
-1.42248308859812));
#45503=CARTESIAN_POINT('Ctrl Pts',(-0.989341079377716,-0.0229649676037106,
-1.42905084630976));
#45504=CARTESIAN_POINT('Ctrl Pts',(-0.989518676934171,-0.0153139854050142,
-1.42935865487244));
#45505=CARTESIAN_POINT('Ctrl Pts',(-0.989605631754353,-0.00766089917197932,
-1.42966646343512));
#45506=CARTESIAN_POINT('Ctrl Pts',(-0.989602407284016,-7.73947795529306E-6,
-1.42997427199779));
#45507=CARTESIAN_POINT('Ctrl Pts',(-0.989600974548901,-8.74702472718336E-6,
-1.46597572800221));
#45508=CARTESIAN_POINT('Ctrl Pts',(-0.989605057217949,-0.00870951445610583,
-1.46562578632685));
#45509=CARTESIAN_POINT('Ctrl Pts',(-0.989492665060294,-0.017410176179129,
-1.4652758446515));
#45510=CARTESIAN_POINT('Ctrl Pts',(-0.989263126563413,-0.026107746288861,
-1.46492590297614));
#45511=CARTESIAN_POINT('Ctrl Pts',(-0.984955113716792,-0.18934504319679,
-1.4583581452645));
#45512=CARTESIAN_POINT('Ctrl Pts',(-0.939383071461817,-0.351493339606654,
-1.45179038755286));
#45513=CARTESIAN_POINT('Ctrl Pts',(-0.858021341400782,-0.493074565003882,
-1.44522262984121));
#45514=CARTESIAN_POINT('Ctrl Pts',(-0.776659611339746,-0.634655790401111,
-1.43865487212957));
#45515=CARTESIAN_POINT('Ctrl Pts',(-0.659508193472649,-0.755669944785702,
-1.43208711441793));
#45516=CARTESIAN_POINT('Ctrl Pts',(-0.520639903880605,-0.841580203173077,
-1.42551935670629));
#45517=CARTESIAN_POINT('Ctrl Pts',(-0.38177161428856,-0.927490461560451,
-1.41895159899465));
#45518=CARTESIAN_POINT('Ctrl Pts',(-0.221186452971569,-0.97829682395061,
-1.41238384128301));
#45519=CARTESIAN_POINT('Ctrl Pts',(-0.0581747145888518,-0.987896174287954,
-1.40581608357137));
#45520=CARTESIAN_POINT('Ctrl Pts',(0.104837023793865,-0.997495524625299,
-1.39924832585972));
#45521=CARTESIAN_POINT('Ctrl Pts',(0.270275339242308,-0.96588786290983,
-1.39268056814808));
#45522=CARTESIAN_POINT('Ctrl Pts',(0.418266951644149,-0.896870060487294,
-1.38611281043644));
#45523=CARTESIAN_POINT('Ctrl Pts',(0.566258564045989,-0.827852258064758,
-1.3795450527248));
#45524=CARTESIAN_POINT('Ctrl Pts',(0.696803473401228,-0.721424314935155,
-1.37297729501316));
#45525=CARTESIAN_POINT('Ctrl Pts',(0.794219970630926,-0.590370889036802,
-1.36640953730152));
#45526=CARTESIAN_POINT('Ctrl Pts',(0.891636467860624,-0.45931746313845,
-1.35984177958988));
#45527=CARTESIAN_POINT('Ctrl Pts',(0.955924552964781,-0.303638554471347,
-1.35327402187823));
#45528=CARTESIAN_POINT('Ctrl Pts',(0.979361618771641,-0.142035094320265,
-1.34670626416659));
#45529=CARTESIAN_POINT('Ctrl Pts',(1.0027986845785,0.0195683658308168,-1.34013850645495));
#45530=CARTESIAN_POINT('Ctrl Pts',(0.985384731088064,0.18709637746588,-1.33357074874331));
#45531=CARTESIAN_POINT('Ctrl Pts',(0.929211609725224,0.340424635837656,
-1.32700299103167));
#45532=CARTESIAN_POINT('Ctrl Pts',(0.873038488362384,0.493752894209432,
-1.32043523332003));
#45533=CARTESIAN_POINT('Ctrl Pts',(0.778106199127141,0.632881399317924,
-1.31386747560839));
#45534=CARTESIAN_POINT('Ctrl Pts',(0.655818484628525,0.741097337444794,
-1.30729971789675));
#45535=CARTESIAN_POINT('Ctrl Pts',(0.533530770129908,0.849313275571664,
-1.3007319601851));
#45536=CARTESIAN_POINT('Ctrl Pts',(0.383887630367918,0.926616646716914,
-1.29416420247346));
#45537=CARTESIAN_POINT('Ctrl Pts',(0.224864949668683,0.963721382323536,
-1.28759644476182));
#45538=CARTESIAN_POINT('Ctrl Pts',(0.065842268969448,1.00082611793016,-1.28102868705018));
#45539=CARTESIAN_POINT('Ctrl Pts',(-0.102559952667031,0.997732217998152,
-1.27446092933854));
#45540=CARTESIAN_POINT('Ctrl Pts',(-0.260112395937802,0.954811337292705,
-1.2678931716269));
#45541=CARTESIAN_POINT('Ctrl Pts',(-0.417664839208572,0.911890456587258,
-1.26132541391526));
#45542=CARTESIAN_POINT('Ctrl Pts',(-0.564367504113633,0.829142595108368,
-1.25475765620361));
#45543=CARTESIAN_POINT('Ctrl Pts',(-0.682597730913487,0.716507840914783,
-1.24818989849197));
#45544=CARTESIAN_POINT('Ctrl Pts',(-0.80082795771334,0.603873086721197,
-1.24162214078033));
#45545=CARTESIAN_POINT('Ctrl Pts',(-0.890585746407986,0.461351439812916,
-1.23505438306869));
#45546=CARTESIAN_POINT('Ctrl Pts',(-0.941088941335523,0.306063315079296,
-1.22848662535705));
#45547=CARTESIAN_POINT('Ctrl Pts',(-0.973156724363405,0.207460723740084,
-1.22431632623877));
#45548=CARTESIAN_POINT('Ctrl Pts',(-0.98939779705991,0.103710929816322,
-1.22014602712049));
#45549=CARTESIAN_POINT('Ctrl Pts',(-0.989466234208983,-1.79285505235583E-5,
-1.21597572800221));
#45550=CARTESIAN_POINT('Origin',(0.,0.,-0.915));
#45551=CARTESIAN_POINT('',(-0.989479227929023,2.11592729404686E-5,-0.929974271997791));
#45552=CARTESIAN_POINT('',(-0.989481817826863,2.16465008535149E-5,-0.965975728002209));
#45553=CARTESIAN_POINT('',(-0.989525,-1.21181862392628E-16,-0.915));
#45554=CARTESIAN_POINT('Ctrl Pts',(-0.989479227929023,2.11592729404686E-5,
-0.929974271997791));
#45555=CARTESIAN_POINT('Ctrl Pts',(-0.989521950655237,0.0538675948649017,
-0.932139187310748));
#45556=CARTESIAN_POINT('Ctrl Pts',(-0.985200273850893,0.107707242346304,
-0.934304102623705));
#45557=CARTESIAN_POINT('Ctrl Pts',(-0.976453133180159,0.160818033141656,
-0.936469017936662));
#45558=CARTESIAN_POINT('Ctrl Pts',(-0.949916713833314,0.321941567041523,
-0.943036775648303));
#45559=CARTESIAN_POINT('Ctrl Pts',(-0.882650593613209,0.476357077624845,
-0.949604533359944));
#45560=CARTESIAN_POINT('Ctrl Pts',(-0.782735116182012,0.605515399454408,
-0.956172291071585));
#45561=CARTESIAN_POINT('Ctrl Pts',(-0.682819638750815,0.734673721283971,
-0.962740048783226));
#45562=CARTESIAN_POINT('Ctrl Pts',(-0.550254804108526,0.838574854359776,
-0.969307806494868));
#45563=CARTESIAN_POINT('Ctrl Pts',(-0.400964964929612,0.904737673571679,
-0.97587556420651));
#45564=CARTESIAN_POINT('Ctrl Pts',(-0.251675125750698,0.970900492783582,
-0.982443321918151));
#45565=CARTESIAN_POINT('Ctrl Pts',(-0.0856602820351579,0.999324998131584,
-0.989011079629792));
#45566=CARTESIAN_POINT('Ctrl Pts',(0.0771370307198936,0.986596695500557,
-0.995578837341433));
#45567=CARTESIAN_POINT('Ctrl Pts',(0.239934343474945,0.973868392869529,
-1.00214659505307));
#45568=CARTESIAN_POINT('Ctrl Pts',(0.399514125269508,0.919987282259473,
-1.00871435276472));
#45569=CARTESIAN_POINT('Ctrl Pts',(0.536706852512593,0.831425832859988,
-1.01528211047636));
#45570=CARTESIAN_POINT('Ctrl Pts',(0.673899579755678,0.742864383460502,
-1.021849868188));
#45571=CARTESIAN_POINT('Ctrl Pts',(0.788705252447284,0.619622595271587,
-1.02841762589964));
#45572=CARTESIAN_POINT('Ctrl Pts',(0.867332837498556,0.476504889877957,
-1.03498538361128));
#45573=CARTESIAN_POINT('Ctrl Pts',(0.945960422549827,0.333387184484326,
-1.04155314132292));
#45574=CARTESIAN_POINT('Ctrl Pts',(0.988409919960763,0.170393561885978,
-1.04812089903456));
#45575=CARTESIAN_POINT('Ctrl Pts',(0.98958208324228,0.0071036333497253,
-1.05468865674621));
#45576=CARTESIAN_POINT('Ctrl Pts',(0.990754246523798,-0.156186295186527,
-1.06125641445785));
#45577=CARTESIAN_POINT('Ctrl Pts',(0.950649075675897,-0.319772529660686,
-1.06782417216949));
#45578=CARTESIAN_POINT('Ctrl Pts',(0.874084204925446,-0.464004271295804,
-1.07439192988113));
#45579=CARTESIAN_POINT('Ctrl Pts',(0.797519334174994,-0.608236012930923,
-1.08095968759277));
#45580=CARTESIAN_POINT('Ctrl Pts',(0.684494763521991,-0.733113261727003,
-1.08752744530441));
#45581=CARTESIAN_POINT('Ctrl Pts',(0.548587571147204,-0.823635136370293,
-1.09409520301605));
#45582=CARTESIAN_POINT('Ctrl Pts',(0.412680378772416,-0.914157011013583,
-1.1006629607277));
#45583=CARTESIAN_POINT('Ctrl Pts',(0.253890564675843,-0.970323511504083,
-1.10723071843934));
#45584=CARTESIAN_POINT('Ctrl Pts',(0.091292757567354,-0.985387636159825,
-1.11379847615098));
#45585=CARTESIAN_POINT('Ctrl Pts',(-0.0713050495411349,-1.00045176081557,
-1.12036623386262));
#45586=CARTESIAN_POINT('Ctrl Pts',(-0.23771084966154,-0.97441350963655,
-1.12693399157426));
#45587=CARTESIAN_POINT('Ctrl Pts',(-0.38793514365297,-0.910400727921418,
-1.1335017492859));
#45588=CARTESIAN_POINT('Ctrl Pts',(-0.538159437644401,-0.846387946206286,
-1.14006950699754));
#45589=CARTESIAN_POINT('Ctrl Pts',(-0.672202225506858,-0.744400633955038,
-1.14663726470919));
#45590=CARTESIAN_POINT('Ctrl Pts',(-0.773961615413973,-0.616690018523645,
-1.15320502242083));
#45591=CARTESIAN_POINT('Ctrl Pts',(-0.875721005321089,-0.488979403092252,
-1.15977278013247));
#45592=CARTESIAN_POINT('Ctrl Pts',(-0.945196997272862,-0.335545484480712,
-1.16634053784411));
#45593=CARTESIAN_POINT('Ctrl Pts',(-0.974043786733467,-0.174819514376474,
-1.17290829555575));
#45594=CARTESIAN_POINT('Ctrl Pts',(-0.984388805724034,-0.117180059723252,
-1.17526362103643));
#45595=CARTESIAN_POINT('Ctrl Pts',(-0.989508588688577,-0.0586027897099681,
-1.17761894651711));
#45596=CARTESIAN_POINT('Ctrl Pts',(-0.989468413969488,-1.8577996640623E-5,
-1.17997427199779));
#45597=CARTESIAN_POINT('Ctrl Pts',(-0.989466234208983,-1.79285505235583E-5,
-1.21597572800221));
#45598=CARTESIAN_POINT('Ctrl Pts',(-0.989505577965029,-0.0596504958599335,
-1.21357826940885));
#45599=CARTESIAN_POINT('Ctrl Pts',(-0.984199910544476,-0.119276144025869,
-1.21118081081549));
#45600=CARTESIAN_POINT('Ctrl Pts',(-0.973483506439899,-0.177912931038826,
-1.20878335222212));
#45601=CARTESIAN_POINT('Ctrl Pts',(-0.944126275456312,-0.338546449864369,
-1.20221559451048));
#45602=CARTESIAN_POINT('Ctrl Pts',(-0.874163212328713,-0.491758884956497,
-1.19564783679884));
#45603=CARTESIAN_POINT('Ctrl Pts',(-0.771998631025041,-0.619145590339313,
-1.1890800790872));
#45604=CARTESIAN_POINT('Ctrl Pts',(-0.669834049721368,-0.746532295722131,
-1.18251232137556));
#45605=CARTESIAN_POINT('Ctrl Pts',(-0.535467950241621,-0.848093271395637,
-1.17594456366392));
#45606=CARTESIAN_POINT('Ctrl Pts',(-0.385041062224816,-0.911628503691119,
-1.16937680595228));
#45607=CARTESIAN_POINT('Ctrl Pts',(-0.234614174208011,-0.975163735986602,
-1.16280904824063));
#45608=CARTESIAN_POINT('Ctrl Pts',(-0.0681264976541487,-1.00067322490406,
-1.15624129052899));
#45609=CARTESIAN_POINT('Ctrl Pts',(0.0944226328881091,-0.985092642719303,
-1.14967353281735));
#45610=CARTESIAN_POINT('Ctrl Pts',(0.256971763430366,-0.969512060534544,
-1.14310577510571));
#45611=CARTESIAN_POINT('Ctrl Pts',(0.415582347961017,-0.912841407247569,
-1.13653801739407));
#45612=CARTESIAN_POINT('Ctrl Pts',(0.551201287724399,-0.821888245902224,
-1.12997025968243));
#45613=CARTESIAN_POINT('Ctrl Pts',(0.686820227487781,-0.730935084556877,
-1.12340250197079));
#45614=CARTESIAN_POINT('Ctrl Pts',(0.799447522483893,-0.60569941515316,
-1.11683474425915));
#45615=CARTESIAN_POINT('Ctrl Pts',(0.875553817275981,-0.461225174285523,
-1.1102669865475));
#45616=CARTESIAN_POINT('Ctrl Pts',(0.951660112068069,-0.316750933417886,
-1.10369922883586));
#45617=CARTESIAN_POINT('Ctrl Pts',(0.991245406656133,-0.153038121086327,
-1.09713147112422));
#45618=CARTESIAN_POINT('Ctrl Pts',(0.989554516956521,0.0102472587652755,
-1.09056371341258));
#45619=CARTESIAN_POINT('Ctrl Pts',(0.987863627256909,0.173532638616877,
-1.08399595570094));
#45620=CARTESIAN_POINT('Ctrl Pts',(0.944896553269623,0.336390585988523,
-1.0774281979893));
#45621=CARTESIAN_POINT('Ctrl Pts',(0.865814715377448,0.479257787601961,
-1.07086044027766));
#45622=CARTESIAN_POINT('Ctrl Pts',(0.786732877485274,0.622124989215399,
-1.06429268256602));
#45623=CARTESIAN_POINT('Ctrl Pts',(0.67153627568821,0.745001445070627,-1.05772492485437));
#45624=CARTESIAN_POINT('Ctrl Pts',(0.53406290343955,0.833126619134794,-1.05115716714273));
#45625=CARTESIAN_POINT('Ctrl Pts',(0.39658953119089,0.921251793198961,-1.04458940943109));
#45626=CARTESIAN_POINT('Ctrl Pts',(0.236839388490635,0.974625685472067,
-1.03802165171945));
#45627=CARTESIAN_POINT('Ctrl Pts',(0.0740024635360275,0.986836756374557,
-1.03145389400781));
#45628=CARTESIAN_POINT('Ctrl Pts',(-0.0888344614185813,0.999047827277046,
-1.02488613629617));
#45629=CARTESIAN_POINT('Ctrl Pts',(-0.254758168627542,0.970096076808919,
-1.01831837858452));
#45630=CARTESIAN_POINT('Ctrl Pts',(-0.403837070367909,0.903459334412967,
-1.01175062087288));
#45631=CARTESIAN_POINT('Ctrl Pts',(-0.552915972108275,0.836822592017015,
-1.00518286316124));
#45632=CARTESIAN_POINT('Ctrl Pts',(-0.685150068380046,0.73250085769324,
-0.998615105449601));
#45633=CARTESIAN_POINT('Ctrl Pts',(-0.78465473646029,0.603025781282765,
-0.99204734773796));
#45634=CARTESIAN_POINT('Ctrl Pts',(-0.884159404540536,0.473550704872287,
-0.985479590026318));
#45635=CARTESIAN_POINT('Ctrl Pts',(-0.950934644429253,0.318922286375109,
-0.978911832314676));
#45636=CARTESIAN_POINT('Ctrl Pts',(-0.976959079471164,0.157715266794669,
-0.972344074603035));
#45637=CARTESIAN_POINT('Ctrl Pts',(-0.985370505395306,0.105611123074779,
-0.97022129240276));
#45638=CARTESIAN_POINT('Ctrl Pts',(-0.989524841441287,0.0528197365828913,
-0.968098510202484));
#45639=CARTESIAN_POINT('Ctrl Pts',(-0.989481817826863,2.16465008535149E-5,
-0.965975728002209));
#45640=CARTESIAN_POINT('Origin',(0.,0.,-0.915));
#45641=CARTESIAN_POINT('',(-0.989606782241323,3.0037068674809E-6,-0.67997427199779));
#45642=CARTESIAN_POINT('',(-0.989607241147724,1.92919255151051E-6,-0.71597572800221));
#45643=CARTESIAN_POINT('',(-0.989525,-1.21181862392628E-16,-0.915));
#45644=CARTESIAN_POINT('Ctrl Pts',(-0.989606782241323,3.0037068674809E-6,
-0.67997427199779));
#45645=CARTESIAN_POINT('Ctrl Pts',(-0.989607295470647,0.00292188642515435,
-0.680091670392743));
#45646=CARTESIAN_POINT('Ctrl Pts',(-0.989594647512363,0.00584076467806051,
-0.680209068787695));
#45647=CARTESIAN_POINT('Ctrl Pts',(-0.989568811039347,0.00875952618805917,
-0.680326467182648));
#45648=CARTESIAN_POINT('Ctrl Pts',(-0.988123410572325,0.172047264691672,
-0.686894224894289));
#45649=CARTESIAN_POINT('Ctrl Pts',(-0.945401229584537,0.334969626845597,
-0.69346198260593));
#45650=CARTESIAN_POINT('Ctrl Pts',(-0.8665342706836,0.477955561544956,-0.700029740317572));
#45651=CARTESIAN_POINT('Ctrl Pts',(-0.787667311782663,0.620941496244314,
-0.706597498029213));
#45652=CARTESIAN_POINT('Ctrl Pts',(-0.672655574968577,0.743991003489105,
-0.713165255740855));
#45653=CARTESIAN_POINT('Ctrl Pts',(-0.535314846785921,0.832322759445795,
-0.719733013452496));
#45654=CARTESIAN_POINT('Ctrl Pts',(-0.397974118603265,0.920654515402485,
-0.726300771164138));
#45655=CARTESIAN_POINT('Ctrl Pts',(-0.238304399052039,0.974268520071073,
-0.732868528875779));
#45656=CARTESIAN_POINT('Ctrl Pts',(-0.0754860154975323,0.986724390367039,
-0.73943628658742));
#45657=CARTESIAN_POINT('Ctrl Pts',(0.0873323680569721,0.999180260663004,
-0.746004044299061));
#45658=CARTESIAN_POINT('Ctrl Pts',(0.253299415614757,0.970477996586349,
-0.752571802010703));
#45659=CARTESIAN_POINT('Ctrl Pts',(0.40247833319284,0.904065458023485,-0.759139559722344));
#45660=CARTESIAN_POINT('Ctrl Pts',(0.551657250770926,0.837652919460619,
-0.765707317433986));
#45661=CARTESIAN_POINT('Ctrl Pts',(0.68404803836931,0.733530106411544,-0.772275075145627));
#45662=CARTESIAN_POINT('Ctrl Pts',(0.78374725071719,0.604204773296391,-0.778842832857268));
#45663=CARTESIAN_POINT('Ctrl Pts',(0.88344646306507,0.47487944018124,-0.78541059056891));
#45664=CARTESIAN_POINT('Ctrl Pts',(0.950454100162448,0.320351587000007,
-0.791978348280551));
#45665=CARTESIAN_POINT('Ctrl Pts',(0.976720868636,0.159183874346109,-0.798546105992192));
#45666=CARTESIAN_POINT('Ctrl Pts',(1.00298763710955,-0.00198383830779042,
-0.805113863703834));
#45667=CARTESIAN_POINT('Ctrl Pts',(0.988513536959279,-0.169791410434359,
-0.811681621415475));
#45668=CARTESIAN_POINT('Ctrl Pts',(0.935037269674611,-0.324080955010237,
-0.818249379127116));
#45669=CARTESIAN_POINT('Ctrl Pts',(0.881561002389944,-0.478370499586115,
-0.824817136838758));
#45670=CARTESIAN_POINT('Ctrl Pts',(0.789082567970882,-0.619142016611303,
-0.831384894550399));
#45671=CARTESIAN_POINT('Ctrl Pts',(0.668710939686584,-0.729485325571656,
-0.837952652262041));
#45672=CARTESIAN_POINT('Ctrl Pts',(0.548339311402286,-0.839828634532009,
-0.844520409973682));
#45673=CARTESIAN_POINT('Ctrl Pts',(0.400074489252753,-0.919743735427527,
-0.851088167685324));
#45674=CARTESIAN_POINT('Ctrl Pts',(0.241726787138328,-0.95963082560987,
-0.857655925396965));
#45675=CARTESIAN_POINT('Ctrl Pts',(0.0833790850239023,-0.999517915792213,
-0.864223683108606));
#45676=CARTESIAN_POINT('Ctrl Pts',(-0.0850514970554142,-0.99937699526138,
-0.870791440820247));
#45677=CARTESIAN_POINT('Ctrl Pts',(-0.243332232996699,-0.959224992098172,
-0.877359198531889));
#45678=CARTESIAN_POINT('Ctrl Pts',(-0.401612968937987,-0.919072988934964,
-0.88392695624353));
#45679=CARTESIAN_POINT('Ctrl Pts',(-0.549743858741242,-0.838909903139379,
-0.890494713955172));
#45680=CARTESIAN_POINT('Ctrl Pts',(-0.66993067713115,-0.728365326549457,
-0.897062471666814));
#45681=CARTESIAN_POINT('Ctrl Pts',(-0.790117495521055,-0.617820749959539,
-0.903630229378455));
#45682=CARTESIAN_POINT('Ctrl Pts',(-0.882360242497614,-0.476894682575286,
-0.910197987090096));
#45683=CARTESIAN_POINT('Ctrl Pts',(-0.935578256749101,-0.322515870274955,
-0.916765744801737));
#45684=CARTESIAN_POINT('Ctrl Pts',(-0.971254135764085,-0.219024601245696,
-0.921168587200421));
#45685=CARTESIAN_POINT('Ctrl Pts',(-0.989392341652577,-0.109487683046862,
-0.925571429599106));
#45686=CARTESIAN_POINT('Ctrl Pts',(-0.989479227929023,2.11592729404686E-5,
-0.929974271997791));
#45687=CARTESIAN_POINT('Ctrl Pts',(-0.989481817826863,2.16465008535149E-5,
-0.965975728002209));
#45688=CARTESIAN_POINT('Ctrl Pts',(-0.989391729021473,-0.110534310408492,
-0.961530752490843));
#45689=CARTESIAN_POINT('Ctrl Pts',(-0.970897986417988,-0.221119659736481,
-0.957085776979477));
#45690=CARTESIAN_POINT('Ctrl Pts',(-0.934548975441814,-0.325486345092866,
-0.952640801468111));
#45691=CARTESIAN_POINT('Ctrl Pts',(-0.880840806175447,-0.479695316736262,
-0.94607304375647));
#45692=CARTESIAN_POINT('Ctrl Pts',(-0.788150837447608,-0.620327639359355,
-0.939505286044829));
#45693=CARTESIAN_POINT('Ctrl Pts',(-0.667613453089349,-0.73048985317756,
-0.932937528333187));
#45694=CARTESIAN_POINT('Ctrl Pts',(-0.547076068731089,-0.840652066995765,
-0.926369770621545));
#45695=CARTESIAN_POINT('Ctrl Pts',(-0.398691268742412,-0.920344172009081,
-0.919802012909904));
#45696=CARTESIAN_POINT('Ctrl Pts',(-0.240283779363316,-0.959993152952737,
-0.913234255198263));
#45697=CARTESIAN_POINT('Ctrl Pts',(-0.0818762899842206,-0.999642133896393,
-0.906666497486621));
#45698=CARTESIAN_POINT('Ctrl Pts',(0.0865538887852915,-0.999247990770388,
-0.90009873977498));
#45699=CARTESIAN_POINT('Ctrl Pts',(0.244774079289893,-0.958858070023422,
-0.893530982063339));
#45700=CARTESIAN_POINT('Ctrl Pts',(0.402994269794494,-0.918468149276455,
-0.886963224351698));
#45701=CARTESIAN_POINT('Ctrl Pts',(0.551004472034184,-0.838082450908528,
-0.880395466640056));
#45702=CARTESIAN_POINT('Ctrl Pts',(0.671024958328965,-0.727357308096143,
-0.873827708928415));
#45703=CARTESIAN_POINT('Ctrl Pts',(0.791045444623745,-0.616632165283759,
-0.867259951216773));
#45704=CARTESIAN_POINT('Ctrl Pts',(0.883076214973616,-0.475567578026917,
-0.860692193505132));
#45705=CARTESIAN_POINT('Ctrl Pts',(0.936062071762188,-0.32110893190557,
-0.854124435793491));
#45706=CARTESIAN_POINT('Ctrl Pts',(0.989047928550761,-0.166650285784224,
-0.84755667808185));
#45707=CARTESIAN_POINT('Ctrl Pts',(1.00298887177804,0.00120241920163183,
-0.840988920370208));
#45708=CARTESIAN_POINT('Ctrl Pts',(0.976210245437653,0.162285874443257,
-0.834421162658567));
#45709=CARTESIAN_POINT('Ctrl Pts',(0.94943161909727,0.323369329684882,-0.827853404946925));
#45710=CARTESIAN_POINT('Ctrl Pts',(0.881933423189232,0.477683535182278,
-0.821285647235283));
#45711=CARTESIAN_POINT('Ctrl Pts',(0.781823879471064,0.606691494773144,
-0.814717889523642));
#45712=CARTESIAN_POINT('Ctrl Pts',(0.681714335752896,0.735699454364011,
-0.808150131812001));
#45713=CARTESIAN_POINT('Ctrl Pts',(0.548993444224598,0.839401168048346,
-0.80158237410036));
#45714=CARTESIAN_POINT('Ctrl Pts',(0.399604303896325,0.905339465973283,
-0.795014616388719));
#45715=CARTESIAN_POINT('Ctrl Pts',(0.250215163568049,0.971277763898222,
-0.788446858677077));
#45716=CARTESIAN_POINT('Ctrl Pts',(0.0841577744397947,0.999452646063762,
-0.781879100965435));
#45717=CARTESIAN_POINT('Ctrl Pts',(-0.078620217223007,0.986479604343173,
-0.775311343253794));
#45718=CARTESIAN_POINT('Ctrl Pts',(-0.241398208885805,0.973506562622584,
-0.768743585542152));
#45719=CARTESIAN_POINT('Ctrl Pts',(-0.400896803083149,0.919385597015869,
-0.762175827830512));
#45720=CARTESIAN_POINT('Ctrl Pts',(-0.53795622888534,0.830617989297559,
-0.755608070118871));
#45721=CARTESIAN_POINT('Ctrl Pts',(-0.675015654687532,0.741850381579249,
-0.749040312407229));
#45722=CARTESIAN_POINT('Ctrl Pts',(-0.78963591209457,0.618436131749344,
-0.742472554695587));
#45723=CARTESIAN_POINT('Ctrl Pts',(-0.86804824103133,0.475200378349671,
-0.735904796983945));
#45724=CARTESIAN_POINT('Ctrl Pts',(-0.94646056996809,0.331964624949999,
-0.729337039272304));
#45725=CARTESIAN_POINT('Ctrl Pts',(-0.988664970434574,0.168907367980558,
-0.722769281560663));
#45726=CARTESIAN_POINT('Ctrl Pts',(-0.989591638215686,0.00561586278790557,
-0.716201523849022));
#45727=CARTESIAN_POINT('Ctrl Pts',(-0.989602257656167,0.00374457249822986,
-0.716126258566751));
#45728=CARTESIAN_POINT('Ctrl Pts',(-0.98960745620187,0.00187325144535842,
-0.716050993284481));
#45729=CARTESIAN_POINT('Ctrl Pts',(-0.989607241147724,1.92919255151051E-6,
-0.71597572800221));
#45730=CARTESIAN_POINT('Origin',(0.,0.,-0.915));
#45731=CARTESIAN_POINT('',(-0.98949450850966,-2.34504978581795E-5,-0.429974271997791));
#45732=CARTESIAN_POINT('',(-0.989491623038811,-2.31174877268823E-5,-0.465975728002209));
#45733=CARTESIAN_POINT('',(-0.989525,-1.21181862392628E-16,-0.915));
#45734=CARTESIAN_POINT('Ctrl Pts',(-0.98949450850966,-2.34504978581795E-5,
-0.429974271997791));
#45735=CARTESIAN_POINT('Ctrl Pts',(-0.989390629923838,0.11532021613374,
-0.43461191118638));
#45736=CARTESIAN_POINT('Ctrl Pts',(-0.969224635588088,0.230699262194344,
-0.439249550374969));
#45737=CARTESIAN_POINT('Ctrl Pts',(-0.929722368496541,0.339027253322421,
-0.443887189563558));
#45738=CARTESIAN_POINT('Ctrl Pts',(-0.873779827740854,0.492439791509651,
-0.4504549472752));
#45739=CARTESIAN_POINT('Ctrl Pts',(-0.779056814575157,0.631710863824647,
-0.457022704986841));
#45740=CARTESIAN_POINT('Ctrl Pts',(-0.656931932066817,0.740110530759358,
-0.463590462698482));
#45741=CARTESIAN_POINT('Ctrl Pts',(-0.534807049558477,0.848510197694069,
-0.470158220410124));
#45742=CARTESIAN_POINT('Ctrl Pts',(-0.385280297707493,0.926038459248495,
-0.476725978121765));
#45743=CARTESIAN_POINT('Ctrl Pts',(-0.226313579867206,0.963382231852442,
-0.483293735833407));
#45744=CARTESIAN_POINT('Ctrl Pts',(-0.0673468620269185,1.00072600445639,
-0.489861493545048));
#45745=CARTESIAN_POINT('Ctrl Pts',(0.101059821802673,0.997885288109858,
-0.496429251256689));
#45746=CARTESIAN_POINT('Ctrl Pts',(0.258676616361611,0.955201323921211,
-0.502997008968331));
#45747=CARTESIAN_POINT('Ctrl Pts',(0.41629341092055,0.912517359732565,-0.509564766679972));
#45748=CARTESIAN_POINT('Ctrl Pts',(0.563120316208835,0.829990147701802,
-0.516132524391613));
#45749=CARTESIAN_POINT('Ctrl Pts',(0.681519748076804,0.717533270356876,
-0.522700282103255));
#45750=CARTESIAN_POINT('Ctrl Pts',(0.799919179944774,0.60507639301195,-0.529268039814896));
#45751=CARTESIAN_POINT('Ctrl Pts',(0.889891138392427,0.46268985035286,-0.535835797526538));
#45752=CARTESIAN_POINT('Ctrl Pts',(0.940627740629528,0.307477827875477,
-0.542403555238179));
#45753=CARTESIAN_POINT('Ctrl Pts',(0.991364342866629,0.15226580539809,-0.54897131294982));
#45754=CARTESIAN_POINT('Ctrl Pts',(1.00286558889318,-0.0157716968975903,
-0.555539070661462));
#45755=CARTESIAN_POINT('Ctrl Pts',(0.973749891355825,-0.176449171625418,
-0.562106828373103));
#45756=CARTESIAN_POINT('Ctrl Pts',(0.944634193818474,-0.337126646353242,
-0.568674586084745));
#45757=CARTESIAN_POINT('Ctrl Pts',(0.874901552717228,-0.49044409351321,
-0.575242343796386));
#45758=CARTESIAN_POINT('Ctrl Pts',(0.772928602574952,-0.617984252551632,
-0.581810101508027));
#45759=CARTESIAN_POINT('Ctrl Pts',(0.670955652432676,-0.745524411590054,
-0.588377859219668));
#45760=CARTESIAN_POINT('Ctrl Pts',(0.536742393249371,-0.847287282506928,
-0.594945616931309));
#45761=CARTESIAN_POINT('Ctrl Pts',(0.38641119471913,-0.911048598965344,
-0.601513374642951));
#45762=CARTESIAN_POINT('Ctrl Pts',(0.236079996188885,-0.974809915423762,
-0.608081132354592));
#45763=CARTESIAN_POINT('Ctrl Pts',(0.0696308583117035,-1.00056967742372,
-0.614648890066234));
#45764=CARTESIAN_POINT('Ctrl Pts',(-0.092941513821779,-0.985233493182963,
-0.621216647777876));
#45765=CARTESIAN_POINT('Ctrl Pts',(-0.255513885955259,-0.969897308942204,
-0.627784405489517));
#45766=CARTESIAN_POINT('Ctrl Pts',(-0.414209492345041,-0.91346517846073,
-0.634352163201158));
#45767=CARTESIAN_POINT('Ctrl Pts',(-0.549965020983942,-0.822716012227143,
-0.640919920912799));
#45768=CARTESIAN_POINT('Ctrl Pts',(-0.685720549622844,-0.731966845993555,
-0.647487678624441));
#45769=CARTESIAN_POINT('Ctrl Pts',(-0.798536000510865,-0.606900644007853,
-0.654055436336083));
#45770=CARTESIAN_POINT('Ctrl Pts',(-0.874859415981747,-0.46254098558835,
-0.660623194047724));
#45771=CARTESIAN_POINT('Ctrl Pts',(-0.949818553586881,-0.320761750037418,
-0.667073553364413));
#45772=CARTESIAN_POINT('Ctrl Pts',(-0.989578583273582,-0.160372632977547,
-0.673523912681102));
#45773=CARTESIAN_POINT('Ctrl Pts',(-0.989606782241323,3.0037068674809E-6,
-0.67997427199779));
#45774=CARTESIAN_POINT('Ctrl Pts',(-0.989607241147724,1.92919255151051E-6,
-0.71597572800221));
#45775=CARTESIAN_POINT('Ctrl Pts',(-0.989588690265119,-0.16142104289649,
-0.709483235572839));
#45776=CARTESIAN_POINT('Ctrl Pts',(-0.949287337941748,-0.322852943750881,
-0.702990743143468));
#45777=CARTESIAN_POINT('Ctrl Pts',(-0.873385615756844,-0.465317863970741,
-0.696498250714097));
#45778=CARTESIAN_POINT('Ctrl Pts',(-0.796603990421151,-0.609434332120872,
-0.689930493002456));
#45779=CARTESIAN_POINT('Ctrl Pts',(-0.683391804654025,-0.734141515005271,
-0.683362735290815));
#45780=CARTESIAN_POINT('Ctrl Pts',(-0.547348673904517,-0.82445896048028,
-0.676794977579174));
#45781=CARTESIAN_POINT('Ctrl Pts',(-0.41130554315501,-0.91477640595529,
-0.670227219867532));
#45782=CARTESIAN_POINT('Ctrl Pts',(-0.252431467423123,-0.970704114020911,
-0.66365946215589));
#45783=CARTESIAN_POINT('Ctrl Pts',(-0.0898111973488909,-0.98552376793866,
-0.657091704444249));
#45784=CARTESIAN_POINT('Ctrl Pts',(0.0728090727253406,-1.00034342185641,
-0.650523946732607));
#45785=CARTESIAN_POINT('Ctrl Pts',(0.239175537141915,-0.974055021626288,
-0.643956189020967));
#45786=CARTESIAN_POINT('Ctrl Pts',(0.389303421961953,-0.909816461705308,
-0.637388431309325));
#45787=CARTESIAN_POINT('Ctrl Pts',(0.539431306781992,-0.845577901784329,
-0.630820673597684));
#45788=CARTESIAN_POINT('Ctrl Pts',(0.673320612005493,-0.743389182172492,
-0.624252915886042));
#45789=CARTESIAN_POINT('Ctrl Pts',(0.774887882910271,-0.615525724287871,
-0.617685158174401));
#45790=CARTESIAN_POINT('Ctrl Pts',(0.876455153815049,-0.487662266403251,
-0.61111740046276));
#45791=CARTESIAN_POINT('Ctrl Pts',(0.945700390401103,-0.334124070245847,
-0.604549642751119));
#45792=CARTESIAN_POINT('Ctrl Pts',(0.974305507624321,-0.173354913844795,
-0.597981885039477));
#45793=CARTESIAN_POINT('Ctrl Pts',(1.00291062484754,-0.0125857574437444,
-0.591414127327836));
#45794=CARTESIAN_POINT('Ctrl Pts',(0.990875622707922,0.155414359200951,
-0.584846369616194));
#45795=CARTESIAN_POINT('Ctrl Pts',(0.939646206011021,0.31046441965291,-0.578278611904553));
#45796=CARTESIAN_POINT('Ctrl Pts',(0.88841678931412,0.465514480104868,-0.571710854192912));
#45797=CARTESIAN_POINT('Ctrl Pts',(0.797992958059933,0.607614484364092,
-0.56514309648127));
#45798=CARTESIAN_POINT('Ctrl Pts',(0.679236876283086,0.719694667368287,
-0.558575338769629));
#45799=CARTESIAN_POINT('Ctrl Pts',(0.560480794506238,0.831774850372484,
-0.552007581057988));
#45800=CARTESIAN_POINT('Ctrl Pts',(0.413392462206728,0.913835212121657,
-0.545439823346346));
#45801=CARTESIAN_POINT('Ctrl Pts',(0.255640867424106,0.956018250476421,
-0.538872065634705));
#45802=CARTESIAN_POINT('Ctrl Pts',(0.0978892726414824,0.998201288831184,
-0.532304307923063));
#45803=CARTESIAN_POINT('Ctrl Pts',(-0.0705255846242527,1.00050700379154,
-0.525736550211422));
#45804=CARTESIAN_POINT('Ctrl Pts',(-0.229372867212486,0.962658421314677,
-0.51916879249978));
#45805=CARTESIAN_POINT('Ctrl Pts',(-0.388220149800715,0.924809838837817,
-0.512601034788139));
#45806=CARTESIAN_POINT('Ctrl Pts',(-0.537499857711443,0.846806958923747,
-0.506033277076498));
#45807=CARTESIAN_POINT('Ctrl Pts',(-0.659279763879886,0.738019878647646,
-0.499465519364857));
#45808=CARTESIAN_POINT('Ctrl Pts',(-0.781059670048333,0.629232798371543,
-0.492897761653215));
#45809=CARTESIAN_POINT('Ctrl Pts',(-0.875339774474493,0.489661517733408,
-0.486330003941574));
#45810=CARTESIAN_POINT('Ctrl Pts',(-0.930794678249116,0.336072038834401,
-0.479762246229932));
#45811=CARTESIAN_POINT('Ctrl Pts',(-0.969596862864337,0.228604404602891,
-0.475166740154025));
#45812=CARTESIAN_POINT('Ctrl Pts',(-0.989390621669975,0.114273602193131,
-0.470571234078117));
#45813=CARTESIAN_POINT('Ctrl Pts',(-0.989491623038811,-2.31174877268823E-5,
-0.465975728002209));
#45814=CARTESIAN_POINT('Origin',(0.,0.,-0.915));
#45815=CARTESIAN_POINT('',(-0.989456987247134,1.47486280241971E-5,-0.17997427199779));
#45816=CARTESIAN_POINT('',(-0.989459186063674,1.5401373482473E-5,-0.215975728002209));
#45817=CARTESIAN_POINT('',(-0.989525,-1.21181862392628E-16,-0.915));
#45818=CARTESIAN_POINT('Ctrl Pts',(-0.989456987247134,1.47486280241971E-5,
-0.17997427199779));
#45819=CARTESIAN_POINT('Ctrl Pts',(-0.989491616529124,0.064441050262125,
-0.182564394268375));
#45820=CARTESIAN_POINT('Ctrl Pts',(-0.983293285821839,0.128860829012359,
-0.18515451653896));
#45821=CARTESIAN_POINT('Ctrl Pts',(-0.97079687644072,0.192034862932722,
-0.187744638809545));
#45822=CARTESIAN_POINT('Ctrl Pts',(-0.939109805134186,0.352224886843149,
-0.194312396521186));
#45823=CARTESIAN_POINT('Ctrl Pts',(-0.86692769727473,0.504405089817102,
-0.200880154232828));
#45824=CARTESIAN_POINT('Ctrl Pts',(-0.762923262955385,0.630294367333439,
-0.207447911944469));
#45825=CARTESIAN_POINT('Ctrl Pts',(-0.658918828636039,0.756183644849777,
-0.214015669656111));
#45826=CARTESIAN_POINT('Ctrl Pts',(-0.523092067856803,0.8557819969085,-0.220583427367752));
#45827=CARTESIAN_POINT('Ctrl Pts',(-0.371758245998546,0.917125400129355,
-0.227151185079393));
#45828=CARTESIAN_POINT('Ctrl Pts',(-0.22042442414029,0.97846880335021,-0.233718942791035));
#45829=CARTESIAN_POINT('Ctrl Pts',(-0.0535835412030128,1.0015572577332,
-0.240286700502676));
#45830=CARTESIAN_POINT('Ctrl Pts',(0.108722171403071,0.983617146112767,
-0.246854458214317));
#45831=CARTESIAN_POINT('Ctrl Pts',(0.271027884009149,0.965677034492338,
-0.253422215925958));
#45832=CARTESIAN_POINT('Ctrl Pts',(0.428798426284033,0.906708356868494,
-0.2599899736376));
#45833=CARTESIAN_POINT('Ctrl Pts',(0.563081845971233,0.813794785223099,
-0.266557731349241));
#45834=CARTESIAN_POINT('Ctrl Pts',(0.697365265658436,0.720881213577702,
-0.273125489060882));
#45835=CARTESIAN_POINT('Ctrl Pts',(0.808161562757956,0.594022747910746,
-0.279693246772524));
#45836=CARTESIAN_POINT('Ctrl Pts',(0.882161211042825,0.448458233569121,
-0.286261004484165));
#45837=CARTESIAN_POINT('Ctrl Pts',(0.956160859327694,0.302893719227494,
-0.292828762195807));
#45838=CARTESIAN_POINT('Ctrl Pts',(0.993363858797916,0.138623156211191,
-0.299396519907448));
#45839=CARTESIAN_POINT('Ctrl Pts',(0.989301258947878,-0.0246204367359938,
-0.30596427761909));
#45840=CARTESIAN_POINT('Ctrl Pts',(0.985238659097841,-0.187864029683177,
-0.312532035330731));
#45841=CARTESIAN_POINT('Ctrl Pts',(0.939910459927547,-0.35008065256124,
-0.319099793042372));
#45842=CARTESIAN_POINT('Ctrl Pts',(0.858761681530321,-0.491784038779624,
-0.325667550754014));
#45843=CARTESIAN_POINT('Ctrl Pts',(0.777612903133097,-0.633487424998005,
-0.332235308465655));
#45844=CARTESIAN_POINT('Ctrl Pts',(0.660643545508944,-0.754677574556705,
-0.338803066177296));
#45845=CARTESIAN_POINT('Ctrl Pts',(0.52190456983259,-0.840796515164743,
-0.345370823888938));
#45846=CARTESIAN_POINT('Ctrl Pts',(0.383165594156234,-0.926915455772781,
-0.351938581600579));
#45847=CARTESIAN_POINT('Ctrl Pts',(0.222657000427679,-0.977963187430155,
-0.35850633931222));
#45848=CARTESIAN_POINT('Ctrl Pts',(0.0596598780034666,-0.987807602567975,
-0.365074097023862));
#45849=CARTESIAN_POINT('Ctrl Pts',(-0.103337244420748,-0.997652017705794,
-0.371641854735503));
#45850=CARTESIAN_POINT('Ctrl Pts',(-0.268822895540619,-0.966293116324059,
-0.378209612447145));
#45851=CARTESIAN_POINT('Ctrl Pts',(-0.416918105195915,-0.897497885927143,
-0.384777370158786));
#45852=CARTESIAN_POINT('Ctrl Pts',(-0.565013314851208,-0.828702655530228,
-0.391345127870427));
#45853=CARTESIAN_POINT('Ctrl Pts',(-0.695718083041927,-0.722471096118137,
-0.397912885582069));
#45854=CARTESIAN_POINT('Ctrl Pts',(-0.793331499589108,-0.591564275791708,
-0.40448064329371));
#45855=CARTESIAN_POINT('Ctrl Pts',(-0.890944916136291,-0.460657455465276,
-0.411048401005351));
#45856=CARTESIAN_POINT('Ctrl Pts',(-0.955466981039936,-0.305075374224508,
-0.417616158716993));
#45857=CARTESIAN_POINT('Ctrl Pts',(-0.97914697931892,-0.143507331574391,
-0.424183916428634));
#45858=CARTESIAN_POINT('Ctrl Pts',(-0.986106006327955,-0.096026062388788,
-0.426114034951686));
#45859=CARTESIAN_POINT('Ctrl Pts',(-0.989537741278422,-0.0480278204863994,
-0.428044153474738));
#45860=CARTESIAN_POINT('Ctrl Pts',(-0.98949450850966,-2.34504978581795E-5,
-0.429974271997791));
#45861=CARTESIAN_POINT('Ctrl Pts',(-0.989491623038811,-2.31174877268823E-5,
-0.465975728002209));
#45862=CARTESIAN_POINT('Ctrl Pts',(-0.98953496975876,-0.049075798221059,
-0.464003476366476));
#45863=CARTESIAN_POINT('Ctrl Pts',(-0.985951175030704,-0.0981222013734553,
-0.462031224730742));
#45864=CARTESIAN_POINT('Ctrl Pts',(-0.978686144299608,-0.14661711800828,
-0.460058973095008));
#45865=CARTESIAN_POINT('Ctrl Pts',(-0.954493003452389,-0.308109118792077,
-0.453491215383367));
#45866=CARTESIAN_POINT('Ctrl Pts',(-0.889477018634865,-0.463485443199799,
-0.446923457671725));
#45867=CARTESIAN_POINT('Ctrl Pts',(-0.791448235943943,-0.594081508018418,
-0.440355699960084));
#45868=CARTESIAN_POINT('Ctrl Pts',(-0.693419453253019,-0.724677572837039,
-0.433787942248443));
#45869=CARTESIAN_POINT('Ctrl Pts',(-0.562377872688697,-0.830493378066557,
-0.427220184536801));
#45870=CARTESIAN_POINT('Ctrl Pts',(-0.414064866042057,-0.898817798579287,
-0.42065242682516));
#45871=CARTESIAN_POINT('Ctrl Pts',(-0.265751859395417,-0.967142219092016,
-0.414084669113519));
#45872=CARTESIAN_POINT('Ctrl Pts',(-0.100167426666459,-0.997975254887957,
-0.407516911401877));
#45873=CARTESIAN_POINT('Ctrl Pts',(0.0627975998423243,-0.987613087092117,
-0.400949153690236));
#45874=CARTESIAN_POINT('Ctrl Pts',(0.225762626351105,-0.977250919296277,
-0.394381395978595));
#45875=CARTESIAN_POINT('Ctrl Pts',(0.386108246639711,-0.925693547908657,
-0.387813638266953));
#45876=CARTESIAN_POINT('Ctrl Pts',(0.52457294062125,-0.839134302921211,
-0.381245880555312));
#45877=CARTESIAN_POINT('Ctrl Pts',(0.663037634602796,-0.752575057933762,
-0.374678122843671));
#45878=CARTESIAN_POINT('Ctrl Pts',(0.779621402277273,-0.631013939346482,
-0.368110365132029));
#45879=CARTESIAN_POINT('Ctrl Pts',(0.860319617138808,-0.489053478264194,
-0.361542607420388));
#45880=CARTESIAN_POINT('Ctrl Pts',(0.94101783200034,-0.347093017181912,
-0.354974849708746));
#45881=CARTESIAN_POINT('Ctrl Pts',(0.985830494048933,-0.184733213604624,
-0.348407091997105));
#45882=CARTESIAN_POINT('Ctrl Pts',(0.989374481078401,-0.0214775413191292,
-0.341839334285463));
#45883=CARTESIAN_POINT('Ctrl Pts',(0.992918468107869,0.141778130966367,
-0.335271576573822));
#45884=CARTESIAN_POINT('Ctrl Pts',(0.955193780118211,0.30592967196007,-0.328703818862181));
#45885=CARTESIAN_POINT('Ctrl Pts',(0.880732096848492,0.451258375508424,
-0.32213606115054));
#45886=CARTESIAN_POINT('Ctrl Pts',(0.806270413578773,0.596587079056778,
-0.315568303438898));
#45887=CARTESIAN_POINT('Ctrl Pts',(0.695071735028993,0.723092945159784,
-0.309000545727257));
#45888=CARTESIAN_POINT('Ctrl Pts',(0.560493801988416,0.815579454673507,
-0.302432788015615));
#45889=CARTESIAN_POINT('Ctrl Pts',(0.425915868947842,0.908065964187229,
-0.295865030303974));
#45890=CARTESIAN_POINT('Ctrl Pts',(0.267958681416473,0.966533117111669,
-0.289297272592333));
#45891=CARTESIAN_POINT('Ctrl Pts',(0.105596852931962,0.98395754615998,-0.282729514880691));
#45892=CARTESIAN_POINT('Ctrl Pts',(-0.0567649755525518,1.00138197520829,
-0.27616175716905));
#45893=CARTESIAN_POINT('Ctrl Pts',(-0.223531444990207,0.977763680380474,
-0.269593999457409));
#45894=CARTESIAN_POINT('Ctrl Pts',(-0.374669738952996,0.915939809086429,
-0.263026241745767));
#45895=CARTESIAN_POINT('Ctrl Pts',(-0.525808032915786,0.854115937792385,
-0.256458484034126));
#45896=CARTESIAN_POINT('Ctrl Pts',(-0.661318151403709,0.754086490032113,
-0.249890726322485));
#45897=CARTESIAN_POINT('Ctrl Pts',(-0.76492192342027,0.627867505842223,
-0.243322968610843));
#45898=CARTESIAN_POINT('Ctrl Pts',(-0.868525695436832,0.501648521652333,
-0.236755210899202));
#45899=CARTESIAN_POINT('Ctrl Pts',(-0.940223120982031,0.349240001032824,
-0.23018745318756));
#45900=CARTESIAN_POINT('Ctrl Pts',(-0.971401577532646,0.18895001738729,
-0.223619695475919));
#45901=CARTESIAN_POINT('Ctrl Pts',(-0.983497390554236,0.126764845768462,
-0.221071706318016));
#45902=CARTESIAN_POINT('Ctrl Pts',(-0.989494756047049,0.0633934473055932,
-0.218523717160113));
#45903=CARTESIAN_POINT('Ctrl Pts',(-0.989459186063674,1.54013734824731E-5,
-0.215975728002209));
#45904=CARTESIAN_POINT('Origin',(0.,0.,-2.22262968985462));
#45905=CARTESIAN_POINT('',(-0.846841790252493,1.26228372977161E-5,-0.0976296898546191));
#45906=CARTESIAN_POINT('',(-0.8469,-1.79235740772804E-14,-0.0695250000000001));
#45907=CARTESIAN_POINT('',(-0.8469,-1.79235740772804E-14,-2.22262968985462));
#45908=CARTESIAN_POINT('',(-0.644274518039102,-0.549718620818712,-0.0695250000000005));
#45909=CARTESIAN_POINT('Ctrl Pts',(-0.846841790252493,1.26228372976933E-5,
-0.0976296898546191));
#45910=CARTESIAN_POINT('Ctrl Pts',(-0.846796275356015,-0.0846659001015894,
-0.0936520544135628));
#45911=CARTESIAN_POINT('Ctrl Pts',(-0.817058392758087,-0.284133958169113,
-0.0842838244620231));
#45912=CARTESIAN_POINT('Ctrl Pts',(-0.718653225003286,-0.462367489267768,
-0.0749155945104837));
#45913=CARTESIAN_POINT('Ctrl Pts',(-0.644274518039102,-0.549718620818712,
-0.0695250000000004));
#45914=CARTESIAN_POINT('Origin',(0.,0.,-0.0695250000000001));
#45915=CARTESIAN_POINT('Origin',(0.,0.,-2.22262968985462));
#45916=CARTESIAN_POINT('',(-0.846873903394892,-2.00704647690821E-5,-0.347629689854619));
#45917=CARTESIAN_POINT('',(-0.846843672143023,1.31814993880319E-5,-0.298320310145379));
#45918=CARTESIAN_POINT('',(-0.8469,-1.79235740772804E-14,-2.22262968985462));
#45919=CARTESIAN_POINT('Ctrl Pts',(-0.846873903394892,-2.00704647690883E-5,
-0.347629689854619));
#45920=CARTESIAN_POINT('Ctrl Pts',(-0.846910904816649,-0.041105339602276,
-0.345699571331567));
#45921=CARTESIAN_POINT('Ctrl Pts',(-0.833979505501722,-0.221971415046033,
-0.337201695096874));
#45922=CARTESIAN_POINT('Ctrl Pts',(-0.707306548807687,-0.52741796683899,
-0.322136061150539));
#45923=CARTESIAN_POINT('Ctrl Pts',(-0.37170956586924,-0.800177647492136,
-0.302432788015616));
#45924=CARTESIAN_POINT('Ctrl Pts',(0.053190657773669,-0.880694623556987,
-0.282729514880691));
#45925=CARTESIAN_POINT('Ctrl Pts',(0.46531181093922,-0.749624694225347,
-0.263026241745767));
#45926=CARTESIAN_POINT('Ctrl Pts',(0.765641814643713,-0.438457403875131,
-0.243322968610843));
#45927=CARTESIAN_POINT('Ctrl Pts',(0.88202629773607,-0.0219507226429252,
-0.223619695475919));
#45928=CARTESIAN_POINT('Ctrl Pts',(0.786504041346395,0.399829646175967,
-0.203916422340995));
#45929=CARTESIAN_POINT('Ctrl Pts',(0.502023960458353,0.725550879818389,
-0.184213149206071));
#45930=CARTESIAN_POINT('Ctrl Pts',(0.0969330160579518,0.876958594872486,
-0.164509876071146));
#45931=CARTESIAN_POINT('Ctrl Pts',(-0.331446894786887,0.817676781830008,
-0.144806602936223));
#45932=CARTESIAN_POINT('Ctrl Pts',(-0.680195083172024,0.561948494949336,
-0.125103329801299));
#45933=CARTESIAN_POINT('Ctrl Pts',(-0.828114799287869,0.250092093274441,
-0.109377692107431));
#45934=CARTESIAN_POINT('Ctrl Pts',(-0.846871428249427,0.0551528515873726,
-0.100219812125204));
#45935=CARTESIAN_POINT('Ctrl Pts',(-0.846841790252493,1.26228372976933E-5,
-0.0976296898546191));
#45936=CARTESIAN_POINT('',(-0.729452881030877,0.430276776454125,-0.0695250000000001));
#45937=CARTESIAN_POINT('Origin',(0.,0.,-0.0695250000000001));
#45938=CARTESIAN_POINT('Ctrl Pts',(-0.846843672143023,1.31814993879972E-5,
-0.298320310145379));
#45939=CARTESIAN_POINT('Ctrl Pts',(-0.846795644364765,-0.0855619705691921,
-0.294300541591641));
#45940=CARTESIAN_POINT('Ctrl Pts',(-0.81282103441623,-0.310992633879406,
-0.283713015326262));
#45941=CARTESIAN_POINT('Ctrl Pts',(-0.615791113824046,-0.631865040078709,
-0.266557731349242));
#45942=CARTESIAN_POINT('Ctrl Pts',(-0.241553908007489,-0.848589468760584,
-0.246854458214317));
#45943=CARTESIAN_POINT('Ctrl Pts',(0.190717468786097,-0.861440191483295,
-0.227151185079393));
#45944=CARTESIAN_POINT('Ctrl Pts',(0.577167311767125,-0.667330005151926,
-0.207447911944469));
#45945=CARTESIAN_POINT('Ctrl Pts',(0.824955967175025,-0.312893524930918,
-0.187744638809545));
#45946=CARTESIAN_POINT('Ctrl Pts',(0.874542449448201,0.116715157342132,
-0.168041365674621));
#45947=CARTESIAN_POINT('Ctrl Pts',(0.714032896413046,0.518283961256023,
-0.148338092539697));
#45948=CARTESIAN_POINT('Ctrl Pts',(0.381951553088681,0.795333171794517,
-0.128634819404772));
#45949=CARTESIAN_POINT('Ctrl Pts',(-0.0418431784879791,0.88130717347886,
-0.108931546269849));
#45950=CARTESIAN_POINT('Ctrl Pts',(-0.455688651728263,0.755540682228038,
-0.0892282731349243));
#45951=CARTESIAN_POINT('Ctrl Pts',(-0.658428920058076,0.550684467012711,
-0.0760927577116414));
#45952=CARTESIAN_POINT('Ctrl Pts',(-0.729452881030877,0.430276776454125,
-0.0695250000000001));
#45953=CARTESIAN_POINT('Origin',(0.,0.,-2.22262968985462));
#45954=CARTESIAN_POINT('',(-0.846969994573332,2.57076813978431E-6,-0.59762968985462));
#45955=CARTESIAN_POINT('',(-0.846871433820842,-1.97854529844221E-5,-0.54832031014538));
#45956=CARTESIAN_POINT('',(-0.8469,-1.79235740772804E-14,-2.22262968985462));
#45957=CARTESIAN_POINT('Ctrl Pts',(-0.846969994573332,2.57076813976785E-6,
-0.59762968985462));
#45958=CARTESIAN_POINT('Ctrl Pts',(-0.846945860058509,-0.137257353648154,
-0.591179330537931));
#45959=CARTESIAN_POINT('Ctrl Pts',(-0.778268067817394,-0.41429865733857,
-0.5781612135096));
#45960=CARTESIAN_POINT('Ctrl Pts',(-0.490329529944689,-0.733504750596127,
-0.558575338769629));
#45961=CARTESIAN_POINT('Ctrl Pts',(-0.0828633950269074,-0.878399638460791,
-0.538872065634705));
#45962=CARTESIAN_POINT('Ctrl Pts',(0.344510672939591,-0.812258987832161,
-0.51916879249978));
#45963=CARTESIAN_POINT('Ctrl Pts',(0.689116041785277,-0.550973091934125,
-0.499465519364857));
#45964=CARTESIAN_POINT('Ctrl Pts',(0.868161261709926,-0.157315894794747,
-0.479762246229933));
#45965=CARTESIAN_POINT('Ctrl Pts',(0.838630713437117,0.274136450605954,
-0.460058973095008));
#45966=CARTESIAN_POINT('Ctrl Pts',(0.607619112085,0.639727505843516,-0.440355699960084));
#45967=CARTESIAN_POINT('Ctrl Pts',(0.230627001460258,0.851624009324031,
-0.42065242682516));
#45968=CARTESIAN_POINT('Ctrl Pts',(-0.201773252809055,0.858917820012625,
-0.400949153690236));
#45969=CARTESIAN_POINT('Ctrl Pts',(-0.585697477490385,0.659856599597445,
-0.381245880555312));
#45970=CARTESIAN_POINT('Ctrl Pts',(-0.805083150423093,0.337294247548553,
-0.363472725943439));
#45971=CARTESIAN_POINT('Ctrl Pts',(-0.846784997329527,0.098698558443348,
-0.352267329043209));
#45972=CARTESIAN_POINT('Ctrl Pts',(-0.846873903394892,-2.00704647690883E-5,
-0.347629689854619));
#45973=CARTESIAN_POINT('Ctrl Pts',(-0.846871433820842,-1.97854529844013E-5,
-0.54832031014538));
#45974=CARTESIAN_POINT('Ctrl Pts',(-0.846908532769453,-0.0420022672629993,
-0.546348058509646));
#45975=CARTESIAN_POINT('Ctrl Pts',(-0.833627112812173,-0.223766549843529,
-0.537808049162271));
#45976=CARTESIAN_POINT('Ctrl Pts',(-0.705627497577025,-0.529662242982048,
-0.522700282103254));
#45977=CARTESIAN_POINT('Ctrl Pts',(-0.369165716682379,-0.801354435040497,
-0.502997008968331));
#45978=CARTESIAN_POINT('Ctrl Pts',(0.0559881381817874,-0.88052120096025,
-0.483293735833406));
#45979=CARTESIAN_POINT('Ctrl Pts',(0.467690841465955,-0.748142722918232,
-0.463590462698483));
#45980=CARTESIAN_POINT('Ctrl Pts',(0.767030806126306,-0.436022934136046,
-0.443887189563558));
#45981=CARTESIAN_POINT('Ctrl Pts',(0.882091598392154,-0.0191486227757228,
-0.424183916428634));
#45982=CARTESIAN_POINT('Ctrl Pts',(0.785229856874429,0.402326145625984,
-0.40448064329371));
#45983=CARTESIAN_POINT('Ctrl Pts',(0.499716623159844,0.727142046192322,
-0.384777370158786));
#45984=CARTESIAN_POINT('Ctrl Pts',(0.0941464492269416,0.877262048653223,
-0.365074097023862));
#45985=CARTESIAN_POINT('Ctrl Pts',(-0.3340423978464,0.816619819635224,-0.345370823888938));
#45986=CARTESIAN_POINT('Ctrl Pts',(-0.681977576889138,0.559784653343796,
-0.325667550754014));
#45987=CARTESIAN_POINT('Ctrl Pts',(-0.828510399589799,0.248297168818575,
-0.309984046172828));
#45988=CARTESIAN_POINT('Ctrl Pts',(-0.846874115253527,0.0542562446861801,
-0.300868299303283));
#45989=CARTESIAN_POINT('Ctrl Pts',(-0.846843672143023,1.31814993879972E-5,
-0.298320310145379));
#45990=CARTESIAN_POINT('Origin',(0.,0.,-2.22262968985462));
#45991=CARTESIAN_POINT('',(-0.846860825277875,1.81094851073512E-5,-0.84762968985462));
#45992=CARTESIAN_POINT('',(-0.846970387335345,1.65112873686153E-6,-0.79832031014538));
#45993=CARTESIAN_POINT('',(-0.8469,-1.79235740772804E-14,-2.22262968985462));
#45994=CARTESIAN_POINT('Ctrl Pts',(-0.846860825277874,1.81094851073073E-5,
-0.84762968985462));
#45995=CARTESIAN_POINT('Ctrl Pts',(-0.846786462338563,-0.093706696417362,
-0.843226847455935));
#45996=CARTESIAN_POINT('Ctrl Pts',(-0.808105529948621,-0.327301471617268,
-0.83225624734561));
#45997=CARTESIAN_POINT('Ctrl Pts',(-0.597286702753671,-0.649384987350965,
-0.814717889523642));
#45998=CARTESIAN_POINT('Ctrl Pts',(-0.21694648727339,-0.855211370798415,
-0.795014616388718));
#45999=CARTESIAN_POINT('Ctrl Pts',(0.215515128035896,-0.855573197728189,
-0.775311343253795));
#46000=CARTESIAN_POINT('Ctrl Pts',(0.596199227614297,-0.650383539209966,
-0.75560807011887));
#46001=CARTESIAN_POINT('Ctrl Pts',(0.833646445550691,-0.288939216624994,
-0.735904796983946));
#46002=CARTESIAN_POINT('Ctrl Pts',(0.870810080882589,0.141922761093581,
-0.716201523849022));
#46003=CARTESIAN_POINT('Ctrl Pts',(0.698761569148873,0.538687791363206,
-0.696498250714097));
#46004=CARTESIAN_POINT('Ctrl Pts',(0.358835570259291,0.806033064210061,
-0.676794977579174));
#46005=CARTESIAN_POINT('Ctrl Pts',(-0.0673006847419141,0.879728870116488,
-0.657091704444249));
#46006=CARTESIAN_POINT('Ctrl Pts',(-0.477267948291393,0.742069789586453,
-0.637388431309326));
#46007=CARTESIAN_POINT('Ctrl Pts',(-0.772571573488883,0.426128420690425,
-0.617685158174401));
#46008=CARTESIAN_POINT('Ctrl Pts',(-0.846354016015757,0.144756787875129,
-0.604432244356166));
#46009=CARTESIAN_POINT('Ctrl Pts',(-0.846970433828444,0.00250074087411703,
-0.597747088249572));
#46010=CARTESIAN_POINT('Ctrl Pts',(-0.846969994573332,2.57076813976785E-6,
-0.59762968985462));
#46011=CARTESIAN_POINT('Ctrl Pts',(-0.846970387335345,1.65112873682055E-6,
-0.79832031014538));
#46012=CARTESIAN_POINT('Ctrl Pts',(-0.846954510280718,-0.138154651200368,
-0.791827817716009));
#46013=CARTESIAN_POINT('Ctrl Pts',(-0.777569601086075,-0.416084227657901,
-0.778767567574997));
#46014=CARTESIAN_POINT('Ctrl Pts',(-0.487996886622684,-0.73505870214776,
-0.759139559722345));
#46015=CARTESIAN_POINT('Ctrl Pts',(-0.0800725146138843,-0.878658437255334,
-0.739436286587419));
#46016=CARTESIAN_POINT('Ctrl Pts',(0.347089281341945,-0.811160457452224,
-0.719733013452496));
#46017=CARTESIAN_POINT('Ctrl Pts',(0.690862867437646,-0.548781154334267,
-0.700029740317572));
#46018=CARTESIAN_POINT('Ctrl Pts',(0.868656629691441,-0.154557163048435,
-0.680326467182648));
#46019=CARTESIAN_POINT('Ctrl Pts',(0.837755611590708,0.276799191120675,
-0.660623194047723));
#46020=CARTESIAN_POINT('Ctrl Pts',(0.605583783625261,0.641654531633949,
-0.6409199209128));
#46021=CARTESIAN_POINT('Ctrl Pts',(0.227920434166312,0.852352352402625,
-0.621216647777875));
#46022=CARTESIAN_POINT('Ctrl Pts',(-0.204500806181377,0.858272495905586,
-0.601513374642951));
#46023=CARTESIAN_POINT('Ctrl Pts',(-0.587790721937716,0.657992647495812,
-0.581810101508027));
#46024=CARTESIAN_POINT('Ctrl Pts',(-0.805632939903566,0.335501306150746,
-0.564079080008836));
#46025=CARTESIAN_POINT('Ctrl Pts',(-0.846784990265332,0.0978027980064761,
-0.552915816221287));
#46026=CARTESIAN_POINT('Ctrl Pts',(-0.846871433820842,-1.97854529844013E-5,
-0.54832031014538));
#46027=CARTESIAN_POINT('Origin',(0.,0.,-2.22262968985462));
#46028=CARTESIAN_POINT('',(-0.846851569986366,-1.59002605872431E-5,-1.09762968985462));
#46029=CARTESIAN_POINT('',(-0.846863041881276,1.85264865106838E-5,-1.04832031014538));
#46030=CARTESIAN_POINT('',(-0.8469,-1.79235740772804E-14,-2.22262968985462));
#46031=CARTESIAN_POINT('Ctrl Pts',(-0.846851569986366,-1.59002605872524E-5,
-1.09762968985462));
#46032=CARTESIAN_POINT('Ctrl Pts',(-0.846885954129866,-0.050156087623229,
-1.09527436437394));
#46033=CARTESIAN_POINT('Ctrl Pts',(-0.830285463477599,-0.240088244909022,
-1.08635128118162));
#46034=CARTESIAN_POINT('Ctrl Pts',(-0.690037039814528,-0.549819198252638,
-1.07086044027766));
#46035=CARTESIAN_POINT('Ctrl Pts',(-0.345869372375964,-0.811681368725081,
-1.05115716714273));
#46036=CARTESIAN_POINT('Ctrl Pts',(0.0813934217585064,-0.878537066934349,
-1.03145389400781));
#46037=CARTESIAN_POINT('Ctrl Pts',(0.489101443966296,-0.734324209456049,
-1.01175062087288));
#46038=CARTESIAN_POINT('Ctrl Pts',(0.779302830144596,-0.413689939461657,
-0.99204734773796));
#46039=CARTESIAN_POINT('Ctrl Pts',(0.882276688888196,0.00633335042843485,
-0.972344074603035));
#46040=CARTESIAN_POINT('Ctrl Pts',(0.773283547661882,0.424835052695301,
-0.952640801468111));
#46041=CARTESIAN_POINT('Ctrl Pts',(0.478509011791072,0.74127012129041,-0.932937528333187));
#46042=CARTESIAN_POINT('Ctrl Pts',(0.0687726720265907,0.879615021850747,
-0.913234255198264));
#46043=CARTESIAN_POINT('Ctrl Pts',(-0.357486304177214,0.806632388023741,
-0.893530982063338));
#46044=CARTESIAN_POINT('Ctrl Pts',(-0.697859185484572,0.539856299692775,
-0.873827708928416));
#46045=CARTESIAN_POINT('Ctrl Pts',(-0.831977558135312,0.231975349762819,
-0.858527278192175));
#46046=CARTESIAN_POINT('Ctrl Pts',(-0.846897390171971,0.0461033991976785,
-0.849794605167577));
#46047=CARTESIAN_POINT('Ctrl Pts',(-0.846860825277874,1.81094851073073E-5,
-0.84762968985462));
#46048=CARTESIAN_POINT('Ctrl Pts',(-0.846863041881276,1.85264865106838E-5,
-1.04832031014538));
#46049=CARTESIAN_POINT('Ctrl Pts',(-0.846785938008928,-0.0946024683408287,
-1.04387533463401));
#46050=CARTESIAN_POINT('Ctrl Pts',(-0.80757060413725,-0.329094830876242,
-1.03286260141101));
#46051=CARTESIAN_POINT('Ctrl Pts',(-0.595220747044056,-0.651279140802846,
-1.01528211047636));
#46052=CARTESIAN_POINT('Ctrl Pts',(-0.214228592898141,-0.855896236083242,
-0.995578837341434));
#46053=CARTESIAN_POINT('Ctrl Pts',(0.218231986874677,-0.854884235941514,
-0.975875564206509));
#46054=CARTESIAN_POINT('Ctrl Pts',(0.598262325502182,-0.648486273440926,
-0.956172291071585));
#46055=CARTESIAN_POINT('Ctrl Pts',(0.834560123160567,-0.286289465029356,
-0.936469017936662));
#46056=CARTESIAN_POINT('Ctrl Pts',(0.870354827142315,0.144688395618483,
-0.916765744801736));
#46057=CARTESIAN_POINT('Ctrl Pts',(0.697046758782688,0.540904865042945,
-0.897062471666814));
#46058=CARTESIAN_POINT('Ctrl Pts',(0.356273186507159,0.807168925029088,
-0.877359198531888));
#46059=CARTESIAN_POINT('Ctrl Pts',(-0.0700950291095755,0.879510627480251,
-0.857655925396965));
#46060=CARTESIAN_POINT('Ctrl Pts',(-0.479622911959631,0.740549876294596,
-0.83795265226204));
#46061=CARTESIAN_POINT('Ctrl Pts',(-0.77392137636837,0.423671995955202,
-0.818249379127117));
#46062=CARTESIAN_POINT('Ctrl Pts',(-0.846577873754564,0.142962661529076,
-0.805038598421563));
#46063=CARTESIAN_POINT('Ctrl Pts',(-0.846970571392702,0.00160325070015155,
-0.798395575427651));
#46064=CARTESIAN_POINT('Ctrl Pts',(-0.846970387335345,1.65112873682055E-6,
-0.79832031014538));
#46065=CARTESIAN_POINT('Origin',(0.,0.,-2.22262968985462));
#46066=CARTESIAN_POINT('',(-0.846966250199675,-6.62394975969204E-6,-1.34762968985462));
#46067=CARTESIAN_POINT('',(-0.846849704405232,-1.53444222700805E-5,-1.29832031014538));
#46068=CARTESIAN_POINT('',(-0.8469,-1.79235740772804E-14,-2.22262968985462));
#46069=CARTESIAN_POINT('Ctrl Pts',(-0.846966250199675,-6.62394975969871E-6,
-1.34762968985462));
#46070=CARTESIAN_POINT('Ctrl Pts',(-0.846969009911585,-0.00655669690887438,
-1.34732188129194));
#46071=CARTESIAN_POINT('Ctrl Pts',(-0.845306643333083,-0.152865259786774,
-1.34044631501763));
#46072=CARTESIAN_POINT('Ctrl Pts',(-0.766374416668415,-0.437175617499231,
-1.32700299103167));
#46073=CARTESIAN_POINT('Ctrl Pts',(-0.466565539319551,-0.748845020430254,
-1.30729971789674));
#46074=CARTESIAN_POINT('Ctrl Pts',(-0.0546642776836284,-0.880604385530872,
-1.28759644476182));
#46075=CARTESIAN_POINT('Ctrl Pts',(0.37037007824383,-0.800798521621077,
-1.2678931716269));
#46076=CARTESIAN_POINT('Ctrl Pts',(0.706423012183327,-0.52860078976397,
-1.24818989849197));
#46077=CARTESIAN_POINT('Ctrl Pts',(0.872757797056872,-0.129406702917007,
-1.22848662535705));
#46078=CARTESIAN_POINT('Ctrl Pts',(0.829412495997682,0.300877348044562,
-1.20878335222212));
#46079=CARTESIAN_POINT('Ctrl Pts',(0.586800818836326,0.658875607452487,
-1.1890800790872));
#46080=CARTESIAN_POINT('Ctrl Pts',(0.20321022801312,0.858578983154271,-1.16937680595228));
#46081=CARTESIAN_POINT('Ctrl Pts',(-0.229201625955346,0.852008733372195,
-1.14967353281735));
#46082=CARTESIAN_POINT('Ctrl Pts',(-0.606547782672759,0.640743360806779,
-1.12997025968243));
#46083=CARTESIAN_POINT('Ctrl Pts',(-0.810482644113683,0.319195791254851,
-1.11262231202818));
#46084=CARTESIAN_POINT('Ctrl Pts',(-0.846790074929525,0.0896583902123634,
-1.10184212208558));
#46085=CARTESIAN_POINT('Ctrl Pts',(-0.846851569986366,-1.59002605872524E-5,
-1.09762968985462));
#46086=CARTESIAN_POINT('Ctrl Pts',(-0.846849704405232,-1.53444222701221E-5,
-1.29832031014538));
#46087=CARTESIAN_POINT('Ctrl Pts',(-0.84688337735639,-0.0510527828440758,
-1.29592285155202));
#46088=CARTESIAN_POINT('Ctrl Pts',(-0.829902698745262,-0.241883433963255,
-1.28695763524702));
#46089=CARTESIAN_POINT('Ctrl Pts',(-0.688286911759098,-0.552008499986543,
-1.27142466123037));
#46090=CARTESIAN_POINT('Ctrl Pts',(-0.343289110846343,-0.812776010553405,
-1.25172138809545));
#46091=CARTESIAN_POINT('Ctrl Pts',(0.0841839088554315,-0.878274061125737,
-1.23201811496052));
#46092=CARTESIAN_POINT('Ctrl Pts',(0.49143174202491,-0.732766743163866,
-1.2123148418256));
#46093=CARTESIAN_POINT('Ctrl Pts',(0.78061308498908,-0.411212194007425,
-1.19261156869067));
#46094=CARTESIAN_POINT('Ctrl Pts',(0.882252111754334,0.00913609662776034,
-1.17290829555575));
#46095=CARTESIAN_POINT('Ctrl Pts',(0.771930043206802,0.42728943978447,-1.15320502242083));
#46096=CARTESIAN_POINT('Ctrl Pts',(0.476151759499167,0.742786482700393,
-1.1335017492859));
#46097=CARTESIAN_POINT('Ctrl Pts',(0.0659780018290307,0.879829051709039,
-1.11379847615098));
#46098=CARTESIAN_POINT('Ctrl Pts',(-0.360046972684807,0.805492665650708,
-1.09409520301605));
#46099=CARTESIAN_POINT('Ctrl Pts',(-0.699570651619342,0.537636643421434,
-1.07439192988113));
#46100=CARTESIAN_POINT('Ctrl Pts',(-0.832343654483411,0.230180174733228,
-1.05913363225757));
#46101=CARTESIAN_POINT('Ctrl Pts',(-0.846899864295118,0.0452065737723092,
-1.05044309234566));
#46102=CARTESIAN_POINT('Ctrl Pts',(-0.846863041881276,1.85264865106838E-5,
-1.04832031014538));
#46103=CARTESIAN_POINT('Origin',(0.,0.,-2.22262968985462));
#46104=CARTESIAN_POINT('',(-0.84688555437138,2.10899746275484E-5,-1.59762968985462));
#46105=CARTESIAN_POINT('',(-0.846965023971566,-7.48627396990331E-6,-1.54832031014538));
#46106=CARTESIAN_POINT('',(-0.8469,-1.79235740772804E-14,-2.22262968985462));
#46107=CARTESIAN_POINT('Ctrl Pts',(-0.846885554371379,2.10899746275542E-5,
-1.59762968985462));
#46108=CARTESIAN_POINT('Ctrl Pts',(-0.846786579154185,-0.10274664313416,
-1.59280164049831));
#46109=CARTESIAN_POINT('Ctrl Pts',(-0.802557679176094,-0.345395880262735,
-1.58140583343035));
#46110=CARTESIAN_POINT('Ctrl Pts',(-0.576164155731512,-0.668196828584006,
-1.56344226865076));
#46111=CARTESIAN_POINT('Ctrl Pts',(-0.189421752756959,-0.861726031055052,
-1.54373899551583));
#46112=CARTESIAN_POINT('Ctrl Pts',(0.242829229569888,-0.848225317583151,
-1.52403572238091));
#46113=CARTESIAN_POINT('Ctrl Pts',(0.616740483602872,-0.630938554242118,
-1.50433244924599));
#46114=CARTESIAN_POINT('Ctrl Pts',(0.842479818084434,-0.262068730894017,
-1.48462917611106));
#46115=CARTESIAN_POINT('Ctrl Pts',(0.865813352240911,0.169763085262774,
-1.46492590297614));
#46116=CARTESIAN_POINT('Ctrl Pts',(0.681135203387868,0.560809329104389,
-1.44522262984121));
#46117=CARTESIAN_POINT('Ctrl Pts',(0.332814302334667,0.81712110846086,-1.42551935670629));
#46118=CARTESIAN_POINT('Ctrl Pts',(-0.0954652444970479,0.877119521452837,
-1.40581608357137));
#46119=CARTESIAN_POINT('Ctrl Pts',(-0.500809263564396,0.726389942318086,
-1.38611281043644));
#46120=CARTESIAN_POINT('Ctrl Pts',(-0.781381130347438,0.406226199993855,
-1.36671734586419));
#46121=CARTESIAN_POINT('Ctrl Pts',(-0.846910125522463,0.133203197406965,
-1.35388963900359));
#46122=CARTESIAN_POINT('Ctrl Pts',(-0.846966250199675,-6.62394975969871E-6,
-1.34762968985462));
#46123=CARTESIAN_POINT('Ctrl Pts',(-0.846965023971566,-7.48627396995969E-6,
-1.54832031014538));
#46124=CARTESIAN_POINT('Ctrl Pts',(-0.846968518185878,-0.00745417022599956,
-1.54797036847002));
#46125=CARTESIAN_POINT('Ctrl Pts',(-0.845066969761898,-0.154659544089421,
-1.54105266908302));
#46126=CARTESIAN_POINT('Ctrl Pts',(-0.764981744407948,-0.439607995293088,
-1.52756721198439));
#46127=CARTESIAN_POINT('Ctrl Pts',(-0.464184283631377,-0.75032340121505,
-1.50786393884946));
#46128=CARTESIAN_POINT('Ctrl Pts',(-0.05186653586545,-0.880773591887012,
-1.48816066571454));
#46129=CARTESIAN_POINT('Ctrl Pts',(0.372912148917511,-0.799617899892882,
-1.46845739257961));
#46130=CARTESIAN_POINT('Ctrl Pts',(0.708098679019178,-0.526353985277906,
-1.44875411944469));
#46131=CARTESIAN_POINT('Ctrl Pts',(0.87316448112032,-0.126633510049379,
-1.42905084630976));
#46132=CARTESIAN_POINT('Ctrl Pts',(0.828452491394789,0.303510669391465,
-1.40934757317484));
#46133=CARTESIAN_POINT('Ctrl Pts',(0.584704766718826,0.660736401868303,
-1.38964430003992));
#46134=CARTESIAN_POINT('Ctrl Pts',(0.200481704953546,0.859220194666598,
-1.36994102690499));
#46135=CARTESIAN_POINT('Ctrl Pts',(-0.231907092208531,0.851276310927182,
-1.35023775377007));
#46136=CARTESIAN_POINT('Ctrl Pts',(-0.608580203776492,0.638813268902558,
-1.33053448063514));
#46137=CARTESIAN_POINT('Ctrl Pts',(-0.810999741514778,0.317401987448,-1.31322866609358));
#46138=CARTESIAN_POINT('Ctrl Pts',(-0.846791131431787,0.0887625744285762,
-1.30249060926366));
#46139=CARTESIAN_POINT('Ctrl Pts',(-0.846849704405232,-1.53444222701221E-5,
-1.29832031014538));
#46140=CARTESIAN_POINT('Origin',(9.02152032747242E-17,0.,-0.0695250000000002));
#46141=CARTESIAN_POINT('',(0.924091453827287,-0.353856906938908,-0.0695250000000001));
#46142=CARTESIAN_POINT('Ctrl Pts',(-0.644274518039098,-0.549718620818717,
-0.0695250000000001));
#46143=CARTESIAN_POINT('Ctrl Pts',(-0.629514607897228,-0.570212568079803,
-0.0695250000000002));
#46144=CARTESIAN_POINT('Ctrl Pts',(-0.613856197663174,-0.590011328072283,
-0.0695250000000003));
#46145=CARTESIAN_POINT('Ctrl Pts',(-0.597342646439648,-0.609050847410868,
-0.0695250000000002));
#46146=CARTESIAN_POINT('Ctrl Pts',(-0.573764312529119,-0.636235802263072,
-0.069525));
#46147=CARTESIAN_POINT('Ctrl Pts',(-0.548443954816583,-0.661874145350851,
-0.0695250000000003));
#46148=CARTESIAN_POINT('Ctrl Pts',(-0.521577921430738,-0.685866619007268,
-0.0695250000000004));
#46149=CARTESIAN_POINT('Ctrl Pts',(-0.513406905541179,-0.693163672526888,
-0.0695250000000004));
#46150=CARTESIAN_POINT('Ctrl Pts',(-0.505092690910161,-0.700308333369332,
-0.0695250000000004));
#46151=CARTESIAN_POINT('Ctrl Pts',(-0.496640257082355,-0.707297384869979,
-0.0695250000000004));
#46152=CARTESIAN_POINT('Ctrl Pts',(-0.489314977156243,-0.713354428285312,
-0.0695250000000004));
#46153=CARTESIAN_POINT('Ctrl Pts',(-0.481887585227203,-0.719293024959345,
-0.069525));
#46154=CARTESIAN_POINT('Ctrl Pts',(-0.474370457275395,-0.72510452921095,
-0.0695249999999999));
#46155=CARTESIAN_POINT('Ctrl Pts',(-0.442888567313103,-0.749443231244141,
-0.0695249999999998));
#46156=CARTESIAN_POINT('Ctrl Pts',(-0.409793969953919,-0.771590511960091,
-0.0695250000000001));
#46157=CARTESIAN_POINT('Ctrl Pts',(-0.375343642665579,-0.791414612519383,
-0.0695250000000003));
#46158=CARTESIAN_POINT('Ctrl Pts',(-0.350727952172436,-0.80557946847527,
-0.0695250000000005));
#46159=CARTESIAN_POINT('Ctrl Pts',(-0.325419068593534,-0.818557693233704,
-0.0695250000000005));
#46160=CARTESIAN_POINT('Ctrl Pts',(-0.299499852848171,-0.830289403880256,
-0.0695250000000005));
#46161=CARTESIAN_POINT('Ctrl Pts',(-0.291030362789716,-0.834122915189619,
-0.0695250000000005));
#46162=CARTESIAN_POINT('Ctrl Pts',(-0.282504034872275,-0.837819395972558,
-0.0695249999999998));
#46163=CARTESIAN_POINT('Ctrl Pts',(-0.273927638577144,-0.84137590496099,
-0.0695249999999998));
#46164=CARTESIAN_POINT('Ctrl Pts',(-0.264547191210553,-0.845265842439012,
-0.0695249999999998));
#46165=CARTESIAN_POINT('Ctrl Pts',(-0.255105521084919,-0.848988937674037,
-0.069525));
#46166=CARTESIAN_POINT('Ctrl Pts',(-0.245606840153278,-0.852543254107393,
-0.069525));
#46167=CARTESIAN_POINT('Ctrl Pts',(-0.207900418576629,-0.86665263990711,
-0.069525));
#46168=CARTESIAN_POINT('Ctrl Pts',(-0.169298093448506,-0.878105947076264,
-0.0695249999999999));
#46169=CARTESIAN_POINT('Ctrl Pts',(-0.130091573045686,-0.88693130443109,
-0.0695249999999997));
#46170=CARTESIAN_POINT('Ctrl Pts',(-0.102099247085215,-0.893232355308744,
-0.0695249999999996));
#46171=CARTESIAN_POINT('Ctrl Pts',(-0.073798080309421,-0.898192899460623,
-0.0695249999999996));
#46172=CARTESIAN_POINT('Ctrl Pts',(-0.0452868955746615,-0.90180864777946,
-0.0695249999999996));
#46173=CARTESIAN_POINT('Ctrl Pts',(-0.0239859768418001,-0.904510000312319,
-0.0695249999999995));
#46174=CARTESIAN_POINT('Ctrl Pts',(-0.00256769535849218,-0.906460483102193,
-0.0695249999999999));
#46175=CARTESIAN_POINT('Ctrl Pts',(0.0189277734581549,-0.907653646015335,
-0.0695249999999999));
#46176=CARTESIAN_POINT('Ctrl Pts',(0.026864202214143,-0.908094178507797,
-0.0695249999999999));
#46177=CARTESIAN_POINT('Ctrl Pts',(0.0348136815882982,-0.908431500832323,
-0.0695249999999997));
#46178=CARTESIAN_POINT('Ctrl Pts',(0.042765812934101,-0.908664920818656,
-0.0695249999999997));
#46179=CARTESIAN_POINT('Ctrl Pts',(0.0842470804049054,-0.909882526070012,
-0.0695249999999998));
#46180=CARTESIAN_POINT('Ctrl Pts',(0.125677974715032,-0.908275201452815,
-0.0695250000000009));
#46181=CARTESIAN_POINT('Ctrl Pts',(0.166763121040939,-0.903860943778449,
-0.0695250000000008));
#46182=CARTESIAN_POINT('Ctrl Pts',(0.176627678125244,-0.902801079065587,
-0.0695250000000008));
#46183=CARTESIAN_POINT('Ctrl Pts',(0.186472385882437,-0.901579177917462,
-0.0695250000000002));
#46184=CARTESIAN_POINT('Ctrl Pts',(0.196293280785995,-0.900195063374112,
-0.0695250000000002));
#46185=CARTESIAN_POINT('Ctrl Pts',(0.234668994651919,-0.89478655588117,
-0.0695250000000001));
#46186=CARTESIAN_POINT('Ctrl Pts',(0.272681208109324,-0.886904450937793,
-0.0695250000000005));
#46187=CARTESIAN_POINT('Ctrl Pts',(0.310125123955116,-0.876660725787972,
-0.0695250000000006));
#46188=CARTESIAN_POINT('Ctrl Pts',(0.329782155791864,-0.871283050220432,
-0.0695250000000006));
#46189=CARTESIAN_POINT('Ctrl Pts',(0.349282561029609,-0.865253829412173,
-0.0695250000000006));
#46190=CARTESIAN_POINT('Ctrl Pts',(0.36859600834363,-0.858584870376398,
-0.0695250000000006));
#46191=CARTESIAN_POINT('Ctrl Pts',(0.376732359496032,-0.855775377505767,
-0.0695250000000006));
#46192=CARTESIAN_POINT('Ctrl Pts',(0.384837496765632,-0.852851562967871,
-0.0695250000000003));
#46193=CARTESIAN_POINT('Ctrl Pts',(0.392902786498845,-0.849816543883558,
-0.0695250000000003));
#46194=CARTESIAN_POINT('Ctrl Pts',(0.433999942212729,-0.834351426568682,
-0.0695250000000003));
#46195=CARTESIAN_POINT('Ctrl Pts',(0.473890548978183,-0.81607027944879,
-0.0695250000000002));
#46196=CARTESIAN_POINT('Ctrl Pts',(0.51229280876073,-0.795158465405007,
-0.0695250000000002));
#46197=CARTESIAN_POINT('Ctrl Pts',(0.550695068543278,-0.774246651361224,
-0.0695250000000001));
#46198=CARTESIAN_POINT('Ctrl Pts',(0.5876103412066,-0.750703718346156,-0.0695250000000004));
#46199=CARTESIAN_POINT('Ctrl Pts',(0.622745109445882,-0.724656753629564,
-0.0695250000000004));
#46200=CARTESIAN_POINT('Ctrl Pts',(0.638877111365698,-0.712697383869337,
-0.0695250000000005));
#46201=CARTESIAN_POINT('Ctrl Pts',(0.654633463274635,-0.700209354343849,
-0.0695250000000005));
#46202=CARTESIAN_POINT('Ctrl Pts',(0.669996947566329,-0.687216016520921,
-0.0695250000000005));
#46203=CARTESIAN_POINT('Ctrl Pts',(0.678922789820835,-0.679667176585591,
-0.0695250000000005));
#46204=CARTESIAN_POINT('Ctrl Pts',(0.68771599710606,-0.671947736058525,
-0.0695250000000001));
#46205=CARTESIAN_POINT('Ctrl Pts',(0.696372929515829,-0.66406195754111,
-0.0695250000000001));
#46206=CARTESIAN_POINT('Ctrl Pts',(0.702557911261651,-0.658427929934892,
-0.0695250000000001));
#46207=CARTESIAN_POINT('Ctrl Pts',(0.708673069158198,-0.652709060668137,
-0.0695250000000001));
#46208=CARTESIAN_POINT('Ctrl Pts',(0.714707061246942,-0.646916923963097,
-0.0695250000000001));
#46209=CARTESIAN_POINT('Ctrl Pts',(0.745695686752405,-0.617170389233001,
-0.0695250000000001));
#46210=CARTESIAN_POINT('Ctrl Pts',(0.77461545607891,-0.585432521388643,
-0.069525));
#46211=CARTESIAN_POINT('Ctrl Pts',(0.801330866406532,-0.551969355975223,
-0.069525));
#46212=CARTESIAN_POINT('Ctrl Pts',(0.828287682902432,-0.518203810233675,
-0.069525));
#46213=CARTESIAN_POINT('Ctrl Pts',(0.853000960044775,-0.48268086089206,
-0.0695249999999999));
#46214=CARTESIAN_POINT('Ctrl Pts',(0.875301042068569,-0.445631041576752,
-0.0695249999999999));
#46215=CARTESIAN_POINT('Ctrl Pts',(0.893145601953607,-0.41598371925765,
-0.0695249999999999));
#46216=CARTESIAN_POINT('Ctrl Pts',(0.909444522886281,-0.385357711644212,
-0.069525));
#46217=CARTESIAN_POINT('Ctrl Pts',(0.924091453827287,-0.353856906938908,
-0.0695250000000001));
#46218=CARTESIAN_POINT('',(-0.989525,-1.21181862392629E-16,-0.0695250000000003));
#46219=CARTESIAN_POINT('Origin',(0.,0.,-0.0695250000000001));
#46220=CARTESIAN_POINT('',(0.849186560444991,0.508032827447782,-0.0695250000000002));
#46221=CARTESIAN_POINT('Origin',(0.,0.,-0.0695250000000001));
#46222=CARTESIAN_POINT('Ctrl Pts',(0.849186560444991,0.508032827447782,
-0.0695250000000002));
#46223=CARTESIAN_POINT('Ctrl Pts',(0.832465613029651,0.532075780979081,
-0.0695250000000002));
#46224=CARTESIAN_POINT('Ctrl Pts',(0.814699598175689,0.555333492117173,
-0.0695249999999997));
#46225=CARTESIAN_POINT('Ctrl Pts',(0.795920427116913,0.577725594506868,
-0.0695249999999998));
#46226=CARTESIAN_POINT('Ctrl Pts',(0.770244398979351,0.60834144273667,-0.0695249999999999));
#46227=CARTESIAN_POINT('Ctrl Pts',(0.742674876881569,0.637340509727314,
-0.0695250000000005));
#46228=CARTESIAN_POINT('Ctrl Pts',(0.713391010537452,0.66457844663845,-0.0695250000000007));
#46229=CARTESIAN_POINT('Ctrl Pts',(0.703372076901965,0.67389740333199,-0.0695250000000007));
#46230=CARTESIAN_POINT('Ctrl Pts',(0.693152303997172,0.683009942300558,
-0.0695250000000002));
#46231=CARTESIAN_POINT('Ctrl Pts',(0.68273841510423,0.691909392025286,-0.0695250000000002));
#46232=CARTESIAN_POINT('Ctrl Pts',(0.675105784312335,0.698432047941648,
-0.0695250000000002));
#46233=CARTESIAN_POINT('Ctrl Pts',(0.667370342782135,0.704838817597991,
-0.0695250000000004));
#46234=CARTESIAN_POINT('Ctrl Pts',(0.659543833079429,0.711120248251889,
-0.0695250000000004));
#46235=CARTESIAN_POINT('Ctrl Pts',(0.626058981692227,0.737994650754968,
-0.0695250000000004));
#46236=CARTESIAN_POINT('Ctrl Pts',(0.590864886279207,0.762616605548979,
-0.069525));
#46237=CARTESIAN_POINT('Ctrl Pts',(0.554186287487196,0.784804033106952,
-0.069525));
#46238=CARTESIAN_POINT('Ctrl Pts',(0.529103291209082,0.799977108992796,
-0.069525));
#46239=CARTESIAN_POINT('Ctrl Pts',(0.503325419420093,0.814010769328655,
-0.0695250000000002));
#46240=CARTESIAN_POINT('Ctrl Pts',(0.47692006115639,0.826833197390815,-0.0695250000000003));
#46241=CARTESIAN_POINT('Ctrl Pts',(0.46840181479615,0.830969653335822,-0.0695250000000004));
#46242=CARTESIAN_POINT('Ctrl Pts',(0.459816463861541,0.834980640477273,
-0.0695249999999996));
#46243=CARTESIAN_POINT('Ctrl Pts',(0.451182152464372,0.838856712876695,
-0.0695249999999997));
#46244=CARTESIAN_POINT('Ctrl Pts',(0.437905879500253,0.844816631720981,
-0.0695249999999997));
#46245=CARTESIAN_POINT('Ctrl Pts',(0.424506188175036,0.8504615084049,-0.069525));
#46246=CARTESIAN_POINT('Ctrl Pts',(0.410992010006838,0.85578480548222,-0.069525));
#46247=CARTESIAN_POINT('Ctrl Pts',(0.371777648040439,0.871231523428853,
-0.0695250000000001));
#46248=CARTESIAN_POINT('Ctrl Pts',(0.331600099063284,0.883974369710503,
-0.0695249999999996));
#46249=CARTESIAN_POINT('Ctrl Pts',(0.290745866776486,0.893985042687368,
-0.0695249999999996));
#46250=CARTESIAN_POINT('Ctrl Pts',(0.25024980796209,0.903907951011698,-0.0695249999999996));
#46251=CARTESIAN_POINT('Ctrl Pts',(0.209087691304592,0.911146366027076,
-0.0695250000000002));
#46252=CARTESIAN_POINT('Ctrl Pts',(0.167537654230177,0.915622168647208,
-0.0695250000000004));
#46253=CARTESIAN_POINT('Ctrl Pts',(0.149988630342492,0.917512563280469,
-0.0695250000000005));
#46254=CARTESIAN_POINT('Ctrl Pts',(0.132370498081357,0.918909523988645,
-0.0695250000000004));
#46255=CARTESIAN_POINT('Ctrl Pts',(0.114704940581103,0.919804424450112,
-0.0695250000000005));
#46256=CARTESIAN_POINT('Ctrl Pts',(0.106506859464303,0.920219722216654,
-0.0695250000000005));
#46257=CARTESIAN_POINT('Ctrl Pts',(0.0983079054751423,0.920526381597904,
-0.069525));
#46258=CARTESIAN_POINT('Ctrl Pts',(0.0901122544371284,0.920724168836828,
-0.069525));
#46259=CARTESIAN_POINT('Ctrl Pts',(0.0489897278813967,0.921716586760351,
-0.0695250000000002));
#46260=CARTESIAN_POINT('Ctrl Pts',(0.00793295039935812,0.919973010373648,
-0.0695249999999997));
#46261=CARTESIAN_POINT('Ctrl Pts',(-0.0327910898782061,0.915446284625334,
-0.0695249999999998));
#46262=CARTESIAN_POINT('Ctrl Pts',(-0.0363378459041664,0.915052041035644,
-0.0695249999999998));
#46263=CARTESIAN_POINT('Ctrl Pts',(-0.0398820734162914,0.914636654549671,
-0.0695250000000006));
#46264=CARTESIAN_POINT('Ctrl Pts',(-0.0434235925645807,0.914200075428631,
-0.0695250000000006));
#46265=CARTESIAN_POINT('Ctrl Pts',(-0.0802746321872905,0.909657280708554,
-0.0695250000000005));
#46266=CARTESIAN_POINT('Ctrl Pts',(-0.116833648576168,0.902822475100424,
-0.0695250000000003));
#46267=CARTESIAN_POINT('Ctrl Pts',(-0.152895642013777,0.89375708945521,
-0.0695250000000002));
#46268=CARTESIAN_POINT('Ctrl Pts',(-0.171831220409218,0.888996999837124,
-0.0695250000000002));
#46269=CARTESIAN_POINT('Ctrl Pts',(-0.190629523232773,0.883621386847789,
-0.069525));
#46270=CARTESIAN_POINT('Ctrl Pts',(-0.209258732975253,0.877635930874417,
-0.069525));
#46271=CARTESIAN_POINT('Ctrl Pts',(-0.217624297379082,0.874948124031094,
-0.069525));
#46272=CARTESIAN_POINT('Ctrl Pts',(-0.225955740196051,0.872137313528728,
-0.0695250000000003));
#46273=CARTESIAN_POINT('Ctrl Pts',(-0.234250054208824,0.869203882116388,
-0.0695250000000003));
#46274=CARTESIAN_POINT('Ctrl Pts',(-0.241741121075245,0.866554533318638,
-0.0695250000000003));
#46275=CARTESIAN_POINT('Ctrl Pts',(-0.249193176417347,0.863808233930807,
-0.069525));
#46276=CARTESIAN_POINT('Ctrl Pts',(-0.256602800192705,0.860966475101326,
-0.069525));
#46277=CARTESIAN_POINT('Ctrl Pts',(-0.294124992514654,0.846575863031793,
-0.069525));
#46278=CARTESIAN_POINT('Ctrl Pts',(-0.330574092810289,0.829736301930517,
-0.0695250000000004));
#46279=CARTESIAN_POINT('Ctrl Pts',(-0.365695559063158,0.810541946680565,
-0.0695250000000003));
#46280=CARTESIAN_POINT('Ctrl Pts',(-0.396561761353498,0.793673150608326,
-0.0695250000000002));
#46281=CARTESIAN_POINT('Ctrl Pts',(-0.426402744048706,0.774984657826367,
-0.0695250000000004));
#46282=CARTESIAN_POINT('Ctrl Pts',(-0.455025122704759,0.754514235939637,
-0.0695250000000004));
#46283=CARTESIAN_POINT('Ctrl Pts',(-0.469941989788981,0.743845850683762,
-0.0695250000000004));
#46284=CARTESIAN_POINT('Ctrl Pts',(-0.484527482772804,0.732693076977225,
-0.0695250000000004));
#46285=CARTESIAN_POINT('Ctrl Pts',(-0.498760924054214,0.721074151458354,
-0.0695250000000004));
#46286=CARTESIAN_POINT('Ctrl Pts',(-0.50875747684214,0.712913847847161,
-0.0695250000000004));
#46287=CARTESIAN_POINT('Ctrl Pts',(-0.518580335702014,0.704523581635438,
-0.0695250000000002));
#46288=CARTESIAN_POINT('Ctrl Pts',(-0.528221721630384,0.695909387857388,
-0.0695250000000001));
#46289=CARTESIAN_POINT('Ctrl Pts',(-0.534327024836865,0.690454542953854,
-0.0695250000000001));
#46290=CARTESIAN_POINT('Ctrl Pts',(-0.540353017486882,0.684915689319018,
-0.0695250000000007));
#46291=CARTESIAN_POINT('Ctrl Pts',(-0.546295490452486,0.679297484790217,
-0.0695250000000007));
#46292=CARTESIAN_POINT('Ctrl Pts',(-0.574958072746145,0.652198960222842,
-0.0695250000000006));
#46293=CARTESIAN_POINT('Ctrl Pts',(-0.601702485869931,0.623237707774714,
-0.0695250000000003));
#46294=CARTESIAN_POINT('Ctrl Pts',(-0.626357124444992,0.59262560076324,
-0.0695250000000003));
#46295=CARTESIAN_POINT('Ctrl Pts',(-0.650560797781831,0.562573428795588,
-0.0695250000000002));
#46296=CARTESIAN_POINT('Ctrl Pts',(-0.672750955666676,0.530929222698942,
-0.0695250000000002));
#46297=CARTESIAN_POINT('Ctrl Pts',(-0.692721855863329,0.497870363939758,
-0.0695250000000001));
#46298=CARTESIAN_POINT('Ctrl Pts',(-0.705966728863737,0.475945444106792,
-0.069525));
#46299=CARTESIAN_POINT('Ctrl Pts',(-0.718234573055067,0.453397852226439,
-0.0695250000000001));
#46300=CARTESIAN_POINT('Ctrl Pts',(-0.729452881030877,0.430276776454125,
-0.0695250000000001));
#46301=CARTESIAN_POINT('Ctrl Pts',(-0.370207279419763,0.761699534110805,
-1.84281958214317));
#46302=CARTESIAN_POINT('Ctrl Pts',(-0.495937788115843,0.700590990019629,
-1.83625182443153));
#46303=CARTESIAN_POINT('Ctrl Pts',(-0.716438090811261,0.514985758881006,
-1.82311630900825));
#46304=CARTESIAN_POINT('Ctrl Pts',(-0.875085689900816,0.112597606289335,
-1.80341303587332));
#46305=CARTESIAN_POINT('Ctrl Pts',(-0.823479197849261,-0.316739409883142,
-1.7837097627384));
#46306=CARTESIAN_POINT('Ctrl Pts',(-0.574039462429418,-0.670029803239366,
-1.76400648960348));
#46307=CARTESIAN_POINT('Ctrl Pts',(-0.186682838485098,-0.862320382256737,
-1.74430321646855));
#46308=CARTESIAN_POINT('Ctrl Pts',(0.2455223736064,-0.847451160704884,-1.72459994333363));
#46309=CARTESIAN_POINT('Ctrl Pts',(0.618741824242655,-0.628975354430863,
-1.7048966701987));
#46310=CARTESIAN_POINT('Ctrl Pts',(0.843308030144031,-0.259391446847321,
-1.68519339706378));
#46311=CARTESIAN_POINT('Ctrl Pts',(0.865269712120719,0.172512904594376,
-1.66549012392885));
#46312=CARTESIAN_POINT('Ctrl Pts',(0.679350192014294,0.562970195790566,
-1.64578685079393));
#46313=CARTESIAN_POINT('Ctrl Pts',(0.330216833785133,0.818174300873478,
-1.626083577659));
#46314=CARTESIAN_POINT('Ctrl Pts',(-0.0982511612190419,0.876811794340843,
-1.60638030452408));
#46315=CARTESIAN_POINT('Ctrl Pts',(-0.503114295254248,0.724795336222326,
-1.58667703138916));
#46316=CARTESIAN_POINT('Ctrl Pts',(-0.78710421375316,0.398646723393102,
-1.56697375825423));
#46317=CARTESIAN_POINT('Ctrl Pts',(-0.88199231792273,-0.023276748797502,
-1.54727048511931));
#46318=CARTESIAN_POINT('Ctrl Pts',(-0.764981744407948,-0.439607995293088,
-1.52756721198439));
#46319=CARTESIAN_POINT('Ctrl Pts',(-0.464184283631377,-0.75032340121505,
-1.50786393884946));
#46320=CARTESIAN_POINT('Ctrl Pts',(-0.05186653586545,-0.880773591887012,
-1.48816066571454));
#46321=CARTESIAN_POINT('Ctrl Pts',(0.372912148917511,-0.799617899892882,
-1.46845739257961));
#46322=CARTESIAN_POINT('Ctrl Pts',(0.708098679019178,-0.526353985277906,
-1.44875411944469));
#46323=CARTESIAN_POINT('Ctrl Pts',(0.87316448112032,-0.126633510049379,
-1.42905084630976));
#46324=CARTESIAN_POINT('Ctrl Pts',(0.828452491394789,0.303510669391465,
-1.40934757317484));
#46325=CARTESIAN_POINT('Ctrl Pts',(0.584704766718826,0.660736401868303,
-1.38964430003992));
#46326=CARTESIAN_POINT('Ctrl Pts',(0.200481704953546,0.859220194666598,
-1.36994102690499));
#46327=CARTESIAN_POINT('Ctrl Pts',(-0.231907092208531,0.851276310927182,
-1.35023775377007));
#46328=CARTESIAN_POINT('Ctrl Pts',(-0.608580203776492,0.638813268902558,
-1.33053448063514));
#46329=CARTESIAN_POINT('Ctrl Pts',(-0.839041903820945,0.272875320594155,
-1.31083120750022));
#46330=CARTESIAN_POINT('Ctrl Pts',(-0.867923762256349,-0.158620931366679,
-1.29112793436529));
#46331=CARTESIAN_POINT('Ctrl Pts',(-0.688286911759098,-0.552008499986543,
-1.27142466123037));
#46332=CARTESIAN_POINT('Ctrl Pts',(-0.343289110846343,-0.812776010553405,
-1.25172138809545));
#46333=CARTESIAN_POINT('Ctrl Pts',(0.0841839088554315,-0.878274061125737,
-1.23201811496052));
#46334=CARTESIAN_POINT('Ctrl Pts',(0.49143174202491,-0.732766743163866,
-1.2123148418256));
#46335=CARTESIAN_POINT('Ctrl Pts',(0.78061308498908,-0.411212194007425,
-1.19261156869067));
#46336=CARTESIAN_POINT('Ctrl Pts',(0.882252111754334,0.00913609662776034,
-1.17290829555575));
#46337=CARTESIAN_POINT('Ctrl Pts',(0.771930043206802,0.42728943978447,-1.15320502242083));
#46338=CARTESIAN_POINT('Ctrl Pts',(0.476151759499167,0.742786482700393,
-1.1335017492859));
#46339=CARTESIAN_POINT('Ctrl Pts',(0.0659780018290307,0.879829051709039,
-1.11379847615098));
#46340=CARTESIAN_POINT('Ctrl Pts',(-0.360046972684807,0.805492665650708,
-1.09409520301605));
#46341=CARTESIAN_POINT('Ctrl Pts',(-0.699570651619342,0.537636643421434,
-1.07439192988113));
#46342=CARTESIAN_POINT('Ctrl Pts',(-0.871022461311121,0.140613402092739,
-1.05468865674621));
#46343=CARTESIAN_POINT('Ctrl Pts',(-0.833211099533203,-0.290192213147162,
-1.03498538361128));
#46344=CARTESIAN_POINT('Ctrl Pts',(-0.595220747044056,-0.651279140802846,
-1.01528211047636));
#46345=CARTESIAN_POINT('Ctrl Pts',(-0.214228592898141,-0.855896236083242,
-0.995578837341434));
#46346=CARTESIAN_POINT('Ctrl Pts',(0.218231986874677,-0.854884235941514,
-0.975875564206509));
#46347=CARTESIAN_POINT('Ctrl Pts',(0.598262325502182,-0.648486273440926,
-0.956172291071585));
#46348=CARTESIAN_POINT('Ctrl Pts',(0.834560123160567,-0.286289465029356,
-0.936469017936662));
#46349=CARTESIAN_POINT('Ctrl Pts',(0.870354827142315,0.144688395618483,
-0.916765744801736));
#46350=CARTESIAN_POINT('Ctrl Pts',(0.697046758782688,0.540904865042945,
-0.897062471666814));
#46351=CARTESIAN_POINT('Ctrl Pts',(0.356273186507159,0.807168925029088,
-0.877359198531888));
#46352=CARTESIAN_POINT('Ctrl Pts',(-0.0700950291095755,0.879510627480251,
-0.857655925396965));
#46353=CARTESIAN_POINT('Ctrl Pts',(-0.479622911959631,0.740549876294596,
-0.83795265226204));
#46354=CARTESIAN_POINT('Ctrl Pts',(-0.77392137636837,0.423671995955202,
-0.818249379127117));
#46355=CARTESIAN_POINT('Ctrl Pts',(-0.88228520776747,0.00500690635942724,
-0.798546105992192));
#46356=CARTESIAN_POINT('Ctrl Pts',(-0.778679992535662,-0.41486109263371,
-0.778842832857268));
#46357=CARTESIAN_POINT('Ctrl Pts',(-0.487996886622684,-0.73505870214776,
-0.759139559722345));
#46358=CARTESIAN_POINT('Ctrl Pts',(-0.0800725146138843,-0.878658437255334,
-0.739436286587419));
#46359=CARTESIAN_POINT('Ctrl Pts',(0.347089281341945,-0.811160457452224,
-0.719733013452496));
#46360=CARTESIAN_POINT('Ctrl Pts',(0.690862867437646,-0.548781154334267,
-0.700029740317572));
#46361=CARTESIAN_POINT('Ctrl Pts',(0.868656629691441,-0.154557163048435,
-0.680326467182648));
#46362=CARTESIAN_POINT('Ctrl Pts',(0.837755611590708,0.276799191120675,
-0.660623194047723));
#46363=CARTESIAN_POINT('Ctrl Pts',(0.605583783625261,0.641654531633949,
-0.6409199209128));
#46364=CARTESIAN_POINT('Ctrl Pts',(0.227920434166312,0.852352352402625,
-0.621216647777875));
#46365=CARTESIAN_POINT('Ctrl Pts',(-0.204500806181377,0.858272495905586,
-0.601513374642951));
#46366=CARTESIAN_POINT('Ctrl Pts',(-0.587790721937716,0.657992647495812,
-0.581810101508027));
#46367=CARTESIAN_POINT('Ctrl Pts',(-0.829863899791275,0.299630046533427,
-0.562106828373103));
#46368=CARTESIAN_POINT('Ctrl Pts',(-0.872562251752902,-0.130718681755497,
-0.542403555238179));
#46369=CARTESIAN_POINT('Ctrl Pts',(-0.705627497577025,-0.529662242982048,
-0.522700282103254));
#46370=CARTESIAN_POINT('Ctrl Pts',(-0.369165716682379,-0.801354435040497,
-0.502997008968331));
#46371=CARTESIAN_POINT('Ctrl Pts',(0.0559881381817874,-0.88052120096025,
-0.483293735833406));
#46372=CARTESIAN_POINT('Ctrl Pts',(0.467690841465955,-0.748142722918232,
-0.463590462698483));
#46373=CARTESIAN_POINT('Ctrl Pts',(0.767030806126306,-0.436022934136046,
-0.443887189563558));
#46374=CARTESIAN_POINT('Ctrl Pts',(0.882091598392154,-0.0191486227757228,
-0.424183916428634));
#46375=CARTESIAN_POINT('Ctrl Pts',(0.785229856874429,0.402326145625984,
-0.40448064329371));
#46376=CARTESIAN_POINT('Ctrl Pts',(0.499716623159844,0.727142046192322,
-0.384777370158786));
#46377=CARTESIAN_POINT('Ctrl Pts',(0.0941464492269416,0.877262048653223,
-0.365074097023862));
#46378=CARTESIAN_POINT('Ctrl Pts',(-0.3340423978464,0.816619819635224,-0.345370823888938));
#46379=CARTESIAN_POINT('Ctrl Pts',(-0.681977576889138,0.559784653343796,
-0.325667550754014));
#46380=CARTESIAN_POINT('Ctrl Pts',(-0.866067568635368,0.168461211957287,
-0.30596427761909));
#46381=CARTESIAN_POINT('Ctrl Pts',(-0.842084910323148,-0.263335048428687,
-0.286261004484165));
#46382=CARTESIAN_POINT('Ctrl Pts',(-0.615791113824046,-0.631865040078709,
-0.266557731349242));
#46383=CARTESIAN_POINT('Ctrl Pts',(-0.241553908007489,-0.848589468760584,
-0.246854458214317));
#46384=CARTESIAN_POINT('Ctrl Pts',(0.190717468786097,-0.861440191483295,
-0.227151185079393));
#46385=CARTESIAN_POINT('Ctrl Pts',(0.577167311767125,-0.667330005151926,
-0.207447911944469));
#46386=CARTESIAN_POINT('Ctrl Pts',(0.824955967175025,-0.312893524930918,
-0.187744638809545));
#46387=CARTESIAN_POINT('Ctrl Pts',(0.874542449448201,0.116715157342132,
-0.168041365674621));
#46388=CARTESIAN_POINT('Ctrl Pts',(0.714032896413046,0.518283961256023,
-0.148338092539697));
#46389=CARTESIAN_POINT('Ctrl Pts',(0.381951553088681,0.795333171794517,
-0.128634819404772));
#46390=CARTESIAN_POINT('Ctrl Pts',(-0.0418431784879791,0.88130717347886,
-0.108931546269849));
#46391=CARTESIAN_POINT('Ctrl Pts',(-0.455688651728263,0.755540682228038,
-0.0892282731349243));
#46392=CARTESIAN_POINT('Ctrl Pts',(-0.658428920058076,0.550684467012711,
-0.0760927577116414));
#46393=CARTESIAN_POINT('Ctrl Pts',(-0.729452881030877,0.430276776454125,
-0.0695250000000001));
#46394=CARTESIAN_POINT('Ctrl Pts',(-0.390989273841475,0.804458378544447,
-1.81537138809545));
#46395=CARTESIAN_POINT('Ctrl Pts',(-0.523777803477758,0.739919438853238,
-1.80880363038381));
#46396=CARTESIAN_POINT('Ctrl Pts',(-0.756656134146546,0.543895053115038,
-1.79566811496052));
#46397=CARTESIAN_POINT('Ctrl Pts',(-0.924209591393358,0.118918397251283,
-1.7759648418256));
#46398=CARTESIAN_POINT('Ctrl Pts',(-0.869706111925403,-0.33451992640795,
-1.75626156869068));
#46399=CARTESIAN_POINT('Ctrl Pts',(-0.606263801520612,-0.70764266610669,
-1.73655829555575));
#46400=CARTESIAN_POINT('Ctrl Pts',(-0.19716248576299,-0.910727689108931,
-1.71685502242083));
#46401=CARTESIAN_POINT('Ctrl Pts',(0.259305043160306,-0.895023767386323,
-1.6971517492859));
#46402=CARTESIAN_POINT('Ctrl Pts',(0.653475579775621,-0.664283580481048,
-1.67744847615098));
#46403=CARTESIAN_POINT('Ctrl Pts',(0.890648057616496,-0.273952672142162,
-1.65774520301605));
#46404=CARTESIAN_POINT('Ctrl Pts',(0.913842582861546,0.18219710698654,-1.63804192988113));
#46405=CARTESIAN_POINT('Ctrl Pts',(0.717486265197291,0.594573149376045,
-1.61833865674621));
#46406=CARTESIAN_POINT('Ctrl Pts',(0.348753920382767,0.864103418700094,
-1.59863538361128));
#46407=CARTESIAN_POINT('Ctrl Pts',(-0.103766598645288,0.926032592612129,
-1.57893211047636));
#46408=CARTESIAN_POINT('Ctrl Pts',(-0.531357171768844,0.765482522757027,
-1.55922883734143));
#46409=CARTESIAN_POINT('Ctrl Pts',(-0.831289177930963,0.421025197405753,
-1.53952556420651));
#46410=CARTESIAN_POINT('Ctrl Pts',(-0.931503930605742,-0.0245834147939755,
-1.51982229107159));
#46411=CARTESIAN_POINT('Ctrl Pts',(-0.807924839340912,-0.464285875534232,
-1.50011901793666));
#46412=CARTESIAN_POINT('Ctrl Pts',(-0.490241780956103,-0.792443633866798,
-1.48041574480174));
#46413=CARTESIAN_POINT('Ctrl Pts',(-0.0547781211284922,-0.930216790038264,
-1.46071247166681));
#46414=CARTESIAN_POINT('Ctrl Pts',(0.393845984175257,-0.844505333660041,
-1.44100919853189));
#46415=CARTESIAN_POINT('Ctrl Pts',(0.747848580264941,-0.555901447453789,
-1.42130592539697));
#46416=CARTESIAN_POINT('Ctrl Pts',(0.922180533436526,-0.133742221967667,
-1.40160265226204));
#46417=CARTESIAN_POINT('Ctrl Pts',(0.874958586795736,0.32054857596129,-1.38189937912712));
#46418=CARTESIAN_POINT('Ctrl Pts',(0.617527814443183,0.697827569387674,
-1.36219610599219));
#46419=CARTESIAN_POINT('Ctrl Pts',(0.211735966837673,0.90745346906512,-1.34249283285727));
#46420=CARTESIAN_POINT('Ctrl Pts',(-0.244925452906858,0.89906364664017,
-1.32278955972234));
#46421=CARTESIAN_POINT('Ctrl Pts',(-0.642743525523892,0.674673757144865,
-1.30308628658742));
#46422=CARTESIAN_POINT('Ctrl Pts',(-0.886142447581508,0.288193478030981,
-1.28338301345249));
#46423=CARTESIAN_POINT('Ctrl Pts',(-0.916645621032203,-0.167525292501866,
-1.26367974031757));
#46424=CARTESIAN_POINT('Ctrl Pts',(-0.726924657573103,-0.582996106673904,
-1.24397646718265));
#46425=CARTESIAN_POINT('Ctrl Pts',(-0.362560024151519,-0.858402089391984,
-1.22427319404772));
#46426=CARTESIAN_POINT('Ctrl Pts',(0.0889096655368591,-0.927576945357665,
-1.2045699209128));
#46427=CARTESIAN_POINT('Ctrl Pts',(0.519018805513831,-0.773901413429442,
-1.18486664777787));
#46428=CARTESIAN_POINT('Ctrl Pts',(0.824433662486056,-0.434296044588096,
-1.16516337464295));
#46429=CARTESIAN_POINT('Ctrl Pts',(0.931778308250955,0.00964896150024885,
-1.14546010150803));
#46430=CARTESIAN_POINT('Ctrl Pts',(0.815263188565314,0.451275804309702,
-1.1257568283731));
#46431=CARTESIAN_POINT('Ctrl Pts',(0.502881064296495,0.78448362210888,-1.10605355523818));
#46432=CARTESIAN_POINT('Ctrl Pts',(0.0696817498161479,0.929219227054417,
-1.08635028210326));
#46433=CARTESIAN_POINT('Ctrl Pts',(-0.380258607068705,0.850709885880736,
-1.06664700896833));
#46434=CARTESIAN_POINT('Ctrl Pts',(-0.738841822630168,0.567817470070777,
-1.04694373583341));
#46435=CARTESIAN_POINT('Ctrl Pts',(-0.919918268980071,0.148506890687803,
-1.02724046269848));
#46436=CARTESIAN_POINT('Ctrl Pts',(-0.879984324656564,-0.306482473469165,
-1.00753718956356));
#46437=CARTESIAN_POINT('Ctrl Pts',(-0.62863412093596,-0.68783941452938,
-0.987833916428634));
#46438=CARTESIAN_POINT('Ctrl Pts',(-0.226254551516672,-0.903942916396294,
-0.96813064329371));
#46439=CARTESIAN_POINT('Ctrl Pts',(0.23048268043472,-0.902874106509137,
-0.948427370158786));
#46440=CARTESIAN_POINT('Ctrl Pts',(0.631846441759413,-0.684889766474151,
-0.928724097023861));
#46441=CARTESIAN_POINT('Ctrl Pts',(0.881409077214873,-0.302360640276263,
-0.909020823888938));
#46442=CARTESIAN_POINT('Ctrl Pts',(0.91921315642998,0.152810638474815,-0.889317550754013));
#46443=CARTESIAN_POINT('Ctrl Pts',(0.736176248282189,0.571269156921856,
-0.86961427761909));
#46444=CARTESIAN_POINT('Ctrl Pts',(0.376272975236873,0.852480243930285,
-0.849911004484164));
#46445=CARTESIAN_POINT('Ctrl Pts',(-0.0740298909692007,0.928882927729935,
-0.830207731349242));
#46446=CARTESIAN_POINT('Ctrl Pts',(-0.506547073733252,0.782121461332782,
-0.810504458214316));
#46447=CARTESIAN_POINT('Ctrl Pts',(-0.817366307412782,0.447455291276615,
-0.790801185079393));
#46448=CARTESIAN_POINT('Ctrl Pts',(-0.931813262145332,0.00528797457665684,
-0.771097911944469));
#46449=CARTESIAN_POINT('Ctrl Pts',(-0.822392053753201,-0.438149778167965,
-0.751394638809545));
#46450=CARTESIAN_POINT('Ctrl Pts',(-0.515391130710755,-0.776322034061729,
-0.731691365674621));
#46451=CARTESIAN_POINT('Ctrl Pts',(-0.0845674736396679,-0.927982898865733,
-0.711988092539696));
#46452=CARTESIAN_POINT('Ctrl Pts',(0.366573521414127,-0.856695845433538,
-0.692284819404772));
#46453=CARTESIAN_POINT('Ctrl Pts',(0.729645217368095,-0.579587590409729,
-0.672581546269848));
#46454=CARTESIAN_POINT('Ctrl Pts',(0.917419628790013,-0.163233400061772,
-0.652878273134924));
#46455=CARTESIAN_POINT('Ctrl Pts',(0.884783947916574,0.292337619362334,
-0.633175));
#46456=CARTESIAN_POINT('Ctrl Pts',(0.639578898018757,0.677674517297069,
-0.613471726865075));
#46457=CARTESIAN_POINT('Ctrl Pts',(0.240714999413281,0.900200092892027,
-0.593768453730152));
#46458=CARTESIAN_POINT('Ctrl Pts',(-0.215980684750912,0.906452570187688,
-0.574065180595228));
#46459=CARTESIAN_POINT('Ctrl Pts',(-0.620787003165868,0.694929791333767,
-0.554361907460304));
#46460=CARTESIAN_POINT('Ctrl Pts',(-0.876449226161066,0.316450110054044,
-0.53465863432538));
#46461=CARTESIAN_POINT('Ctrl Pts',(-0.921544497258574,-0.138056719298448,
-0.514955361190455));
#46462=CARTESIAN_POINT('Ctrl Pts',(-0.745238676323796,-0.559395417857205,
-0.495252088055532));
#46463=CARTESIAN_POINT('Ctrl Pts',(-0.389889241829712,-0.84633935112569,
-0.475548814920607));
#46464=CARTESIAN_POINT('Ctrl Pts',(0.0591310941420255,-0.929950230868132,
-0.455845541785683));
#46465=CARTESIAN_POINT('Ctrl Pts',(0.493945183286743,-0.790140540785833,
-0.436142268650758));
#46466=CARTESIAN_POINT('Ctrl Pts',(0.810088927401454,-0.460499563010433,
-0.416438995515835));
#46467=CARTESIAN_POINT('Ctrl Pts',(0.931608784293944,-0.0202235518595937,
-0.39673572238091));
#46468=CARTESIAN_POINT('Ctrl Pts',(0.829309601959138,0.42491116806858,-0.377032449245987));
#46469=CARTESIAN_POINT('Ctrl Pts',(0.527768767599633,0.767960967882476,
-0.357329176111062));
#46470=CARTESIAN_POINT('Ctrl Pts',(0.0994314641129952,0.926508122447519,
-0.337625902976139));
#46471=CARTESIAN_POINT('Ctrl Pts',(-0.352794236706888,0.862461674941034,
-0.317922629841215));
#46472=CARTESIAN_POINT('Ctrl Pts',(-0.720261141223303,0.591208782986478,
-0.29821935670629));
#46473=CARTESIAN_POINT('Ctrl Pts',(-0.914685227932655,0.177917968109297,
-0.278516083571366));
#46474=CARTESIAN_POINT('Ctrl Pts',(-0.889356276613872,-0.278117652152912,
-0.258812810436442));
#46475=CARTESIAN_POINT('Ctrl Pts',(-0.650359227969422,-0.667335481823592,
-0.239109537301518));
#46476=CARTESIAN_POINT('Ctrl Pts',(-0.255113803362931,-0.896225975621676,
-0.219406264166594));
#46477=CARTESIAN_POINT('Ctrl Pts',(0.201423604491066,-0.909798087854495,
-0.19970299103167));
#46478=CARTESIAN_POINT('Ctrl Pts',(0.609567236134733,-0.704791311872434,
-0.179999717896745));
#46479=CARTESIAN_POINT('Ctrl Pts',(0.87126578132795,-0.33045814845722,-0.160296444761821));
#46480=CARTESIAN_POINT('Ctrl Pts',(0.923635855538078,0.123267091579122,
-0.140593171626897));
#46481=CARTESIAN_POINT('Ctrl Pts',(0.754115921504916,0.547378403722327,
-0.120889898491973));
#46482=CARTESIAN_POINT('Ctrl Pts',(0.403392825281099,0.839980077618579,
-0.101186625357049));
#46483=CARTESIAN_POINT('Ctrl Pts',(-0.0441920915166111,0.930780324821963,
-0.0814833522221251));
#46484=CARTESIAN_POINT('Ctrl Pts',(-0.48126923737503,0.797953792710495,
-0.0617800790872008));
#46485=CARTESIAN_POINT('Ctrl Pts',(-0.695390554538055,0.58159774764706,
-0.0486445636639179));
#46486=CARTESIAN_POINT('Ctrl Pts',(-0.770401523986372,0.454430838421997,
-0.0420768059522765));
#46487=CARTESIAN_POINT('Ctrl Pts',(-0.411771268263186,0.847217222978089,
-1.78792319404772));
#46488=CARTESIAN_POINT('Ctrl Pts',(-0.551617818839675,0.779247887686847,
-1.78135543633608));
#46489=CARTESIAN_POINT('Ctrl Pts',(-0.796874177481831,0.57280434734907,
-1.7682199209128));
#46490=CARTESIAN_POINT('Ctrl Pts',(-0.973333492885899,0.12523918821323,
-1.74851664777788));
#46491=CARTESIAN_POINT('Ctrl Pts',(-0.915933026001545,-0.352300442932758,
-1.72881337464295));
#46492=CARTESIAN_POINT('Ctrl Pts',(-0.638488140611806,-0.745255528974016,
-1.70911010150803));
#46493=CARTESIAN_POINT('Ctrl Pts',(-0.207642133040882,-0.959134995961123,
-1.6894068283731));
#46494=CARTESIAN_POINT('Ctrl Pts',(0.273087712714213,-0.942596374067765,
-1.66970355523818));
#46495=CARTESIAN_POINT('Ctrl Pts',(0.688209335308588,-0.699591806531232,
-1.65000028210326));
#46496=CARTESIAN_POINT('Ctrl Pts',(0.93798808508896,-0.288513897437003,
-1.63029700896833));
#46497=CARTESIAN_POINT('Ctrl Pts',(0.962415453602374,0.191881309378704,
-1.61059373583341));
#46498=CARTESIAN_POINT('Ctrl Pts',(0.755622338380288,0.626176102961525,
-1.59089046269848));
#46499=CARTESIAN_POINT('Ctrl Pts',(0.3672910069804,0.910032536526708,-1.57118718956356));
#46500=CARTESIAN_POINT('Ctrl Pts',(-0.109282036071534,0.975253390883418,
-1.55148391642864));
#46501=CARTESIAN_POINT('Ctrl Pts',(-0.55960004828344,0.806169709291727,
-1.53178064329371));
#46502=CARTESIAN_POINT('Ctrl Pts',(-0.875474142108766,0.443403671418404,
-1.51207737015879));
#46503=CARTESIAN_POINT('Ctrl Pts',(-0.981015543288755,-0.0258900807904488,
-1.49237409702386));
#46504=CARTESIAN_POINT('Ctrl Pts',(-0.850867934273877,-0.488963755775376,
-1.47267082388894));
#46505=CARTESIAN_POINT('Ctrl Pts',(-0.516299278280827,-0.834563866518545,
-1.45296755075401));
#46506=CARTESIAN_POINT('Ctrl Pts',(-0.057689706391535,-0.979659988189516,
-1.43326427761909));
#46507=CARTESIAN_POINT('Ctrl Pts',(0.414779819433004,-0.889392767427202,
-1.41356100448416));
#46508=CARTESIAN_POINT('Ctrl Pts',(0.787598481510704,-0.585448909629671,
-1.39385773134924));
#46509=CARTESIAN_POINT('Ctrl Pts',(0.971196585752732,-0.140850933885956,
-1.37415445821432));
#46510=CARTESIAN_POINT('Ctrl Pts',(0.921464682196681,0.337586482531115,
-1.35445118507939));
#46511=CARTESIAN_POINT('Ctrl Pts',(0.650350862167541,0.734918736907045,
-1.33474791194447));
#46512=CARTESIAN_POINT('Ctrl Pts',(0.2229902287218,0.955686743463641,-1.31504463880954));
#46513=CARTESIAN_POINT('Ctrl Pts',(-0.257943813605184,0.946850982353159,
-1.29534136567462));
#46514=CARTESIAN_POINT('Ctrl Pts',(-0.676906847271293,0.710534245387173,
-1.2756380925397));
#46515=CARTESIAN_POINT('Ctrl Pts',(-0.93324299134207,0.303511635467807,
-1.25593481940477));
#46516=CARTESIAN_POINT('Ctrl Pts',(-0.965367479808057,-0.176429653637053,
-1.23623154626985));
#46517=CARTESIAN_POINT('Ctrl Pts',(-0.765562403387109,-0.613983713361266,
-1.21652827313492));
#46518=CARTESIAN_POINT('Ctrl Pts',(-0.381830937456696,-0.904028168230564,
-1.196825));
#46519=CARTESIAN_POINT('Ctrl Pts',(0.0936354222182865,-0.976879829589592,
-1.17712172686507));
#46520=CARTESIAN_POINT('Ctrl Pts',(0.546605869002752,-0.815036083695018,
-1.15741845373015));
#46521=CARTESIAN_POINT('Ctrl Pts',(0.868254239983032,-0.457379895168767,
-1.13771518059523));
#46522=CARTESIAN_POINT('Ctrl Pts',(0.981304504747574,0.0101618263727374,
-1.1180119074603));
#46523=CARTESIAN_POINT('Ctrl Pts',(0.858596333923827,0.475262168834934,
-1.09830863432538));
#46524=CARTESIAN_POINT('Ctrl Pts',(0.529610369093823,0.826180761517367,
-1.07860536119046));
#46525=CARTESIAN_POINT('Ctrl Pts',(0.073385497803265,0.978609402399795,
-1.05890208805553));
#46526=CARTESIAN_POINT('Ctrl Pts',(-0.400470241452602,0.895927106110765,
-1.03919881492061));
#46527=CARTESIAN_POINT('Ctrl Pts',(-0.778112993640995,0.59799829672012,
-1.01949554178568));
#46528=CARTESIAN_POINT('Ctrl Pts',(-0.968814076649019,0.156400379282867,
-0.999792268650758));
#46529=CARTESIAN_POINT('Ctrl Pts',(-0.926757549779925,-0.322772733791168,
-0.980088995515835));
#46530=CARTESIAN_POINT('Ctrl Pts',(-0.662047494827864,-0.724399688255913,
-0.960385722380911));
#46531=CARTESIAN_POINT('Ctrl Pts',(-0.238280510135202,-0.951989596709347,
-0.940682449245987));
#46532=CARTESIAN_POINT('Ctrl Pts',(0.242733373994761,-0.95086397707676,
-0.920979176111061));
#46533=CARTESIAN_POINT('Ctrl Pts',(0.665430558016644,-0.721293259507376,
-0.901275902976139));
#46534=CARTESIAN_POINT('Ctrl Pts',(0.928258031269179,-0.318431815523169,
-0.881572629841214));
#46535=CARTESIAN_POINT('Ctrl Pts',(0.968071485717646,0.160932881331148,
-0.86186935670629));
#46536=CARTESIAN_POINT('Ctrl Pts',(0.775305737781691,0.601633448800766,
-0.842166083571366));
#46537=CARTESIAN_POINT('Ctrl Pts',(0.396272763966587,0.897791562831483,
-0.822462810436441));
#46538=CARTESIAN_POINT('Ctrl Pts',(-0.0779647528288262,0.978255227979619,
-0.802759537301518));
#46539=CARTESIAN_POINT('Ctrl Pts',(-0.533471235506874,0.823693046370968,
-0.783056264166593));
#46540=CARTESIAN_POINT('Ctrl Pts',(-0.860811238457195,0.471238586598027,
-0.76335299103167));
#46541=CARTESIAN_POINT('Ctrl Pts',(-0.981341316523194,0.0055690427938866,
-0.743649717896745));
#46542=CARTESIAN_POINT('Ctrl Pts',(-0.866104114970739,-0.461438463702219,
-0.723946444761821));
#46543=CARTESIAN_POINT('Ctrl Pts',(-0.542785374798827,-0.8175853659757,
-0.704243171626897));
#46544=CARTESIAN_POINT('Ctrl Pts',(-0.089062432665451,-0.977307360476132,
-0.684539898491973));
#46545=CARTESIAN_POINT('Ctrl Pts',(0.386057761486308,-0.902231233414852,
-0.664836625357049));
#46546=CARTESIAN_POINT('Ctrl Pts',(0.768427567298545,-0.610394026485191,
-0.645133352222124));
#46547=CARTESIAN_POINT('Ctrl Pts',(0.966182627888584,-0.171909637075109,
-0.625430079087201));
#46548=CARTESIAN_POINT('Ctrl Pts',(0.931812284242439,0.307876047603994,
-0.605726805952276));
#46549=CARTESIAN_POINT('Ctrl Pts',(0.673574012412253,0.71369450296019,-0.586023532817353));
#46550=CARTESIAN_POINT('Ctrl Pts',(0.253509564660249,0.948047833381428,
-0.566320259682428));
#46551=CARTESIAN_POINT('Ctrl Pts',(-0.227460563320446,0.95463264446979,
-0.546616986547504));
#46552=CARTESIAN_POINT('Ctrl Pts',(-0.65378328439402,0.731866935171721,
-0.526913713412581));
#46553=CARTESIAN_POINT('Ctrl Pts',(-0.923034552530858,0.333270173574662,
-0.507210440277655));
#46554=CARTESIAN_POINT('Ctrl Pts',(-0.970526742764244,-0.145394756841399,
-0.487507167142732));
#46555=CARTESIAN_POINT('Ctrl Pts',(-0.78484985507057,-0.589128592732363,
-0.467803894007808));
#46556=CARTESIAN_POINT('Ctrl Pts',(-0.410612766977043,-0.891324267210884,
-0.448100620872884));
#46557=CARTESIAN_POINT('Ctrl Pts',(0.0622740501022626,-0.979379260776014,
-0.428397347737959));
#46558=CARTESIAN_POINT('Ctrl Pts',(0.520199525107533,-0.832138358653435,
-0.408694074603035));
#46559=CARTESIAN_POINT('Ctrl Pts',(0.8531470486766,-0.48497619188482,-0.388990801468111));
#46560=CARTESIAN_POINT('Ctrl Pts',(0.981125970195735,-0.0212984809434644,
-0.369287528333187));
#46561=CARTESIAN_POINT('Ctrl Pts',(0.873389347043846,0.447496190511176,
-0.349584255198263));
#46562=CARTESIAN_POINT('Ctrl Pts',(0.555820912039423,0.808779889572632,
-0.329880982063339));
#46563=CARTESIAN_POINT('Ctrl Pts',(0.104716478999048,0.975754196241814,
-0.310177708928415));
#46564=CARTESIAN_POINT('Ctrl Pts',(-0.371546075567376,0.908303530246846,
-0.290474435793491));
#46565=CARTESIAN_POINT('Ctrl Pts',(-0.758544705557467,0.62263291262916,
-0.270771162658567));
#46566=CARTESIAN_POINT('Ctrl Pts',(-0.963302887229944,0.187374724261306,
-0.251067889523643));
#46567=CARTESIAN_POINT('Ctrl Pts',(-0.936627642904595,-0.292900255877137,
-0.231364616388719));
#46568=CARTESIAN_POINT('Ctrl Pts',(-0.684927342114798,-0.702805923568475,
-0.211661343253794));
#46569=CARTESIAN_POINT('Ctrl Pts',(-0.268673698718373,-0.943862482482769,
-0.19195807011887));
#46570=CARTESIAN_POINT('Ctrl Pts',(0.212129740196035,-0.958155984225694,
-0.172254796983946));
#46571=CARTESIAN_POINT('Ctrl Pts',(0.641967160502342,-0.742252618592942,
-0.152551523849022));
#46572=CARTESIAN_POINT('Ctrl Pts',(0.917575595480876,-0.348022771983522,
-0.132848250714098));
#46573=CARTESIAN_POINT('Ctrl Pts',(0.972729261627955,0.129819025816112,
-0.113144977579174));
#46574=CARTESIAN_POINT('Ctrl Pts',(0.794198946596785,0.57647284618863,-0.0934417044442497));
#46575=CARTESIAN_POINT('Ctrl Pts',(0.424834097473517,0.884626983442641,
-0.0737384313093252));
#46576=CARTESIAN_POINT('Ctrl Pts',(-0.046541004545243,0.980253476165065,
-0.0540351581744016));
#46577=CARTESIAN_POINT('Ctrl Pts',(-0.506849823021797,0.840366903192951,
-0.0343318850394773));
#46578=CARTESIAN_POINT('Ctrl Pts',(-0.732352189018033,0.612511028281409,
-0.0211963696161944));
#46579=CARTESIAN_POINT('Ctrl Pts',(-0.811350166941868,0.478584900389869,
-0.014628611904553));
#46580=CARTESIAN_POINT('Ctrl Pts',(-0.432553262684897,0.889976067411731,
-1.760475));
#46581=CARTESIAN_POINT('Ctrl Pts',(-0.579457834201591,0.818576336520457,
-1.75390724228836));
#46582=CARTESIAN_POINT('Ctrl Pts',(-0.837092220817113,0.601713641583103,
-1.74077172686507));
#46583=CARTESIAN_POINT('Ctrl Pts',(-1.02245739437844,0.131559979175176,
-1.72106845373015));
#46584=CARTESIAN_POINT('Ctrl Pts',(-0.962159940077686,-0.370080959457566,
-1.70136518059523));
#46585=CARTESIAN_POINT('Ctrl Pts',(-0.670712479703,-0.782868391841341,-1.6816619074603));
#46586=CARTESIAN_POINT('Ctrl Pts',(-0.218121780318774,-1.00754230281332,
-1.66195863432538));
#46587=CARTESIAN_POINT('Ctrl Pts',(0.28687038226812,-0.990168980749204,
-1.64225536119046));
#46588=CARTESIAN_POINT('Ctrl Pts',(0.722943090841553,-0.734900032581417,
-1.62255208805553));
#46589=CARTESIAN_POINT('Ctrl Pts',(0.985328112561426,-0.303075122731843,
-1.60284881492061));
#46590=CARTESIAN_POINT('Ctrl Pts',(1.0109883243432,0.201565511770867,-1.58314554178568));
#46591=CARTESIAN_POINT('Ctrl Pts',(0.793758411563286,0.657779056547004,
-1.56344226865076));
#46592=CARTESIAN_POINT('Ctrl Pts',(0.385828093578033,0.955961654353322,
-1.54373899551583));
#46593=CARTESIAN_POINT('Ctrl Pts',(-0.11479747349778,1.02447418915471,-1.52403572238091));
#46594=CARTESIAN_POINT('Ctrl Pts',(-0.587842924798037,0.846856895826426,
-1.50433244924599));
#46595=CARTESIAN_POINT('Ctrl Pts',(-0.919659106286569,0.465782145431056,
-1.48462917611106));
#46596=CARTESIAN_POINT('Ctrl Pts',(-1.03052715597177,-0.0271967467869228,
-1.46492590297614));
#46597=CARTESIAN_POINT('Ctrl Pts',(-0.893811029206843,-0.51364163601652,
-1.44522262984121));
#46598=CARTESIAN_POINT('Ctrl Pts',(-0.542356775605552,-0.876684099170293,
-1.42551935670629));
#46599=CARTESIAN_POINT('Ctrl Pts',(-0.0606012916545775,-1.02910318634077,
-1.40581608357137));
#46600=CARTESIAN_POINT('Ctrl Pts',(0.435713654690751,-0.934280201194361,
-1.38611281043644));
#46601=CARTESIAN_POINT('Ctrl Pts',(0.827348382756466,-0.614996371805552,
-1.36640953730152));
#46602=CARTESIAN_POINT('Ctrl Pts',(1.02021263806894,-0.147959645804244,
-1.34670626416659));
#46603=CARTESIAN_POINT('Ctrl Pts',(0.967970777597627,0.354624389100941,
-1.32700299103167));
#46604=CARTESIAN_POINT('Ctrl Pts',(0.683173909891899,0.772009904426415,
-1.30729971789675));
#46605=CARTESIAN_POINT('Ctrl Pts',(0.234244490605928,1.00392001786216,-1.28759644476182));
#46606=CARTESIAN_POINT('Ctrl Pts',(-0.270962174303511,0.994638318066147,
-1.2678931716269));
#46607=CARTESIAN_POINT('Ctrl Pts',(-0.711070169018694,0.746394733629479,
-1.24818989849197));
#46608=CARTESIAN_POINT('Ctrl Pts',(-0.980343535102633,0.318829792904634,
-1.22848662535705));
#46609=CARTESIAN_POINT('Ctrl Pts',(-1.01408933858391,-0.185334014772241,
-1.20878335222212));
#46610=CARTESIAN_POINT('Ctrl Pts',(-0.804200149201113,-0.644971320048627,
-1.1890800790872));
#46611=CARTESIAN_POINT('Ctrl Pts',(-0.401101850761873,-0.949654247069143,
-1.16937680595228));
#46612=CARTESIAN_POINT('Ctrl Pts',(0.0983611788997142,-1.02618271382152,
-1.14967353281735));
#46613=CARTESIAN_POINT('Ctrl Pts',(0.574192932491672,-0.856170753960593,
-1.12997025968243));
#46614=CARTESIAN_POINT('Ctrl Pts',(0.912074817480007,-0.480463745749438,
-1.1102669865475));
#46615=CARTESIAN_POINT('Ctrl Pts',(1.03083070124419,0.0106746912452258,
-1.09056371341258));
#46616=CARTESIAN_POINT('Ctrl Pts',(0.901929479282339,0.499248533360167,
-1.07086044027766));
#46617=CARTESIAN_POINT('Ctrl Pts',(0.55633967389115,0.867877900925852,-1.05115716714273));
#46618=CARTESIAN_POINT('Ctrl Pts',(0.0770892457903824,1.02799957774517,
-1.03145389400781));
#46619=CARTESIAN_POINT('Ctrl Pts',(-0.4206818758365,0.941144326340793,-1.01175062087288));
#46620=CARTESIAN_POINT('Ctrl Pts',(-0.817384164651821,0.628179123369462,
-0.992047347737959));
#46621=CARTESIAN_POINT('Ctrl Pts',(-1.01770988431797,0.164293867877931,
-0.972344074603035));
#46622=CARTESIAN_POINT('Ctrl Pts',(-0.973530774903286,-0.339062994113169,
-0.952640801468111));
#46623=CARTESIAN_POINT('Ctrl Pts',(-0.695460868719769,-0.760959961982448,
-0.932937528333187));
#46624=CARTESIAN_POINT('Ctrl Pts',(-0.250306468753732,-1.0000362770224,
-0.913234255198262));
#46625=CARTESIAN_POINT('Ctrl Pts',(0.254984067554803,-0.998853847644383,
-0.89353098206334));
#46626=CARTESIAN_POINT('Ctrl Pts',(0.699014674273875,-0.7576967525406,-0.873827708928414));
#46627=CARTESIAN_POINT('Ctrl Pts',(0.975106985323486,-0.334502990770076,
-0.854124435793491));
#46628=CARTESIAN_POINT('Ctrl Pts',(1.01692981500531,0.16905512418748,-0.834421162658567));
#46629=CARTESIAN_POINT('Ctrl Pts',(0.814435227281192,0.631997740679676,
-0.814717889523642));
#46630=CARTESIAN_POINT('Ctrl Pts',(0.416272552696301,0.94310288173268,-0.795014616388719));
#46631=CARTESIAN_POINT('Ctrl Pts',(-0.0818996146884514,1.0276275282293,
-0.775311343253793));
#46632=CARTESIAN_POINT('Ctrl Pts',(-0.560395397280496,0.865264631409154,
-0.755608070118871));
#46633=CARTESIAN_POINT('Ctrl Pts',(-0.904256169501606,0.495021881919439,
-0.735904796983944));
#46634=CARTESIAN_POINT('Ctrl Pts',(-1.03086937090106,0.00585011101111694,
-0.716201523849023));
#46635=CARTESIAN_POINT('Ctrl Pts',(-0.909816176188277,-0.484727149236474,
-0.696498250714097));
#46636=CARTESIAN_POINT('Ctrl Pts',(-0.570179618886898,-0.858848697889669,
-0.676794977579175));
#46637=CARTESIAN_POINT('Ctrl Pts',(-0.0935573916912343,-1.02663182208653,
-0.657091704444248));
#46638=CARTESIAN_POINT('Ctrl Pts',(0.40554200155849,-0.947766621396166,
-0.637388431309326));
#46639=CARTESIAN_POINT('Ctrl Pts',(0.807209917228995,-0.641200462560654,
-0.617685158174401));
#46640=CARTESIAN_POINT('Ctrl Pts',(1.01494562698716,-0.180585874088446,
-0.597981885039478));
#46641=CARTESIAN_POINT('Ctrl Pts',(0.978840620568303,0.323414475845652,
-0.578278611904553));
#46642=CARTESIAN_POINT('Ctrl Pts',(0.707569126805749,0.749714488623311,
-0.55857533876963));
#46643=CARTESIAN_POINT('Ctrl Pts',(0.266304129907217,0.99589557387083,-0.538872065634705));
#46644=CARTESIAN_POINT('Ctrl Pts',(-0.238940441889981,1.00281271875189,
-0.519168792499781));
#46645=CARTESIAN_POINT('Ctrl Pts',(-0.686779565622172,0.768804079009677,
-0.499465519364857));
#46646=CARTESIAN_POINT('Ctrl Pts',(-0.969619878900649,0.350090237095279,
-0.479762246229933));
#46647=CARTESIAN_POINT('Ctrl Pts',(-1.01950898826992,-0.152732794384349,
-0.460058973095008));
#46648=CARTESIAN_POINT('Ctrl Pts',(-0.824461033817341,-0.618861767607521,
-0.440355699960084));
#46649=CARTESIAN_POINT('Ctrl Pts',(-0.431336292124375,-0.936309183296075,
-0.42065242682516));
#46650=CARTESIAN_POINT('Ctrl Pts',(0.0654170060624995,-1.0288082906839,
-0.400949153690236));
#46651=CARTESIAN_POINT('Ctrl Pts',(0.546453866928323,-0.874136176521035,
-0.381245880555312));
#46652=CARTESIAN_POINT('Ctrl Pts',(0.896205169951745,-0.509452820759208,
-0.361542607420388));
#46653=CARTESIAN_POINT('Ctrl Pts',(1.03064315609753,-0.0223734100273349,
-0.341839334285463));
#46654=CARTESIAN_POINT('Ctrl Pts',(0.917469092128553,0.470081212953772,
-0.32213606115054));
#46655=CARTESIAN_POINT('Ctrl Pts',(0.583873056479214,0.849598811262788,
-0.302432788015615));
#46656=CARTESIAN_POINT('Ctrl Pts',(0.110001493885101,1.02500027003611,-0.282729514880691));
#46657=CARTESIAN_POINT('Ctrl Pts',(-0.390297914427862,0.954145385552656,
-0.263026241745767));
#46658=CARTESIAN_POINT('Ctrl Pts',(-0.796828269891632,0.654057042271841,
-0.243322968610843));
#46659=CARTESIAN_POINT('Ctrl Pts',(-1.01192054652723,0.196831480413315,
-0.223619695475919));
#46660=CARTESIAN_POINT('Ctrl Pts',(-0.983899009195318,-0.307682859601362,
-0.203916422340995));
#46661=CARTESIAN_POINT('Ctrl Pts',(-0.719495456260174,-0.738276365313358,
-0.184213149206071));
#46662=CARTESIAN_POINT('Ctrl Pts',(-0.282233594073814,-0.991498989343861,
-0.164509876071147));
#46663=CARTESIAN_POINT('Ctrl Pts',(0.222835875901004,-1.00651388059689,
-0.144806602936223));
#46664=CARTESIAN_POINT('Ctrl Pts',(0.674367084869952,-0.779713925313451,
-0.125103329801299));
#46665=CARTESIAN_POINT('Ctrl Pts',(0.963885409633801,-0.365587395509823,
-0.105400056666374));
#46666=CARTESIAN_POINT('Ctrl Pts',(1.02182266771783,0.136370960053101,-0.0856967835314503));
#46667=CARTESIAN_POINT('Ctrl Pts',(0.834281971688654,0.605567288654934,
-0.0659935103965262));
#46668=CARTESIAN_POINT('Ctrl Pts',(0.446275369665935,0.929273889266702,
-0.0462902372616017));
#46669=CARTESIAN_POINT('Ctrl Pts',(-0.0488899175738751,1.02972662750817,
-0.0265869641266781));
#46670=CARTESIAN_POINT('Ctrl Pts',(-0.532430408668564,0.882780013675407,
-0.00688369099175381));
#46671=CARTESIAN_POINT('Ctrl Pts',(-0.769313823498012,0.643424308915757,
0.0062518244315291));
#46672=CARTESIAN_POINT('Ctrl Pts',(-0.852298809897364,0.502738962357741,
0.0128195821431705));
#46673=CARTESIAN_POINT('Ctrl Pts',(-0.989459186063674,1.54013734824731E-5,
-0.215975728002209));
#46674=CARTESIAN_POINT('Ctrl Pts',(-0.98940307000832,-0.0999713176614304,
-0.211955959448471));
#46675=CARTESIAN_POINT('Ctrl Pts',(-0.974331598209586,-0.199974581563408,
-0.207936190894733));
#46676=CARTESIAN_POINT('Ctrl Pts',(-0.94450200659478,-0.295362720550915,
-0.203916422340995));
#46677=CARTESIAN_POINT('Ctrl Pts',(-0.89576449155027,-0.451214028172027,
-0.197348664629354));
#46678=CARTESIAN_POINT('Ctrl Pts',(-0.807629973905222,-0.594745196742693,
-0.190780906917712));
#46679=CARTESIAN_POINT('Ctrl Pts',(-0.690685738051638,-0.708714551699776,
-0.184213149206071));
#46680=CARTESIAN_POINT('Ctrl Pts',(-0.573741502198054,-0.822683906656859,
-0.177645391494429));
#46681=CARTESIAN_POINT('Ctrl Pts',(-0.427987548135934,-0.90709144800036,
-0.171077633782788));
#46682=CARTESIAN_POINT('Ctrl Pts',(-0.270932326109071,-0.951797700547616,
-0.164509876071147));
#46683=CARTESIAN_POINT('Ctrl Pts',(-0.113877104082208,-0.996503953094872,
-0.157942118359506));
#46684=CARTESIAN_POINT('Ctrl Pts',(0.0544793859093978,-1.00150891684588,
-0.151374360647864));
#46685=CARTESIAN_POINT('Ctrl Pts',(0.213912832400026,-0.966211406174147,
-0.144806602936223));
#46686=CARTESIAN_POINT('Ctrl Pts',(0.373346278890653,-0.930913895502412,
-0.138238845224581));
#46687=CARTESIAN_POINT('Ctrl Pts',(0.523856681880303,-0.855313910407931,
-0.13167108751294));
#46688=CARTESIAN_POINT('Ctrl Pts',(0.647364937502435,-0.748492829560086,
-0.125103329801298));
#46689=CARTESIAN_POINT('Ctrl Pts',(0.770873193124568,-0.641671748712241,
-0.118535572089657));
#46690=CARTESIAN_POINT('Ctrl Pts',(0.867379301379184,-0.503629572111032,
-0.111967814378016));
#46691=CARTESIAN_POINT('Ctrl Pts',(0.925288565187164,-0.350948757883274,
-0.105400056666374));
#46692=CARTESIAN_POINT('Ctrl Pts',(0.983197828995144,-0.198267943655515,
-0.0988322989547328));
#46693=CARTESIAN_POINT('Ctrl Pts',(1.00251024835649,-0.0309484918012002,
-0.0922645412430913));
#46694=CARTESIAN_POINT('Ctrl Pts',(0.980909675365629,0.13091062222626,-0.08569678353145));
#46695=CARTESIAN_POINT('Ctrl Pts',(0.963180651960666,0.263759136111232,
-0.0803061890209666));
#46696=CARTESIAN_POINT('Ctrl Pts',(0.917890288593679,0.392929253024943,
-0.0749155945104836));
#46697=CARTESIAN_POINT('Ctrl Pts',(0.849186560444991,0.508032827447782,
-0.0695250000000002));
#46698=CARTESIAN_POINT('',(-0.491859688152273,-0.689459403554686,-1.760475));
#46699=CARTESIAN_POINT('Ctrl Pts',(-0.491859688152275,-0.689459403554684,
-1.760475));
#46700=CARTESIAN_POINT('Ctrl Pts',(-0.513554842694071,-0.676529705956258,
-1.760475));
#46701=CARTESIAN_POINT('Ctrl Pts',(-0.534635231361505,-0.662644680299156,
-1.760475));
#46702=CARTESIAN_POINT('Ctrl Pts',(-0.555033286604471,-0.647841975554216,
-1.760475));
#46703=CARTESIAN_POINT('Ctrl Pts',(-0.58415798250627,-0.626706417821615,
-1.760475));
#46704=CARTESIAN_POINT('Ctrl Pts',(-0.611892735613209,-0.603701443225965,
-1.760475));
#46705=CARTESIAN_POINT('Ctrl Pts',(-0.638121657096046,-0.579014067915186,
-1.760475));
#46706=CARTESIAN_POINT('Ctrl Pts',(-0.646098901072591,-0.571505668604011,
-1.760475));
#46707=CARTESIAN_POINT('Ctrl Pts',(-0.65393672584828,-0.563841411402002,
-1.760475));
#46708=CARTESIAN_POINT('Ctrl Pts',(-0.661631495607065,-0.556025978619957,
-1.760475));
#46709=CARTESIAN_POINT('Ctrl Pts',(-0.668300148268516,-0.549252753655965,
-1.760475));
#46710=CARTESIAN_POINT('Ctrl Pts',(-0.674859642024538,-0.54236754289441,
-1.760475));
#46711=CARTESIAN_POINT('Ctrl Pts',(-0.681300291911483,-0.535381927138061,
-1.760475));
#46712=CARTESIAN_POINT('Ctrl Pts',(-0.708273869420477,-0.506126021078973,
-1.760475));
#46713=CARTESIAN_POINT('Ctrl Pts',(-0.733203917913654,-0.475073691031234,
-1.760475));
#46714=CARTESIAN_POINT('Ctrl Pts',(-0.755936918937743,-0.442469540470751,
-1.760475));
#46715=CARTESIAN_POINT('Ctrl Pts',(-0.77218026589336,-0.419172988942604,
-1.760475));
#46716=CARTESIAN_POINT('Ctrl Pts',(-0.78730146906442,-0.395083087809655,
-1.760475));
#46717=CARTESIAN_POINT('Ctrl Pts',(-0.801233694577352,-0.370277201526068,
-1.760475));
#46718=CARTESIAN_POINT('Ctrl Pts',(-0.805786257659718,-0.362171507140401,
-1.760475));
#46719=CARTESIAN_POINT('Ctrl Pts',(-0.810207227008384,-0.353997321790457,
-1.760475));
#46720=CARTESIAN_POINT('Ctrl Pts',(-0.814493086153977,-0.345761134855412,
-1.760475));
#46721=CARTESIAN_POINT('Ctrl Pts',(-0.819180750550855,-0.336752793948747,
-1.760475));
#46722=CARTESIAN_POINT('Ctrl Pts',(-0.823707501249501,-0.327669012074212,
-1.760475));
#46723=CARTESIAN_POINT('Ctrl Pts',(-0.828071044204866,-0.318513817684205,
-1.760475));
#46724=CARTESIAN_POINT('Ctrl Pts',(-0.845392775283347,-0.282170915410279,
-1.760475));
#46725=CARTESIAN_POINT('Ctrl Pts',(-0.860145988846534,-0.244705464421566,
-1.760475));
#46726=CARTESIAN_POINT('Ctrl Pts',(-0.872333447502791,-0.206410510016498,
-1.760475));
#46727=CARTESIAN_POINT('Ctrl Pts',(-0.881034937585783,-0.179069029287595,
-1.760475));
#46728=CARTESIAN_POINT('Ctrl Pts',(-0.888427703296585,-0.151303781793152,
-1.760475));
#46729=CARTESIAN_POINT('Ctrl Pts',(-0.894498914094688,-0.12321284647818,
-1.760475));
#46730=CARTESIAN_POINT('Ctrl Pts',(-0.89903476223958,-0.102225893286487,
-1.760475));
#46731=CARTESIAN_POINT('Ctrl Pts',(-0.902832725396058,-0.0810569930890353,
-1.760475));
#46732=CARTESIAN_POINT('Ctrl Pts',(-0.905882898683675,-0.0597456113193039,
-1.760475));
#46733=CARTESIAN_POINT('Ctrl Pts',(-0.907009065019949,-0.0518771532136601,
-1.760475));
#46734=CARTESIAN_POINT('Ctrl Pts',(-0.9080335392552,-0.0439867555116406,
-1.760475));
#46735=CARTESIAN_POINT('Ctrl Pts',(-0.908954731322743,-0.0360847177437703,
-1.760475));
#46736=CARTESIAN_POINT('Ctrl Pts',(-0.913760013494143,0.00513526508232103,
-1.760475));
#46737=CARTESIAN_POINT('Ctrl Pts',(-0.915746617672292,0.0465497049188463,
-1.760475));
#46738=CARTESIAN_POINT('Ctrl Pts',(-0.914906895042617,0.0878627812257661,
-1.760475));
#46739=CARTESIAN_POINT('Ctrl Pts',(-0.914705277088933,0.0977820779209303,
-1.760475));
#46740=CARTESIAN_POINT('Ctrl Pts',(-0.914340512210413,0.107695632494892,
-1.760475));
#46741=CARTESIAN_POINT('Ctrl Pts',(-0.913812080888137,0.117599511663197,
-1.760475));
#46742=CARTESIAN_POINT('Ctrl Pts',(-0.911747207846467,0.156299437728377,
-1.760475));
#46743=CARTESIAN_POINT('Ctrl Pts',(-0.90718655399813,0.194851447623349,
-1.760475));
#46744=CARTESIAN_POINT('Ctrl Pts',(-0.900223938978484,0.233041812511025,
-1.760475));
#46745=CARTESIAN_POINT('Ctrl Pts',(-0.896568758292669,0.253090699851166,
-1.760475));
#46746=CARTESIAN_POINT('Ctrl Pts',(-0.892250917284448,0.273039973286555,
-1.760475));
#46747=CARTESIAN_POINT('Ctrl Pts',(-0.887279551691811,0.292858392455839,
-1.760475));
#46748=CARTESIAN_POINT('Ctrl Pts',(-0.885185218028628,0.301207483192346,
-1.760475));
#46749=CARTESIAN_POINT('Ctrl Pts',(-0.882974289057405,0.30953537751547,
-1.760475));
#46750=CARTESIAN_POINT('Ctrl Pts',(-0.880649122486369,0.317833204271337,
-1.760475));
#46751=CARTESIAN_POINT('Ctrl Pts',(-0.868801101037989,0.36011526294322,
-1.760475));
#46752=CARTESIAN_POINT('Ctrl Pts',(-0.854043141892115,0.401439171484018,
-1.760475));
#46753=CARTESIAN_POINT('Ctrl Pts',(-0.836535505825568,0.441508132758752,
-1.760475));
#46754=CARTESIAN_POINT('Ctrl Pts',(-0.819027869759021,0.481577094033486,
-1.760475));
#46755=CARTESIAN_POINT('Ctrl Pts',(-0.798770224193348,0.520392501962671,
-1.760475));
#46756=CARTESIAN_POINT('Ctrl Pts',(-0.775863758341581,0.557650930856443,
-1.760475));
#46757=CARTESIAN_POINT('Ctrl Pts',(-0.765346338316838,0.574758002225448,
-1.760475));
#46758=CARTESIAN_POINT('Ctrl Pts',(-0.754269712559982,0.591536614134397,
-1.760475));
#46759=CARTESIAN_POINT('Ctrl Pts',(-0.742655654021007,0.607967592002281,
-1.760475));
#46760=CARTESIAN_POINT('Ctrl Pts',(-0.735908143868069,0.617513625338877,
-1.760475));
#46761=CARTESIAN_POINT('Ctrl Pts',(-0.728979187640245,0.626942295282531,
-1.760475));
#46762=CARTESIAN_POINT('Ctrl Pts',(-0.721872716760233,0.636249606571553,
-1.760475));
#46763=CARTESIAN_POINT('Ctrl Pts',(-0.716795469419606,0.642899253391818,
-1.760475));
#46764=CARTESIAN_POINT('Ctrl Pts',(-0.71162765235188,0.649486685668207,
-1.760475));
#46765=CARTESIAN_POINT('Ctrl Pts',(-0.706379814108373,0.655999601780021,
-1.760475));
#46766=CARTESIAN_POINT('Ctrl Pts',(-0.679428641377427,0.68944779872642,
-1.760475));
#46767=CARTESIAN_POINT('Ctrl Pts',(-0.65031445627706,0.721007357869669,
-1.760475));
#46768=CARTESIAN_POINT('Ctrl Pts',(-0.619290562197985,0.750520252800286,
-1.760475));
#46769=CARTESIAN_POINT('Ctrl Pts',(-0.587986290776079,0.780299869472499,
-1.760475));
#46770=CARTESIAN_POINT('Ctrl Pts',(-0.554736927205615,0.807996564025384,
-1.760475));
#46771=CARTESIAN_POINT('Ctrl Pts',(-0.519757449609006,0.833421359243327,
-1.760475));
#46772=CARTESIAN_POINT('Ctrl Pts',(-0.491766816907548,0.853766320156187,
-1.760475));
#46773=CARTESIAN_POINT('Ctrl Pts',(-0.462667324820022,0.872656204698553,
-1.760475));
#46774=CARTESIAN_POINT('Ctrl Pts',(-0.4325532626849,0.88997606741173,-1.760475));
#46775=CARTESIAN_POINT('Ctrl Pts',(-0.491859688152273,-0.689459403554686,
-1.760475));
#46776=CARTESIAN_POINT('Ctrl Pts',(-0.398395568260706,-0.755994133601717,
-1.75508440548952));
#46777=CARTESIAN_POINT('Ctrl Pts',(-0.16086093226988,-0.861432027295567,
-1.74312605326739));
#46778=CARTESIAN_POINT('Ctrl Pts',(0.2455223736064,-0.847451160704884,-1.72459994333363));
#46779=CARTESIAN_POINT('Ctrl Pts',(0.618741824242655,-0.628975354430863,
-1.7048966701987));
#46780=CARTESIAN_POINT('Ctrl Pts',(0.843308030144031,-0.259391446847321,
-1.68519339706378));
#46781=CARTESIAN_POINT('Ctrl Pts',(0.865269712120719,0.172512904594376,
-1.66549012392885));
#46782=CARTESIAN_POINT('Ctrl Pts',(0.679350192014294,0.562970195790566,
-1.64578685079393));
#46783=CARTESIAN_POINT('Ctrl Pts',(0.330216833785133,0.818174300873478,
-1.626083577659));
#46784=CARTESIAN_POINT('Ctrl Pts',(-0.0982511612190419,0.876811794340843,
-1.60638030452408));
#46785=CARTESIAN_POINT('Ctrl Pts',(-0.503114295254248,0.724795336222326,
-1.58667703138916));
#46786=CARTESIAN_POINT('Ctrl Pts',(-0.782060386406126,0.404439313852934,
-1.56732369992959));
#46787=CARTESIAN_POINT('Ctrl Pts',(-0.846902938248956,0.132306308151429,
-1.55453812618166));
#46788=CARTESIAN_POINT('Ctrl Pts',(-0.846965023971566,-7.48627396995969E-6,
-1.54832031014538));
#46789=CARTESIAN_POINT('Origin',(-9.02152032747242E-17,0.,-1.760475));
#46790=CARTESIAN_POINT('',(-0.989525,-1.21181862392629E-16,-1.760475));
#46791=CARTESIAN_POINT('Origin',(0.,0.,-1.760475));
#46792=CARTESIAN_POINT('Origin',(0.,0.,-1.760475));
#46793=CARTESIAN_POINT('',(0.4918304658226,-0.689450798018774,-1.760475));
#46794=CARTESIAN_POINT('Ctrl Pts',(0.432585265653203,0.889991656643918,
-1.760475));
#46795=CARTESIAN_POINT('Ctrl Pts',(0.45798591835325,0.875415629978971,-1.760475));
#46796=CARTESIAN_POINT('Ctrl Pts',(0.482694780440998,0.859730461206841,
-1.760475));
#46797=CARTESIAN_POINT('Ctrl Pts',(0.506629023856996,0.84296098228689,-1.760475));
#46798=CARTESIAN_POINT('Ctrl Pts',(0.53935338136335,0.820032727825965,-1.760475));
#46799=CARTESIAN_POINT('Ctrl Pts',(0.570631005944284,0.795078082524571,
-1.760475));
#46800=CARTESIAN_POINT('Ctrl Pts',(0.600302577473977,0.768263021275726,
-1.760475));
#46801=CARTESIAN_POINT('Ctrl Pts',(0.610454158722013,0.759088742364806,
-1.760475));
#46802=CARTESIAN_POINT('Ctrl Pts',(0.620417490178586,0.749696503061233,
-1.760475));
#46803=CARTESIAN_POINT('Ctrl Pts',(0.630185343180822,0.740092423589821,
-1.760475));
#46804=CARTESIAN_POINT('Ctrl Pts',(0.637344475756988,0.733053325213531,
-1.760475));
#46805=CARTESIAN_POINT('Ctrl Pts',(0.644397060752394,0.725901766656863,
-1.760475));
#46806=CARTESIAN_POINT('Ctrl Pts',(0.651332664052404,0.718648627745557,
-1.760475));
#46807=CARTESIAN_POINT('Ctrl Pts',(0.681005868927243,0.687616882187022,
-1.760475));
#46808=CARTESIAN_POINT('Ctrl Pts',(0.708583107655331,0.654687253158885,
-1.760475));
#46809=CARTESIAN_POINT('Ctrl Pts',(0.733863523204194,0.620067867414038,
-1.760475));
#46810=CARTESIAN_POINT('Ctrl Pts',(0.751151766686191,0.596393083714486,
-1.760475));
#46811=CARTESIAN_POINT('Ctrl Pts',(0.767365051485111,0.571927361560537,
-1.760475));
#46812=CARTESIAN_POINT('Ctrl Pts',(0.782425995121837,0.546731616997909,
-1.760475));
#46813=CARTESIAN_POINT('Ctrl Pts',(0.787284585117823,0.538603587611031,
-1.760475));
#46814=CARTESIAN_POINT('Ctrl Pts',(0.792023989005052,0.530397840115069,
-1.760475));
#46815=CARTESIAN_POINT('Ctrl Pts',(0.796633225077183,0.522131632421258,
-1.760475));
#46816=CARTESIAN_POINT('Ctrl Pts',(0.803720470973657,0.509421359907429,
-1.760475));
#46817=CARTESIAN_POINT('Ctrl Pts',(0.810504546411578,0.496560849854548,
-1.760475));
#46818=CARTESIAN_POINT('Ctrl Pts',(0.816978165074221,0.483558434025041,
-1.760475));
#46819=CARTESIAN_POINT('Ctrl Pts',(0.835762792526234,0.445829066562774,
-1.760475));
#46820=CARTESIAN_POINT('Ctrl Pts',(0.851937120041244,0.406905973470094,
-1.760475));
#46821=CARTESIAN_POINT('Ctrl Pts',(0.865448139529281,0.367072134072767,
-1.760475));
#46822=CARTESIAN_POINT('Ctrl Pts',(0.878840701435135,0.327587537033374,
-1.760475));
#46823=CARTESIAN_POINT('Ctrl Pts',(0.889616537975764,0.287206908970188,
-1.760475));
#46824=CARTESIAN_POINT('Ctrl Pts',(0.89767373544074,0.246200579867532,-1.760475));
#46825=CARTESIAN_POINT('Ctrl Pts',(0.901076744052898,0.228881295873818,
-1.760475));
#46826=CARTESIAN_POINT('Ctrl Pts',(0.903994163014496,0.211450433808179,
-1.760475));
#46827=CARTESIAN_POINT('Ctrl Pts',(0.906415520733311,0.193928848146053,
-1.760475));
#46828=CARTESIAN_POINT('Ctrl Pts',(0.907539225087183,0.185797425869091,
-1.760475));
#46829=CARTESIAN_POINT('Ctrl Pts',(0.908554772027421,0.177655725181455,
-1.760475));
#46830=CARTESIAN_POINT('Ctrl Pts',(0.909461566888417,0.169507887069413,
-1.760475));
#46831=CARTESIAN_POINT('Ctrl Pts',(0.914011444452751,0.128625800703072,
-1.760475));
#46832=CARTESIAN_POINT('Ctrl Pts',(0.915829911660294,0.0875722848076394,
-1.760475));
#46833=CARTESIAN_POINT('Ctrl Pts',(0.914846868041438,0.046609243460652,
-1.760475));
#46834=CARTESIAN_POINT('Ctrl Pts',(0.914761251370463,0.0430416304210539,
-1.760475));
#46835=CARTESIAN_POINT('Ctrl Pts',(0.91465435174813,0.0394747054990269,
-1.760475));
#46836=CARTESIAN_POINT('Ctrl Pts',(0.914526104044267,0.0359086435694835,
-1.760475));
#46837=CARTESIAN_POINT('Ctrl Pts',(0.913191646411139,-0.0011973506802701,
-1.760475));
#46838=CARTESIAN_POINT('Ctrl Pts',(0.909548495924747,-0.0382108997772076,
-1.760475));
#46839=CARTESIAN_POINT('Ctrl Pts',(0.903640101856299,-0.074922457480337,
-1.760475));
#46840=CARTESIAN_POINT('Ctrl Pts',(0.900537698662256,-0.0941991090640101,
-1.760475));
#46841=CARTESIAN_POINT('Ctrl Pts',(0.89681019627246,-0.113392304066952,
-1.760475));
#46842=CARTESIAN_POINT('Ctrl Pts',(0.89246049865831,-0.132469853078937,
-1.760475));
#46843=CARTESIAN_POINT('Ctrl Pts',(0.890507239189318,-0.141036748196337,
-1.760475));
#46844=CARTESIAN_POINT('Ctrl Pts',(0.888428483231742,-0.149580301912525,
-1.760475));
#46845=CARTESIAN_POINT('Ctrl Pts',(0.886224351701397,-0.158097485205295,
-1.760475));
#46846=CARTESIAN_POINT('Ctrl Pts',(0.884233674210441,-0.165789841507014,
-1.760475));
#46847=CARTESIAN_POINT('Ctrl Pts',(0.882143031893133,-0.173451728693595,
-1.760475));
#46848=CARTESIAN_POINT('Ctrl Pts',(0.879953614149768,-0.181079610448173,
-1.760475));
#46849=CARTESIAN_POINT('Ctrl Pts',(0.868866441708987,-0.219707067737752,
-1.760475));
#46850=CARTESIAN_POINT('Ctrl Pts',(0.855246588377019,-0.257477541532766,
-1.760475));
#46851=CARTESIAN_POINT('Ctrl Pts',(0.839165814934115,-0.294129295903733,
-1.760475));
#46852=CARTESIAN_POINT('Ctrl Pts',(0.82503338612271,-0.326340327997428,
-1.760475));
#46853=CARTESIAN_POINT('Ctrl Pts',(0.808999319325282,-0.357687581877215,
-1.760475));
#46854=CARTESIAN_POINT('Ctrl Pts',(0.79108449509014,-0.387975132360534,
-1.760475));
#46855=CARTESIAN_POINT('Ctrl Pts',(0.781747975332567,-0.403759842820672,
-1.760475));
#46856=CARTESIAN_POINT('Ctrl Pts',(0.771900190824228,-0.419256373417897,
-1.760475));
#46857=CARTESIAN_POINT('Ctrl Pts',(0.761557518747048,-0.434442544451675,
-1.760475));
#46858=CARTESIAN_POINT('Ctrl Pts',(0.754293562385933,-0.445108229572368,
-1.760475));
#46859=CARTESIAN_POINT('Ctrl Pts',(0.746785465653178,-0.45562078837041,
-1.760475));
#46860=CARTESIAN_POINT('Ctrl Pts',(0.739038567160396,-0.465971948253785,
-1.760475));
#46861=CARTESIAN_POINT('Ctrl Pts',(0.734132940351708,-0.472526691093413,
-1.760475));
#46862=CARTESIAN_POINT('Ctrl Pts',(0.729136752700646,-0.479009696834791,
-1.760475));
#46863=CARTESIAN_POINT('Ctrl Pts',(0.724054279914929,-0.485416368873636,
-1.760475));
#46864=CARTESIAN_POINT('Ctrl Pts',(0.699539728324438,-0.516317998619886,
-1.760475));
#46865=CARTESIAN_POINT('Ctrl Pts',(0.673003337176752,-0.545469980344396,
-1.760475));
#46866=CARTESIAN_POINT('Ctrl Pts',(0.644641319797155,-0.572683000469787,
-1.760475));
#46867=CARTESIAN_POINT('Ctrl Pts',(0.616798119179157,-0.599398222050533,
-1.760475));
#46868=CARTESIAN_POINT('Ctrl Pts',(0.587194500700165,-0.624245366063714,
-1.760475));
#46869=CARTESIAN_POINT('Ctrl Pts',(0.555989358652953,-0.647004098426802,
-1.760475));
#46870=CARTESIAN_POINT('Ctrl Pts',(0.535293767266585,-0.662097938562045,
-1.760475));
#46871=CARTESIAN_POINT('Ctrl Pts',(0.513893228447004,-0.676272337278064,
-1.760475));
#46872=CARTESIAN_POINT('Ctrl Pts',(0.491830465822602,-0.689450798018773,
-1.760475));
#46873=CARTESIAN_POINT('Origin',(0.,0.,-1.760475));
#46874=CARTESIAN_POINT('Origin',(0.,0.,-2.22262968985462));
#46875=CARTESIAN_POINT('Ctrl Pts',(0.491830465822599,-0.689450798018774,
-1.760475));
#46876=CARTESIAN_POINT('Ctrl Pts',(0.605635182346436,-0.608266430836124,
-1.75390724228836));
#46877=CARTESIAN_POINT('Ctrl Pts',(0.79216447554976,-0.388547169429118,
-1.74077172686508));
#46878=CARTESIAN_POINT('Ctrl Pts',(0.88161996364164,0.0346345312550622,
-1.72106845373015));
#46879=CARTESIAN_POINT('Ctrl Pts',(0.759268494074124,0.449392048212061,
-1.70136518059523));
#46880=CARTESIAN_POINT('Ctrl Pts',(0.454502118692952,0.756233452283398,
-1.6816619074603));
#46881=CARTESIAN_POINT('Ctrl Pts',(0.0405418686236695,0.881364469834283,
-1.66195863432538));
#46882=CARTESIAN_POINT('Ctrl Pts',(-0.383158700471979,0.79476040598,-1.64225536119046));
#46883=CARTESIAN_POINT('Ctrl Pts',(-0.714805313372813,0.517208687205868,
-1.62255208805553));
#46884=CARTESIAN_POINT('Ctrl Pts',(-0.835534807601658,0.213858991565929,
-1.60767686427692));
#46885=CARTESIAN_POINT('Ctrl Pts',(-0.846921218466673,0.0370517561408366,
-1.59936939820995));
#46886=CARTESIAN_POINT('Ctrl Pts',(-0.846885554371379,2.10899746275542E-5,
-1.59762968985462));
#46887=CARTESIAN_POINT('Ctrl Pts',(0.574658804691352,-0.805560043581921,
-1.84281958214317));
#46888=CARTESIAN_POINT('Ctrl Pts',(0.707629181498825,-0.710703554106881,
-1.83625182443153));
#46889=CARTESIAN_POINT('Ctrl Pts',(0.925571558234001,-0.453981742625281,
-1.82311630900825));
#46890=CARTESIAN_POINT('Ctrl Pts',(1.03009209413448,0.0404672742238311,
-1.80341303587332));
#46891=CARTESIAN_POINT('Ctrl Pts',(0.887135620024441,0.525073404778649,
-1.7837097627384));
#46892=CARTESIAN_POINT('Ctrl Pts',(0.531044053606855,0.883589451966854,
-1.76400648960347));
#46893=CARTESIAN_POINT('Ctrl Pts',(0.0473694563110631,1.02979357304613,
-1.74430321646855));
#46894=CARTESIAN_POINT('Ctrl Pts',(-0.447685810703192,0.928604664927808,
-1.72459994333363));
#46895=CARTESIAN_POINT('Ctrl Pts',(-0.835184470085288,0.60431092951634,
-1.7048966701987));
#46896=CARTESIAN_POINT('Ctrl Pts',(-1.02203007614907,0.134835279898603,
-1.68519339706378));
#46897=CARTESIAN_POINT('Ctrl Pts',(-0.963332906852676,-0.367036471470568,
-1.66549012392885));
#46898=CARTESIAN_POINT('Ctrl Pts',(-0.673194989019042,-0.780726729017107,
-1.64578685079393));
#46899=CARTESIAN_POINT('Ctrl Pts',(-0.221321950521705,-1.00684785792862,
-1.62608357765901));
#46900=CARTESIAN_POINT('Ctrl Pts',(0.283723690388641,-0.991073512081083,
-1.60638030452408));
#46901=CARTESIAN_POINT('Ctrl Pts',(0.720604707801549,-0.737193851560317,
-1.58667703138916));
#46902=CARTESIAN_POINT('Ctrl Pts',(0.984360422706338,-0.306203283667381,
-1.56697375825423));
#46903=CARTESIAN_POINT('Ctrl Pts',(1.01162351797873,0.198352600005484,-1.54727048511931));
#46904=CARTESIAN_POINT('Ctrl Pts',(0.795844033690379,0.655254281948304,
-1.52756721198439));
#46905=CARTESIAN_POINT('Ctrl Pts',(0.388862997423207,0.954731095583577,
-1.50786393884946));
#46906=CARTESIAN_POINT('Ctrl Pts',(-0.111542385241397,1.0248337400704,-1.48816066571454));
#46907=CARTESIAN_POINT('Ctrl Pts',(-0.585149706610647,0.848720046844145,
-1.46845739257961));
#46908=CARTESIAN_POINT('Ctrl Pts',(-0.918174794088913,0.468701338919505,
-1.44875411944469));
#46909=CARTESIAN_POINT('Ctrl Pts',(-1.03060836078115,-0.0239228797397841,
-1.42905084630976));
#46910=CARTESIAN_POINT('Ctrl Pts',(-0.895438239052798,-0.510799625582625,
-1.40934757317484));
#46911=CARTESIAN_POINT('Ctrl Pts',(-0.545139054546205,-0.874956746772044,
-1.38964430003991));
#46912=CARTESIAN_POINT('Ctrl Pts',(-0.0638701964516418,-1.0289054842277,
-1.36994102690499));
#46913=CARTESIAN_POINT('Ctrl Pts',(0.432743478184231,-0.935659649435702,
-1.35023775377007));
#46914=CARTESIAN_POINT('Ctrl Pts',(0.82539051969619,-0.617621556844013,
-1.33053448063514));
#46915=CARTESIAN_POINT('Ctrl Pts',(1.01973746502858,-0.151199867403416,
-1.31083120750022));
#46916=CARTESIAN_POINT('Ctrl Pts',(0.969092454955847,0.351547594549289,
-1.2911279343653));
#46917=CARTESIAN_POINT('Ctrl Pts',(0.685622954609774,0.769835736762807,
-1.27142466123037));
#46918=CARTESIAN_POINT('Ctrl Pts',(0.237432519630045,1.00317082100098,-1.25172138809545));
#46919=CARTESIAN_POINT('Ctrl Pts',(-0.267801085043643,0.995494086539286,
-1.23201811496052));
#46920=CARTESIAN_POINT('Ctrl Pts',(-0.708695471306245,0.748649869054587,
-1.2123148418256));
#46921=CARTESIAN_POINT('Ctrl Pts',(-0.979325750132951,0.321942498921626,
-1.19261156869068));
#46922=CARTESIAN_POINT('Ctrl Pts',(-1.01467298922463,-0.182111565869176,
-1.17290829555575));
#46923=CARTESIAN_POINT('Ctrl Pts',(-0.806245013369315,-0.642413321703791,
-1.15320502242083));
#46924=CARTESIAN_POINT('Ctrl Pts',(-0.404116649781944,-0.948375258457533,
-1.1335017492859));
#46925=CARTESIAN_POINT('Ctrl Pts',(0.0951007505792697,-1.02649001199458,
-1.11379847615098));
#46926=CARTESIAN_POINT('Ctrl Pts',(0.571470192868989,-0.857990510523082,
-1.09409520301605));
#46927=CARTESIAN_POINT('Ctrl Pts',(0.910543904827996,-0.483358764134844,
-1.07439192988113));
#46928=CARTESIAN_POINT('Ctrl Pts',(1.0308594173717,0.00739993928763064,
-1.05468865674621));
#46929=CARTESIAN_POINT('Ctrl Pts',(0.90351092513889,0.496380807082673,-1.03498538361128));
#46930=CARTESIAN_POINT('Ctrl Pts',(0.559093907064072,0.866106171649417,
-1.01528211047636));
#46931=CARTESIAN_POINT('Ctrl Pts',(0.0803545616803817,1.02774950347959,
-0.995578837341433));
#46932=CARTESIAN_POINT('Ctrl Pts',(-0.417689969466237,0.94247598743558,
-0.97587556420651));
#46933=CARTESIAN_POINT('Ctrl Pts',(-0.815384473393104,0.630772588208167,
-0.956172291071584));
#46934=CARTESIAN_POINT('Ctrl Pts',(-1.01718283405342,0.1675260564582,-0.936469017936662));
#46935=CARTESIAN_POINT('Ctrl Pts',(-0.974602989474174,-0.335968615191032,
-0.916765744801736));
#46936=CARTESIAN_POINT('Ctrl Pts',(-0.697874748544491,-0.758746817343798,
-0.897062471666814));
#46937=CARTESIAN_POINT('Ctrl Pts',(-0.253482079134731,-0.999236074730547,
-0.877359198531888));
#46938=CARTESIAN_POINT('Ctrl Pts',(0.251809667103219,-0.999658836323045,
-0.857655925396965));
#46939=CARTESIAN_POINT('Ctrl Pts',(0.69660413355182,-0.75991353363649,-0.837952652262041));
#46940=CARTESIAN_POINT('Ctrl Pts',(0.974039436809005,-0.337598982560928,
-0.818249379127116));
#46941=CARTESIAN_POINT('Ctrl Pts',(1.01746173725982,0.165823733818778,-0.798546105992192));
#46942=CARTESIAN_POINT('Ctrl Pts',(0.816438825967693,0.629407293362469,
-0.778842832857268));
#46943=CARTESIAN_POINT('Ctrl Pts',(0.419266463172544,0.941775732509693,
-0.759139559722345));
#46944=CARTESIAN_POINT('Ctrl Pts',(-0.0786346795008153,1.02788252473966,
-0.739436286587419));
#46945=CARTESIAN_POINT('Ctrl Pts',(-0.557643838154491,0.867040510733896,
-0.719733013452497));
#46946=CARTESIAN_POINT('Ctrl Pts',(-0.902679048596748,0.497891988999522,
-0.700029740317572));
#46947=CARTESIAN_POINT('Ctrl Pts',(-1.03084559156011,0.00912490253774741,
-0.680326467182647));
#46948=CARTESIAN_POINT('Ctrl Pts',(-0.911351451398881,-0.481834442022157,
-0.660623194047724));
#46949=CARTESIAN_POINT('Ctrl Pts',(-0.572905098734823,-0.857033047979255,
-0.640919920912798));
#46950=CARTESIAN_POINT('Ctrl Pts',(-0.0968182795654776,-1.02632943942368,
-0.621216647777876));
#46951=CARTESIAN_POINT('Ctrl Pts',(0.402529134066059,-0.949050153423805,
-0.60151337464295));
#46952=CARTESIAN_POINT('Ctrl Pts',(0.805168911615982,-0.643761540673181,
-0.581810101508027));
#46953=CARTESIAN_POINT('Ctrl Pts',(1.01436683491972,-0.183809199193264,
-0.562106828373103));
#46954=CARTESIAN_POINT('Ctrl Pts',(0.97986309684008,0.320303307693771,-0.542403555238179));
#46955=CARTESIAN_POINT('Ctrl Pts',(0.70994722149712,0.74746293567104,-0.522700282103255));
#46956=CARTESIAN_POINT('Ctrl Pts',(0.269466505632264,0.995044571763327,
-0.50299700896833));
#46957=CARTESIAN_POINT('Ctrl Pts',(-0.23575354585651,1.00356672080292,-0.483293735833407));
#46958=CARTESIAN_POINT('Ctrl Pts',(-0.68433380140946,0.770981936139643,
-0.463590462698482));
#46959=CARTESIAN_POINT('Ctrl Pts',(-0.968502840906551,0.353168719194655,
-0.443887189563558));
#46960=CARTESIAN_POINT('Ctrl Pts',(-1.01998904594358,-0.149493292983739,
-0.424183916428634));
#46961=CARTESIAN_POINT('Ctrl Pts',(-0.826422851232646,-0.616239536706045,
-0.40448064329371));
#46962=CARTESIAN_POINT('Ctrl Pts',(-0.434308546660483,-0.934934214942325,
-0.384777370158786));
#46963=CARTESIAN_POINT('Ctrl Pts',(0.0621484066991229,-1.02901091908753,
-0.365074097023862));
#46964=CARTESIAN_POINT('Ctrl Pts',(0.54367418788479,-0.875867724115407,
-0.345370823888937));
#46965=CARTESIAN_POINT('Ctrl Pts',(0.894582260757255,-0.512297275439298,
-0.325667550754014));
#46966=CARTESIAN_POINT('Ctrl Pts',(1.03056685826814,-0.0256474068051044,
-0.305964277619089));
#46967=CARTESIAN_POINT('Ctrl Pts',(0.918957859857471,0.467164282243796,
-0.286261004484165));
#46968=CARTESIAN_POINT('Ctrl Pts',(0.586568968558927,0.847739679244646,
-0.266557731349241));
#46969=CARTESIAN_POINT('Ctrl Pts',(0.113257341734262,1.02464571211618,-0.246854458214317));
#46970=CARTESIAN_POINT('Ctrl Pts',(-0.387265307077567,0.955380348967222,
-0.227151185079393));
#46971=CARTESIAN_POINT('Ctrl Pts',(-0.794745589415275,0.656585292791054,
-0.207447911944469));
#46972=CARTESIAN_POINT('Ctrl Pts',(-1.01129191299364,0.200044683869197,
-0.187744638809545));
#46973=CARTESIAN_POINT('Ctrl Pts',(-0.984868017254482,-0.304554850671511,
-0.168041365674621));
#46974=CARTESIAN_POINT('Ctrl Pts',(-0.721844019653508,-0.7359886668888,
-0.148338092539697));
#46975=CARTESIAN_POINT('Ctrl Pts',(-0.285368307933075,-0.990594073043749,
-0.128634819404772));
#46976=CARTESIAN_POINT('Ctrl Pts',(0.219610032591509,-1.00722329017286,
-0.108931546269848));
#46977=CARTESIAN_POINT('Ctrl Pts',(0.671944475147084,-0.78183934050936,
-0.0892282731349243));
#46978=CARTESIAN_POINT('Ctrl Pts',(0.865681796314515,-0.506392760472071,
-0.0760927577116414));
#46979=CARTESIAN_POINT('Ctrl Pts',(0.924091453827287,-0.353856906938908,
-0.0695250000000001));
#46980=CARTESIAN_POINT('Ctrl Pts',(0.547049358401768,-0.766856961727539,
-1.81537138809545));
#46981=CARTESIAN_POINT('Ctrl Pts',(0.673631181781362,-0.676557846349963,
-1.80880363038381));
#46982=CARTESIAN_POINT('Ctrl Pts',(0.881102530672586,-0.43217021822656,
-1.79566811496052));
#46983=CARTESIAN_POINT('Ctrl Pts',(0.980601383970203,0.038523026567575,
-1.7759648418256));
#46984=CARTESIAN_POINT('Ctrl Pts',(0.844513244707669,0.49984628592312,-1.75626156869068));
#46985=CARTESIAN_POINT('Ctrl Pts',(0.505530075302221,0.841137452072369,
-1.73655829555575));
#46986=CARTESIAN_POINT('Ctrl Pts',(0.0450935937485983,0.980317205308848,
-1.71685502242083));
#46987=CARTESIAN_POINT('Ctrl Pts',(-0.426176773959454,0.883989911945206,
-1.6971517492859));
#46988=CARTESIAN_POINT('Ctrl Pts',(-0.795058084514463,0.575276848746182,
-1.67744847615098));
#46989=CARTESIAN_POINT('Ctrl Pts',(-0.972926705134103,0.12835712731848,
-1.65774520301605));
#46990=CARTESIAN_POINT('Ctrl Pts',(-0.917049637661276,-0.349402227180467,
-1.63804192988113));
#46991=CARTESIAN_POINT('Ctrl Pts',(-0.640851377923199,-0.743216762206073,
-1.61833865674621));
#46992=CARTESIAN_POINT('Ctrl Pts',(-0.21068855126679,-0.958473915637432,
-1.59863538361128));
#46993=CARTESIAN_POINT('Ctrl Pts',(0.270092203449057,-0.943457447248438,
-1.57893211047636));
#46994=CARTESIAN_POINT('Ctrl Pts',(0.685983299735323,-0.701775419120918,
-1.55922883734143));
#46995=CARTESIAN_POINT('Ctrl Pts',(0.93706688783237,-0.291491766076259,
-1.53952556420651));
#46996=CARTESIAN_POINT('Ctrl Pts',(0.963020129399458,0.188822761757913,
-1.51982229107159));
#46997=CARTESIAN_POINT('Ctrl Pts',(0.757607756922875,0.623772631000333,
-1.50011901793666));
#46998=CARTESIAN_POINT('Ctrl Pts',(0.370180099060361,0.908861099876003,
-1.48041574480174));
#46999=CARTESIAN_POINT('Ctrl Pts',(-0.106183338326614,0.975595667197877,
-1.46071247166681));
#47000=CARTESIAN_POINT('Ctrl Pts',(-0.557036225595229,0.807943345335459,
-1.44100919853189));
#47001=CARTESIAN_POINT('Ctrl Pts',(-0.874061143597708,0.446182612438484,
-1.42130592539696));
#47002=CARTESIAN_POINT('Ctrl Pts',(-0.981092846618151,-0.0227735064805993,
-1.40160265226204));
#47003=CARTESIAN_POINT('Ctrl Pts',(-0.85241696492467,-0.486258289554828,
-1.38189937912712));
#47004=CARTESIAN_POINT('Ctrl Pts',(-0.518947882803987,-0.832919504658114,
-1.36219610599219));
#47005=CARTESIAN_POINT('Ctrl Pts',(-0.0608015568623043,-0.979471784662089,
-1.34249283285727));
#47006=CARTESIAN_POINT('Ctrl Pts',(0.411952344870764,-0.89070594016416,
-1.32278955972234));
#47007=CARTESIAN_POINT('Ctrl Pts',(0.785734683858569,-0.587947967817332,
-1.30308628658742));
#47008=CARTESIAN_POINT('Ctrl Pts',(0.970744242371342,-0.14393547924128,
-1.2833830134525));
#47009=CARTESIAN_POINT('Ctrl Pts',(0.922532468636458,0.334657512381047,
-1.26367974031757));
#47010=CARTESIAN_POINT('Ctrl Pts',(0.652682242685291,0.7328490269927,-1.24397646718265));
#47011=CARTESIAN_POINT('Ctrl Pts',(0.22602508909107,0.954973541718743,-1.22427319404772));
#47012=CARTESIAN_POINT('Ctrl Pts',(-0.254934598680877,0.94766563548359,
-1.2045699209128));
#47013=CARTESIAN_POINT('Ctrl Pts',(-0.67464624176175,0.712681032971984,
-1.18486664777788));
#47014=CARTESIAN_POINT('Ctrl Pts',(-0.932274105787528,0.306474791719114,
-1.16516337464295));
#47015=CARTESIAN_POINT('Ctrl Pts',(-0.965923088990291,-0.173362027089766,
-1.14546010150803));
#47016=CARTESIAN_POINT('Ctrl Pts',(-0.767509022184385,-0.611548613886739,
-1.1257568283731));
#47017=CARTESIAN_POINT('Ctrl Pts',(-0.384700890646618,-0.902810628546715,
-1.10605355523818));
#47018=CARTESIAN_POINT('Ctrl Pts',(0.090531640972349,-0.977172363641172,
-1.08635028210325));
#47019=CARTESIAN_POINT('Ctrl Pts',(0.544013943234757,-0.816768410167404,
-1.06664700896833));
#47020=CARTESIAN_POINT('Ctrl Pts',(0.86679687993353,-0.460135822577115,
-1.04694373583341));
#47021=CARTESIAN_POINT('Ctrl Pts',(0.981331841210531,0.00704440966789899,
-1.02724046269848));
#47022=CARTESIAN_POINT('Ctrl Pts',(0.860101799313222,0.472532222286882,
-1.00753718956356));
#47023=CARTESIAN_POINT('Ctrl Pts',(0.532232275306405,0.824494154863082,
-0.987833916428634));
#47024=CARTESIAN_POINT('Ctrl Pts',(0.0764939317957849,0.978371342936638,
-0.968130643293711));
#47025=CARTESIAN_POINT('Ctrl Pts',(-0.397622081036563,0.897194787631635,
-0.948427370158785));
#47026=CARTESIAN_POINT('Ctrl Pts',(-0.776209377423594,0.600467158703036,
-0.928724097023862));
#47027=CARTESIAN_POINT('Ctrl Pts',(-0.968312348481428,0.159477277565179,
-0.909020823888938));
#47028=CARTESIAN_POINT('Ctrl Pts',(-0.927778249868891,-0.319827024110592,
-0.889317550754013));
#47029=CARTESIAN_POINT('Ctrl Pts',(-0.664345399947551,-0.722292874012854,
-0.86961427761909));
#47030=CARTESIAN_POINT('Ctrl Pts',(-0.241303548514284,-0.951227840086503,
-0.849911004484165));
#47031=CARTESIAN_POINT('Ctrl Pts',(0.239711487414111,-0.951630290124759,
-0.830207731349241));
#47032=CARTESIAN_POINT('Ctrl Pts',(0.663135831572647,-0.723403535494316,
-0.810504458214317));
#47033=CARTESIAN_POINT('Ctrl Pts',(0.927241773056233,-0.321379060582283,
-0.790801185079393));
#47034=CARTESIAN_POINT('Ctrl Pts',(0.968577851800747,0.157856742910379,
-0.771097911944469));
#47035=CARTESIAN_POINT('Ctrl Pts',(0.777213073694752,0.599167459362714,
-0.751394638809544));
#47036=CARTESIAN_POINT('Ctrl Pts',(0.39912283220146,0.896528176409816,-0.73169136567462));
#47037=CARTESIAN_POINT('Ctrl Pts',(-0.0748566812478484,0.978497973198602,
-0.711988092539697));
#47038=CARTESIAN_POINT('Ctrl Pts',(-0.530851874866792,0.825383603684749,
-0.692284819404772));
#47039=CARTESIAN_POINT('Ctrl Pts',(-0.85930989022746,0.473970799563156,
-0.672581546269849));
#47040=CARTESIAN_POINT('Ctrl Pts',(-0.981318679659197,0.00868649716666914,
-0.652878273134924));
#47041=CARTESIAN_POINT('Ctrl Pts',(-0.867565627979979,-0.458684736424889,
-0.633175000000001));
#47042=CARTESIAN_POINT('Ctrl Pts',(-0.545379909138111,-0.815856948851546,
-0.613471726865076));
#47043=CARTESIAN_POINT('Ctrl Pts',(-0.0921666513859544,-0.977019505769383,
-0.593768453730152));
#47044=CARTESIAN_POINT('Ctrl Pts',(0.383189647023903,-0.90345309822659,
-0.574065180595227));
#47045=CARTESIAN_POINT('Ctrl Pts',(0.766484621672412,-0.612832057760162,
-0.554361907460304));
#47046=CARTESIAN_POINT('Ctrl Pts',(0.965631643849792,-0.174978097727091,
-0.534658634325379));
#47047=CARTESIAN_POINT('Ctrl Pts',(0.932785635705759,0.304914355331165,
-0.514955361190455));
#47048=CARTESIAN_POINT('Ctrl Pts',(0.67583785169308,0.711551125728532,-0.495252088055531));
#47049=CARTESIAN_POINT('Ctrl Pts',(0.256520004241595,0.947237717616896,
-0.475548814920607));
#47050=CARTESIAN_POINT('Ctrl Pts',(-0.224426781507358,0.955350420539488,
-0.455845541785683));
#47051=CARTESIAN_POINT('Ctrl Pts',(-0.651455026769769,0.733940157292244,
-0.436142268650759));
#47052=CARTESIAN_POINT('Ctrl Pts',(-0.921971182557243,0.336200750194329,
-0.416438995515835));
#47053=CARTESIAN_POINT('Ctrl Pts',(-0.970983736097037,-0.142310897082741,
-0.396735722380911));
#47054=CARTESIAN_POINT('Ctrl Pts',(-0.786717417090993,-0.586632346750361,
-0.377032449245986));
#47055=CARTESIAN_POINT('Ctrl Pts',(-0.413442219730069,-0.890015359125594,
-0.357329176111063));
#47056=CARTESIAN_POINT('Ctrl Pts',(0.0591624903906386,-0.979572153910683,
-0.337625902976138));
#47057=CARTESIAN_POINT('Ctrl Pts',(0.5175533955696,-0.833786714152053,-0.317922629841214));
#47058=CARTESIAN_POINT('Ctrl Pts',(0.851602112052742,-0.48768398491791,
-0.29821935670629));
#47059=CARTESIAN_POINT('Ctrl Pts',(0.98105333809078,-0.0244151787510444,
-0.278516083571366));
#47060=CARTESIAN_POINT('Ctrl Pts',(0.874806587020447,0.444719403554519,
-0.258812810436442));
#47061=CARTESIAN_POINT('Ctrl Pts',(0.558387299192069,0.807010079435893,
-0.239109537301518));
#47062=CARTESIAN_POINT('Ctrl Pts',(0.107815899842159,0.975416673034951,
-0.219406264166593));
#47063=CARTESIAN_POINT('Ctrl Pts',(-0.36865916964734,0.909479159921484,
-0.19970299103167));
#47064=CARTESIAN_POINT('Ctrl Pts',(-0.756562087334191,0.625039693510482,
-0.179999717896746));
#47065=CARTESIAN_POINT('Ctrl Pts',(-0.962704456355113,0.190433549558341,
-0.160296444761821));
#47066=CARTESIAN_POINT('Ctrl Pts',(-0.93755009503223,-0.289922531940463,
-0.140593171626897));
#47067=CARTESIAN_POINT('Ctrl Pts',(-0.687163068926953,-0.700628137471483,
-0.120889898491973));
#47068=CARTESIAN_POINT('Ctrl Pts',(-0.271657805446542,-0.943001042829635,
-0.101186625357049));
#47069=CARTESIAN_POINT('Ctrl Pts',(0.209058882326361,-0.958831310262997,
-0.0814833522221245));
#47070=CARTESIAN_POINT('Ctrl Pts',(0.63966094491192,-0.744275918348846,
-0.0617800790872008));
#47071=CARTESIAN_POINT('Ctrl Pts',(0.824090168614572,-0.482063152002576,
-0.0486445636639179));
#47072=CARTESIAN_POINT('Ctrl Pts',(0.879693537789418,-0.336855874001501,
-0.0420768059522765));
#47073=CARTESIAN_POINT('Ctrl Pts',(0.519439912112184,-0.728153879873157,
-1.78792319404772));
#47074=CARTESIAN_POINT('Ctrl Pts',(0.639633182063899,-0.642412138593043,
-1.78135543633608));
#47075=CARTESIAN_POINT('Ctrl Pts',(0.836633503111173,-0.410358693827839,
-1.7682199209128));
#47076=CARTESIAN_POINT('Ctrl Pts',(0.931110673805921,0.0365787789113189,
-1.74851664777787));
#47077=CARTESIAN_POINT('Ctrl Pts',(0.801890869390896,0.47461916706759,-1.72881337464295));
#47078=CARTESIAN_POINT('Ctrl Pts',(0.480016096997586,0.798685452177885,
-1.70911010150802));
#47079=CARTESIAN_POINT('Ctrl Pts',(0.0428177311861338,0.930840837571564,
-1.68940682837311));
#47080=CARTESIAN_POINT('Ctrl Pts',(-0.404667737215717,0.839375158962604,
-1.66970355523818));
#47081=CARTESIAN_POINT('Ctrl Pts',(-0.754931698943638,0.546242767976024,
-1.65000028210326));
#47082=CARTESIAN_POINT('Ctrl Pts',(-0.923823334119134,0.121878974738357,
-1.63029700896833));
#47083=CARTESIAN_POINT('Ctrl Pts',(-0.870766368469874,-0.331767982890366,
-1.61059373583341));
#47084=CARTESIAN_POINT('Ctrl Pts',(-0.608507766827356,-0.705706795395039,
-1.59089046269848));
#47085=CARTESIAN_POINT('Ctrl Pts',(-0.200055152011874,-0.910099973346243,
-1.57118718956356));
#47086=CARTESIAN_POINT('Ctrl Pts',(0.256460716509473,-0.895841382415795,
-1.55148391642863));
#47087=CARTESIAN_POINT('Ctrl Pts',(0.651361891669097,-0.666356986681518,
-1.53178064329371));
#47088=CARTESIAN_POINT('Ctrl Pts',(0.889773352958402,-0.276780248485138,
-1.51207737015879));
#47089=CARTESIAN_POINT('Ctrl Pts',(0.914416740820184,0.179292923510344,
-1.49237409702386));
#47090=CARTESIAN_POINT('Ctrl Pts',(0.719371480155372,0.592290980052361,
-1.47267082388894));
#47091=CARTESIAN_POINT('Ctrl Pts',(0.351497200697514,0.862991104168431,
-1.45296755075401));
#47092=CARTESIAN_POINT('Ctrl Pts',(-0.100824291411831,0.926357594325357,
-1.43326427761909));
#47093=CARTESIAN_POINT('Ctrl Pts',(-0.528922744579813,0.767166643826773,
-1.41356100448417));
#47094=CARTESIAN_POINT('Ctrl Pts',(-0.829947493106503,0.423663885957463,
-1.39385773134924));
#47095=CARTESIAN_POINT('Ctrl Pts',(-0.931577332455155,-0.0216241332214148,
-1.37415445821432));
#47096=CARTESIAN_POINT('Ctrl Pts',(-0.809395690796543,-0.46171695352703,
-1.35445118507939));
#47097=CARTESIAN_POINT('Ctrl Pts',(-0.492756711061769,-0.790882262544183,
-1.33474791194447));
#47098=CARTESIAN_POINT('Ctrl Pts',(-0.0577329172729664,-0.930038085096481,
-1.31504463880955));
#47099=CARTESIAN_POINT('Ctrl Pts',(0.391161211557297,-0.845752230892618,
-1.29534136567462));
#47100=CARTESIAN_POINT('Ctrl Pts',(0.746078848020947,-0.558274378790652,
-1.2756380925397));
#47101=CARTESIAN_POINT('Ctrl Pts',(0.921751019714107,-0.136671091079143,
-1.25593481940477));
#47102=CARTESIAN_POINT('Ctrl Pts',(0.87597248231707,0.317767430212804,-1.23623154626985));
#47103=CARTESIAN_POINT('Ctrl Pts',(0.619741530760809,0.695862317222595,
-1.21652827313492));
#47104=CARTESIAN_POINT('Ctrl Pts',(0.214617658552094,0.906776262436506,
-1.196825));
#47105=CARTESIAN_POINT('Ctrl Pts',(-0.242068112318111,0.899837184427893,
-1.17712172686508));
#47106=CARTESIAN_POINT('Ctrl Pts',(-0.640597012217254,0.67671219688938,
-1.15741845373015));
#47107=CARTESIAN_POINT('Ctrl Pts',(-0.885222461442106,0.291007084516601,
-1.13771518059523));
#47108=CARTESIAN_POINT('Ctrl Pts',(-0.917173188755948,-0.164612488310355,
-1.1180119074603));
#47109=CARTESIAN_POINT('Ctrl Pts',(-0.728773030999457,-0.58068390606969,
-1.09830863432538));
#47110=CARTESIAN_POINT('Ctrl Pts',(-0.36528513151129,-0.857245998635898,
-1.07860536119046));
#47111=CARTESIAN_POINT('Ctrl Pts',(0.0859625313654273,-0.927854715287762,
-1.05890208805553));
#47112=CARTESIAN_POINT('Ctrl Pts',(0.516557693600527,-0.775546309811726,
-1.03919881492061));
#47113=CARTESIAN_POINT('Ctrl Pts',(0.823049855039062,-0.436912881019387,
-1.01949554178568));
#47114=CARTESIAN_POINT('Ctrl Pts',(0.931804265049363,0.00668888004816687,
-0.999792268650759));
#47115=CARTESIAN_POINT('Ctrl Pts',(0.816692673487552,0.448683637491092,
-0.980088995515835));
#47116=CARTESIAN_POINT('Ctrl Pts',(0.505370643548739,0.782882138076745,
-0.96038572238091));
#47117=CARTESIAN_POINT('Ctrl Pts',(0.0726333019111879,0.928993182393693,
-0.940682449245987));
#47118=CARTESIAN_POINT('Ctrl Pts',(-0.377554192606889,0.851913587827687,
-0.920979176111061));
#47119=CARTESIAN_POINT('Ctrl Pts',(-0.737034281454082,0.570161729197906,
-0.901275902976139));
#47120=CARTESIAN_POINT('Ctrl Pts',(-0.919441862909439,0.151428498672156,
-0.881572629841214));
#47121=CARTESIAN_POINT('Ctrl Pts',(-0.880953510263607,-0.303685433030151,
-0.86186935670629));
#47122=CARTESIAN_POINT('Ctrl Pts',(-0.630816051350612,-0.68583893068191,
-0.842166083571366));
#47123=CARTESIAN_POINT('Ctrl Pts',(-0.229125017893837,-0.903219605442459,
-0.822462810436442));
#47124=CARTESIAN_POINT('Ctrl Pts',(0.227613307725003,-0.903601743926474,
-0.802759537301517));
#47125=CARTESIAN_POINT('Ctrl Pts',(0.629667529593472,-0.686893537352141,
-0.783056264166594));
#47126=CARTESIAN_POINT('Ctrl Pts',(0.880444109303463,-0.305159138603638,
-0.763352991031669));
#47127=CARTESIAN_POINT('Ctrl Pts',(0.919693966341668,0.14988975200198,-0.743649717896745));
#47128=CARTESIAN_POINT('Ctrl Pts',(0.737987321421813,0.56892762536296,-0.723946444761821));
#47129=CARTESIAN_POINT('Ctrl Pts',(0.378979201230375,0.851280620309938,
-0.704243171626897));
#47130=CARTESIAN_POINT('Ctrl Pts',(-0.0710786829948813,0.929113421657545,
-0.684539898491973));
#47131=CARTESIAN_POINT('Ctrl Pts',(-0.504059911579092,0.783726696635601,
-0.664836625357049));
#47132=CARTESIAN_POINT('Ctrl Pts',(-0.815940731858172,0.450049610126791,
-0.645133352222125));
#47133=CARTESIAN_POINT('Ctrl Pts',(-0.931791767758281,0.00824809179559103,
-0.6254300790872));
#47134=CARTESIAN_POINT('Ctrl Pts',(-0.823779804561077,-0.435535030827622,
-0.605726805952277));
#47135=CARTESIAN_POINT('Ctrl Pts',(-0.5178547195414,-0.774680849723837,
-0.586023532817352));
#47136=CARTESIAN_POINT('Ctrl Pts',(-0.0875150232064309,-0.927709572115086,
-0.566320259682429));
#47137=CARTESIAN_POINT('Ctrl Pts',(0.363850159981747,-0.857856043029375,
-0.546616986547504));
#47138=CARTESIAN_POINT('Ctrl Pts',(0.727800331728844,-0.581902574847143,
-0.52691371341258));
#47139=CARTESIAN_POINT('Ctrl Pts',(0.91689645277986,-0.16614699626092,-0.507210440277656));
#47140=CARTESIAN_POINT('Ctrl Pts',(0.885708174571438,0.28952540296856,-0.487507167142732));
#47141=CARTESIAN_POINT('Ctrl Pts',(0.64172848188904,0.675639315786023,-0.467803894007807));
#47142=CARTESIAN_POINT('Ctrl Pts',(0.243573502850927,0.899430863470464,
-0.448100620872884));
#47143=CARTESIAN_POINT('Ctrl Pts',(-0.213100017158207,0.907134120276057,
-0.428397347737959));
#47144=CARTESIAN_POINT('Ctrl Pts',(-0.618576252130077,0.696898378444844,
-0.408694074603035));
#47145=CARTESIAN_POINT('Ctrl Pts',(-0.875439524207936,0.319232781194004,
-0.388990801468111));
#47146=CARTESIAN_POINT('Ctrl Pts',(-0.921978426250493,-0.135128501181744,
-0.369287528333187));
#47147=CARTESIAN_POINT('Ctrl Pts',(-0.74701198294934,-0.557025156794675,
-0.349584255198263));
#47148=CARTESIAN_POINT('Ctrl Pts',(-0.392575892799654,-0.845096503308866,
-0.329880982063339));
#47149=CARTESIAN_POINT('Ctrl Pts',(0.0561765740821534,-0.930133388733834,
-0.310177708928415));
#47150=CARTESIAN_POINT('Ctrl Pts',(0.49143260325441,-0.791705704188701,
-0.29047443579349));
#47151=CARTESIAN_POINT('Ctrl Pts',(0.808621963348227,-0.46307069439652,
-0.270771162658566));
#47152=CARTESIAN_POINT('Ctrl Pts',(0.931539817913425,-0.0231829506969853,
-0.251067889523642));
#47153=CARTESIAN_POINT('Ctrl Pts',(0.830655314183421,0.422274524865243,
-0.231364616388718));
#47154=CARTESIAN_POINT('Ctrl Pts',(0.530205629825212,0.766280479627141,
-0.211661343253794));
#47155=CARTESIAN_POINT('Ctrl Pts',(0.102374457950055,0.926187633953719,
-0.19195807011887));
#47156=CARTESIAN_POINT('Ctrl Pts',(-0.350053032217113,0.863577970875746,
-0.172254796983946));
#47157=CARTESIAN_POINT('Ctrl Pts',(-0.718378585253108,0.593494094229909,
-0.152551523849022));
#47158=CARTESIAN_POINT('Ctrl Pts',(-0.914116999716585,0.180822415247486,
-0.132848250714098));
#47159=CARTESIAN_POINT('Ctrl Pts',(-0.890232172809978,-0.275290213209414,
-0.113144977579174));
#47160=CARTESIAN_POINT('Ctrl Pts',(-0.652482118200398,-0.665267608054165,
-0.0934417044442497));
#47161=CARTESIAN_POINT('Ctrl Pts',(-0.25794730296001,-0.895408012615521,
-0.0737384313093254));
#47162=CARTESIAN_POINT('Ctrl Pts',(0.198507732061213,-0.91043933035314,
-0.054035158174401));
#47163=CARTESIAN_POINT('Ctrl Pts',(0.607377414676756,-0.706712496188332,
-0.0343318850394772));
#47164=CARTESIAN_POINT('Ctrl Pts',(0.78249854091463,-0.457733543533081,
-0.0211963696161944));
#47165=CARTESIAN_POINT('Ctrl Pts',(0.835295621751549,-0.319854841064094,
-0.014628611904553));
#47166=CARTESIAN_POINT('Ctrl Pts',(0.491830465822599,-0.689450798018774,
-1.760475));
#47167=CARTESIAN_POINT('Ctrl Pts',(0.605635182346436,-0.608266430836124,
-1.75390724228836));
#47168=CARTESIAN_POINT('Ctrl Pts',(0.79216447554976,-0.388547169429118,
-1.74077172686508));
#47169=CARTESIAN_POINT('Ctrl Pts',(0.88161996364164,0.0346345312550622,
-1.72106845373015));
#47170=CARTESIAN_POINT('Ctrl Pts',(0.759268494074124,0.449392048212061,
-1.70136518059523));
#47171=CARTESIAN_POINT('Ctrl Pts',(0.454502118692952,0.756233452283398,
-1.6816619074603));
#47172=CARTESIAN_POINT('Ctrl Pts',(0.0405418686236695,0.881364469834283,
-1.66195863432538));
#47173=CARTESIAN_POINT('Ctrl Pts',(-0.383158700471979,0.79476040598,-1.64225536119046));
#47174=CARTESIAN_POINT('Ctrl Pts',(-0.714805313372813,0.517208687205868,
-1.62255208805553));
#47175=CARTESIAN_POINT('Ctrl Pts',(-0.874719963104165,0.115400822158233,
-1.60284881492061));
#47176=CARTESIAN_POINT('Ctrl Pts',(-0.824483099278473,-0.314133738600265,
-1.58314554178568));
#47177=CARTESIAN_POINT('Ctrl Pts',(-0.576164155731512,-0.668196828584006,
-1.56344226865076));
#47178=CARTESIAN_POINT('Ctrl Pts',(-0.189421752756959,-0.861726031055052,
-1.54373899551583));
#47179=CARTESIAN_POINT('Ctrl Pts',(0.242829229569888,-0.848225317583151,
-1.52403572238091));
#47180=CARTESIAN_POINT('Ctrl Pts',(0.616740483602872,-0.630938554242118,
-1.50433244924599));
#47181=CARTESIAN_POINT('Ctrl Pts',(0.842479818084434,-0.262068730894017,
-1.48462917611106));
#47182=CARTESIAN_POINT('Ctrl Pts',(0.865813352240911,0.169763085262774,
-1.46492590297614));
#47183=CARTESIAN_POINT('Ctrl Pts',(0.681135203387868,0.560809329104389,
-1.44522262984121));
#47184=CARTESIAN_POINT('Ctrl Pts',(0.332814302334667,0.81712110846086,-1.42551935670629));
#47185=CARTESIAN_POINT('Ctrl Pts',(-0.0954652444970479,0.877119521452837,
-1.40581608357137));
#47186=CARTESIAN_POINT('Ctrl Pts',(-0.500809263564396,0.726389942318086,
-1.38611281043644));
#47187=CARTESIAN_POINT('Ctrl Pts',(-0.785833842615297,0.401145159476442,
-1.36640953730152));
#47188=CARTESIAN_POINT('Ctrl Pts',(-0.882061818292162,-0.0204747599622306,
-1.34670626416659));
#47189=CARTESIAN_POINT('Ctrl Pts',(-0.766374416668415,-0.437175617499231,
-1.32700299103167));
#47190=CARTESIAN_POINT('Ctrl Pts',(-0.466565539319551,-0.748845020430254,
-1.30729971789674));
#47191=CARTESIAN_POINT('Ctrl Pts',(-0.0546642776836284,-0.880604385530872,
-1.28759644476182));
#47192=CARTESIAN_POINT('Ctrl Pts',(0.37037007824383,-0.800798521621077,
-1.2678931716269));
#47193=CARTESIAN_POINT('Ctrl Pts',(0.706423012183327,-0.52860078976397,
-1.24818989849197));
#47194=CARTESIAN_POINT('Ctrl Pts',(0.872757797056872,-0.129406702917007,
-1.22848662535705));
#47195=CARTESIAN_POINT('Ctrl Pts',(0.829412495997682,0.300877348044562,
-1.20878335222212));
#47196=CARTESIAN_POINT('Ctrl Pts',(0.586800818836326,0.658875607452487,
-1.1890800790872));
#47197=CARTESIAN_POINT('Ctrl Pts',(0.20321022801312,0.858578983154271,-1.16937680595228));
#47198=CARTESIAN_POINT('Ctrl Pts',(-0.229201625955346,0.852008733372195,
-1.14967353281735));
#47199=CARTESIAN_POINT('Ctrl Pts',(-0.606547782672759,0.640743360806779,
-1.12997025968243));
#47200=CARTESIAN_POINT('Ctrl Pts',(-0.838170817096684,0.275539377314088,
-1.11026698654751));
#47201=CARTESIAN_POINT('Ctrl Pts',(-0.868423288521605,-0.155862949530944,
-1.09056371341258));
#47202=CARTESIAN_POINT('Ctrl Pts',(-0.690037039814528,-0.549819198252638,
-1.07086044027766));
#47203=CARTESIAN_POINT('Ctrl Pts',(-0.345869372375964,-0.811681368725081,
-1.05115716714273));
#47204=CARTESIAN_POINT('Ctrl Pts',(0.0813934217585064,-0.878537066934349,
-1.03145389400781));
#47205=CARTESIAN_POINT('Ctrl Pts',(0.489101443966296,-0.734324209456049,
-1.01175062087288));
#47206=CARTESIAN_POINT('Ctrl Pts',(0.779302830144596,-0.413689939461657,
-0.99204734773796));
#47207=CARTESIAN_POINT('Ctrl Pts',(0.882276688888196,0.00633335042843485,
-0.972344074603035));
#47208=CARTESIAN_POINT('Ctrl Pts',(0.773283547661882,0.424835052695301,
-0.952640801468111));
#47209=CARTESIAN_POINT('Ctrl Pts',(0.478509011791072,0.74127012129041,-0.932937528333187));
#47210=CARTESIAN_POINT('Ctrl Pts',(0.0687726720265907,0.879615021850747,
-0.913234255198264));
#47211=CARTESIAN_POINT('Ctrl Pts',(-0.357486304177214,0.806632388023741,
-0.893530982063338));
#47212=CARTESIAN_POINT('Ctrl Pts',(-0.697859185484572,0.539856299692775,
-0.873827708928416));
#47213=CARTESIAN_POINT('Ctrl Pts',(-0.870571377337449,0.143379719779135,
-0.85412443579349));
#47214=CARTESIAN_POINT('Ctrl Pts',(-0.834128770658324,-0.287543841949712,
-0.834421162658567));
#47215=CARTESIAN_POINT('Ctrl Pts',(-0.597286702753671,-0.649384987350965,
-0.814717889523642));
#47216=CARTESIAN_POINT('Ctrl Pts',(-0.21694648727339,-0.855211370798415,
-0.795014616388718));
#47217=CARTESIAN_POINT('Ctrl Pts',(0.215515128035896,-0.855573197728189,
-0.775311343253795));
#47218=CARTESIAN_POINT('Ctrl Pts',(0.596199227614297,-0.650383539209966,
-0.75560807011887));
#47219=CARTESIAN_POINT('Ctrl Pts',(0.833646445550691,-0.288939216624994,
-0.735904796983946));
#47220=CARTESIAN_POINT('Ctrl Pts',(0.870810080882589,0.141922761093581,
-0.716201523849022));
#47221=CARTESIAN_POINT('Ctrl Pts',(0.698761569148873,0.538687791363206,
-0.696498250714097));
#47222=CARTESIAN_POINT('Ctrl Pts',(0.358835570259291,0.806033064210061,
-0.676794977579174));
#47223=CARTESIAN_POINT('Ctrl Pts',(-0.0673006847419141,0.879728870116488,
-0.657091704444249));
#47224=CARTESIAN_POINT('Ctrl Pts',(-0.477267948291393,0.742069789586453,
-0.637388431309326));
#47225=CARTESIAN_POINT('Ctrl Pts',(-0.772571573488883,0.426128420690425,
-0.617685158174401));
#47226=CARTESIAN_POINT('Ctrl Pts',(-0.882264855857366,0.00780968642451235,
-0.597981885039478));
#47227=CARTESIAN_POINT('Ctrl Pts',(-0.779993981142175,-0.412385325230355,
-0.578278611904553));
#47228=CARTESIAN_POINT('Ctrl Pts',(-0.490329529944689,-0.733504750596127,
-0.558575338769629));
#47229=CARTESIAN_POINT('Ctrl Pts',(-0.0828633950269074,-0.878399638460791,
-0.538872065634705));
#47230=CARTESIAN_POINT('Ctrl Pts',(0.344510672939591,-0.812258987832161,
-0.51916879249978));
#47231=CARTESIAN_POINT('Ctrl Pts',(0.689116041785277,-0.550973091934125,
-0.499465519364857));
#47232=CARTESIAN_POINT('Ctrl Pts',(0.868161261709926,-0.157315894794747,
-0.479762246229933));
#47233=CARTESIAN_POINT('Ctrl Pts',(0.838630713437117,0.274136450605954,
-0.460058973095008));
#47234=CARTESIAN_POINT('Ctrl Pts',(0.607619112085,0.639727505843516,-0.440355699960084));
#47235=CARTESIAN_POINT('Ctrl Pts',(0.230627001460258,0.851624009324031,
-0.42065242682516));
#47236=CARTESIAN_POINT('Ctrl Pts',(-0.201773252809055,0.858917820012625,
-0.400949153690236));
#47237=CARTESIAN_POINT('Ctrl Pts',(-0.585697477490385,0.659856599597445,
-0.381245880555312));
#47238=CARTESIAN_POINT('Ctrl Pts',(-0.828907865858628,0.302264812193679,
-0.361542607420387));
#47239=CARTESIAN_POINT('Ctrl Pts',(-0.872973116403949,-0.127946105280747,
-0.341839334285464));
#47240=CARTESIAN_POINT('Ctrl Pts',(-0.707306548807687,-0.52741796683899,
-0.322136061150539));
#47241=CARTESIAN_POINT('Ctrl Pts',(-0.37170956586924,-0.800177647492136,
-0.302432788015616));
#47242=CARTESIAN_POINT('Ctrl Pts',(0.053190657773669,-0.880694623556987,
-0.282729514880691));
#47243=CARTESIAN_POINT('Ctrl Pts',(0.46531181093922,-0.749624694225347,
-0.263026241745767));
#47244=CARTESIAN_POINT('Ctrl Pts',(0.765641814643713,-0.438457403875131,
-0.243322968610843));
#47245=CARTESIAN_POINT('Ctrl Pts',(0.88202629773607,-0.0219507226429252,
-0.223619695475919));
#47246=CARTESIAN_POINT('Ctrl Pts',(0.786504041346395,0.399829646175967,
-0.203916422340995));
#47247=CARTESIAN_POINT('Ctrl Pts',(0.502023960458353,0.725550879818389,
-0.184213149206071));
#47248=CARTESIAN_POINT('Ctrl Pts',(0.0969330160579518,0.876958594872486,
-0.164509876071146));
#47249=CARTESIAN_POINT('Ctrl Pts',(-0.331446894786887,0.817676781830008,
-0.144806602936223));
#47250=CARTESIAN_POINT('Ctrl Pts',(-0.680195083172024,0.561948494949336,
-0.125103329801299));
#47251=CARTESIAN_POINT('Ctrl Pts',(-0.865529543078058,0.171211280936631,
-0.105400056666374));
#47252=CARTESIAN_POINT('Ctrl Pts',(-0.842914250587726,-0.260657894478366,
-0.08569678353145));
#47253=CARTESIAN_POINT('Ctrl Pts',(-0.617801167473842,-0.629907078636848,
-0.0659935103965262));
#47254=CARTESIAN_POINT('Ctrl Pts',(-0.244236800473478,-0.847814982401407,
-0.0462902372616019));
#47255=CARTESIAN_POINT('Ctrl Pts',(0.187956581796065,-0.862047350443283,
-0.0265869641266775));
#47256=CARTESIAN_POINT('Ctrl Pts',(0.575093884441593,-0.669149074027817,
-0.00688369099175378));
#47257=CARTESIAN_POINT('Ctrl Pts',(0.740906913214688,-0.433403935063586,
0.0062518244315291));
#47258=CARTESIAN_POINT('Ctrl Pts',(0.790897705713681,-0.302853808126686,
0.0128195821431705));
#47259=CARTESIAN_POINT('Ctrl Pts',(0.924091453827287,-0.353856906938908,
-0.0695250000000001));
#47260=CARTESIAN_POINT('Ctrl Pts',(0.865681796314515,-0.506392760472071,
-0.0760927577116414));
#47261=CARTESIAN_POINT('Ctrl Pts',(0.768813135730799,-0.644116050490716,
-0.0826605154232829));
#47262=CARTESIAN_POINT('Ctrl Pts',(0.644989731679679,-0.750541687110621,
-0.0892282731349242));
#47263=CARTESIAN_POINT('Ctrl Pts',(0.521166327628559,-0.856967323730525,
-0.0957960308465655));
#47264=CARTESIAN_POINT('Ctrl Pts',(0.370388180110033,-0.93209530695169,
-0.102363788558207));
#47265=CARTESIAN_POINT('Ctrl Pts',(0.210836049596674,-0.966887762374088,
-0.108931546269848));
#47266=CARTESIAN_POINT('Ctrl Pts',(0.0512839190833129,-1.00168021779649,
-0.11549930398149));
#47267=CARTESIAN_POINT('Ctrl Pts',(-0.117042194424879,-0.996137145420118,
-0.122067061693131));
#47268=CARTESIAN_POINT('Ctrl Pts',(-0.273951203132383,-0.950931374872775,
-0.128634819404772));
#47269=CARTESIAN_POINT('Ctrl Pts',(-0.430860211839885,-0.905725604325433,
-0.135202577116414));
#47270=CARTESIAN_POINT('Ctrl Pts',(-0.576352115746697,-0.820857135607116,
-0.141770334828055));
#47271=CARTESIAN_POINT('Ctrl Pts',(-0.692935400633598,-0.706517265211744,
-0.148338092539697));
#47272=CARTESIAN_POINT('Ctrl Pts',(-0.809518685520499,-0.592177394816371,
-0.154905850251338));
#47273=CARTESIAN_POINT('Ctrl Pts',(-0.897193351387491,-0.44836612274394,
-0.161473607962979));
#47274=CARTESIAN_POINT('Ctrl Pts',(-0.94543466694418,-0.292360564284275,
-0.168041365674621));
#47275=CARTESIAN_POINT('Ctrl Pts',(-0.974651086749275,-0.19787881486909,
-0.172019001115677));
#47276=CARTESIAN_POINT('Ctrl Pts',(-0.98940380726374,-0.0989243414783639,
-0.175996636556733));
#47277=CARTESIAN_POINT('Ctrl Pts',(-0.989456987247134,1.47486280241971E-5,
-0.17997427199779));
#47278=CARTESIAN_POINT('Origin',(0.,0.,-0.799));
#47279=CARTESIAN_POINT('',(0.288675134594813,-0.5,-0.799));
#47280=CARTESIAN_POINT('',(-0.288675134594813,-0.5,-0.799));
#47281=CARTESIAN_POINT('',(0.144337567297406,-0.5,-0.799));
#47282=CARTESIAN_POINT('Origin',(0.,0.,-0.799));
#47283=CARTESIAN_POINT('Origin',(0.,0.,-0.799));
#47284=CARTESIAN_POINT('',(-0.577350269189626,2.77555756156289E-16,-0.799));
#47285=CARTESIAN_POINT('',(-0.360843918243516,-0.375,-0.799));
#47286=CARTESIAN_POINT('Origin',(0.,0.,-0.799));
#47287=CARTESIAN_POINT('Origin',(0.,0.,-0.799));
#47288=CARTESIAN_POINT('',(-0.288675134594813,0.5,-0.799));
#47289=CARTESIAN_POINT('',(-0.505181485540923,0.125,-0.799));
#47290=CARTESIAN_POINT('Origin',(0.,0.,-0.799));
#47291=CARTESIAN_POINT('Origin',(0.,0.,-0.799));
#47292=CARTESIAN_POINT('',(0.288675134594813,0.5,-0.799));
#47293=CARTESIAN_POINT('',(-0.144337567297406,0.5,-0.799));
#47294=CARTESIAN_POINT('Origin',(0.,0.,-0.799));
#47295=CARTESIAN_POINT('Origin',(0.,0.,-0.799));
#47296=CARTESIAN_POINT('',(0.577350269189626,0.,-0.799));
#47297=CARTESIAN_POINT('',(0.360843918243516,0.375,-0.799));
#47298=CARTESIAN_POINT('Origin',(0.,0.,-0.799));
#47299=CARTESIAN_POINT('Origin',(0.,0.,-0.799));
#47300=CARTESIAN_POINT('',(0.505181485540923,-0.125,-0.799));
#47301=CARTESIAN_POINT('Origin',(0.,0.,-0.799));
#47302=CARTESIAN_POINT('Origin',(0.,0.,-0.972705080756888));
#47303=CARTESIAN_POINT('',(0.,0.,-1.14641016151378));
#47304=CARTESIAN_POINT('',(-0.575688399926292,-7.05014956275995E-17,-0.8));
#47305=CARTESIAN_POINT('',(-0.288675134594813,-3.53525079574969E-17,-0.972705080756888));
#47306=CARTESIAN_POINT('',(-0.575681140772105,-0.00289101522350376,-0.8));
#47307=CARTESIAN_POINT('Origin',(0.,0.,-0.8));
#47308=CARTESIAN_POINT('Ctrl Pts',(-0.577350269189626,1.38777878078145E-16,
-0.799));
#47309=CARTESIAN_POINT('Ctrl Pts',(-0.576514502127378,-0.00144759101510493,
-0.799502907828364));
#47310=CARTESIAN_POINT('Ctrl Pts',(-0.575681140772105,-0.00289101522350382,
-0.8));
#47311=CARTESIAN_POINT('',(-0.290344263012334,-0.497108984776496,-0.8));
#47312=CARTESIAN_POINT('Ctrl Pts',(-0.290344263012334,-0.497108984776496,
-0.8));
#47313=CARTESIAN_POINT('Ctrl Pts',(-0.289510901657063,-0.498552408984891,
-0.799502907828365));
#47314=CARTESIAN_POINT('Ctrl Pts',(-0.288675134594813,-0.5,-0.799));
#47315=CARTESIAN_POINT('',(-0.285336877759771,-0.5,-0.8));
#47316=CARTESIAN_POINT('Origin',(0.,0.,-0.8));
#47317=CARTESIAN_POINT('Ctrl Pts',(-0.288675134594813,-0.5,-0.799));
#47318=CARTESIAN_POINT('Ctrl Pts',(-0.287003600470267,-0.5,-0.799502907828379));
#47319=CARTESIAN_POINT('Ctrl Pts',(-0.28533687775977,-0.5,-0.8));
#47320=CARTESIAN_POINT('',(0.285336877759771,-0.5,-0.8));
#47321=CARTESIAN_POINT('Ctrl Pts',(0.28533687775977,-0.5,-0.8));
#47322=CARTESIAN_POINT('Ctrl Pts',(0.287003600470239,-0.5,-0.799502907828387));
#47323=CARTESIAN_POINT('Ctrl Pts',(0.288675134594813,-0.5,-0.799));
#47324=CARTESIAN_POINT('',(0.290344263012334,-0.497108984776496,-0.8));
#47325=CARTESIAN_POINT('Origin',(0.,0.,-0.8));
#47326=CARTESIAN_POINT('Ctrl Pts',(0.288675134594813,-0.5,-0.799));
#47327=CARTESIAN_POINT('Ctrl Pts',(0.289510901657071,-0.498552408984877,
-0.79950290782837));
#47328=CARTESIAN_POINT('Ctrl Pts',(0.290344263012334,-0.497108984776496,
-0.8));
#47329=CARTESIAN_POINT('',(0.575681140772105,-0.00289101522350382,-0.8));
#47330=CARTESIAN_POINT('Ctrl Pts',(0.575681140772105,-0.00289101522350412,
-0.8));
#47331=CARTESIAN_POINT('Ctrl Pts',(0.576514502127361,-0.00144759101513511,
-0.799502907828374));
#47332=CARTESIAN_POINT('Ctrl Pts',(0.577350269189626,-3.05311331771918E-16,
-0.799));
#47333=CARTESIAN_POINT('',(0.575681140772105,0.00289101522350384,-0.8));
#47334=CARTESIAN_POINT('Origin',(0.,0.,-0.8));
#47335=CARTESIAN_POINT('Ctrl Pts',(0.577350269189626,4.44089209850062E-16,
-0.799));
#47336=CARTESIAN_POINT('Ctrl Pts',(0.57651450212736,0.00144759101513667,
-0.799502907828375));
#47337=CARTESIAN_POINT('Ctrl Pts',(0.575681140772105,0.00289101522350415,
-0.8));
#47338=CARTESIAN_POINT('',(0.290344263012334,0.497108984776496,-0.8));
#47339=CARTESIAN_POINT('Ctrl Pts',(0.290344263012334,0.497108984776496,
-0.8));
#47340=CARTESIAN_POINT('Ctrl Pts',(0.28951090165707,0.498552408984879,-0.799502907828369));
#47341=CARTESIAN_POINT('Ctrl Pts',(0.288675134594813,0.5,-0.799));
#47342=CARTESIAN_POINT('',(0.28533687775977,0.5,-0.8));
#47343=CARTESIAN_POINT('Origin',(0.,0.,-0.8));
#47344=CARTESIAN_POINT('Ctrl Pts',(0.288675134594813,0.5,-0.799));
#47345=CARTESIAN_POINT('Ctrl Pts',(0.287003600470183,0.5,-0.799502907828404));
#47346=CARTESIAN_POINT('Ctrl Pts',(0.28533687775977,0.5,-0.8));
#47347=CARTESIAN_POINT('',(-0.28533687775977,0.5,-0.8));
#47348=CARTESIAN_POINT('Ctrl Pts',(-0.28533687775977,0.5,-0.8));
#47349=CARTESIAN_POINT('Ctrl Pts',(-0.287003600470227,0.5,-0.799502907828391));
#47350=CARTESIAN_POINT('Ctrl Pts',(-0.288675134594813,0.5,-0.799));
#47351=CARTESIAN_POINT('',(-0.290344263012334,0.497108984776496,-0.8));
#47352=CARTESIAN_POINT('Origin',(0.,0.,-0.8));
#47353=CARTESIAN_POINT('Ctrl Pts',(-0.288675134594813,0.5,-0.799));
#47354=CARTESIAN_POINT('Ctrl Pts',(-0.289510901657074,0.498552408984871,
-0.799502907828372));
#47355=CARTESIAN_POINT('Ctrl Pts',(-0.290344263012334,0.497108984776496,
-0.8));
#47356=CARTESIAN_POINT('',(-0.575681140772105,0.00289101522350423,-0.8));
#47357=CARTESIAN_POINT('Ctrl Pts',(-0.575681140772105,0.00289101522350412,
-0.8));
#47358=CARTESIAN_POINT('Ctrl Pts',(-0.576514502127331,0.00144759101518657,
-0.799502907828392));
#47359=CARTESIAN_POINT('Ctrl Pts',(-0.577350269189626,6.10622663543836E-16,
-0.799));
#47360=CARTESIAN_POINT('Origin',(0.,0.,-0.8));
#47361=CARTESIAN_POINT('Origin',(-0.577350269189626,1.11022302462516E-16,
0.));
#47362=CARTESIAN_POINT('',(-0.288675134594813,0.5,0.));
#47363=CARTESIAN_POINT('',(-0.288675134594813,0.5,0.));
#47364=CARTESIAN_POINT('',(-0.577350269189626,7.07050159149938E-17,0.));
#47365=CARTESIAN_POINT('',(-0.505181485540923,0.125,0.));
#47366=CARTESIAN_POINT('',(-0.577350269189626,7.07050159149938E-17,0.));
#47367=CARTESIAN_POINT('Origin',(-0.577350269189626,1.11022302462516E-16,
0.));
#47368=CARTESIAN_POINT('',(-0.577350269189626,1.11022302462516E-16,-0.8));
#47369=CARTESIAN_POINT('',(-0.577350269189626,7.07050159149938E-17,0.));
#47370=CARTESIAN_POINT('',(-0.288675134594813,0.5,-0.8));
#47371=CARTESIAN_POINT('Origin',(-0.288675134594813,0.5,0.));
#47372=CARTESIAN_POINT('',(0.288675134594813,0.5,0.));
#47373=CARTESIAN_POINT('',(0.288675134594813,0.5,0.));
#47374=CARTESIAN_POINT('',(-0.144337567297406,0.5,0.));
#47375=CARTESIAN_POINT('Origin',(-0.288675134594813,0.5,0.));
#47376=CARTESIAN_POINT('',(0.288675134594813,0.5,-0.8));
#47377=CARTESIAN_POINT('',(0.288675134594813,0.5,-0.8));
#47378=CARTESIAN_POINT('',(0.288675134594813,0.5,0.));
#47379=CARTESIAN_POINT('Origin',(-0.288675134594813,0.5,0.));
#47380=CARTESIAN_POINT('',(-0.288675134594813,0.5,-0.8));
#47381=CARTESIAN_POINT('',(-0.288675134594813,0.5,0.));
#47382=CARTESIAN_POINT('',(0.288675134594813,0.5,-0.8));
#47383=CARTESIAN_POINT('Origin',(-0.288675134594813,-0.5,0.));
#47384=CARTESIAN_POINT('',(-0.288675134594813,-0.5,0.));
#47385=CARTESIAN_POINT('',(-0.360843918243516,-0.375,0.));
#47386=CARTESIAN_POINT('',(-0.288675134594813,-0.5,0.));
#47387=CARTESIAN_POINT('Origin',(-0.288675134594813,-0.5,0.));
#47388=CARTESIAN_POINT('',(-0.288675134594813,-0.5,-0.8));
#47389=CARTESIAN_POINT('',(-0.288675134594813,-0.5,0.));
#47390=CARTESIAN_POINT('',(-0.577350269189626,7.07050159149938E-17,-0.8));
#47391=CARTESIAN_POINT('Origin',(0.288675134594813,0.5,0.));
#47392=CARTESIAN_POINT('',(0.577350269189626,0.,0.));
#47393=CARTESIAN_POINT('',(0.577350269189626,0.,0.));
#47394=CARTESIAN_POINT('',(0.360843918243516,0.375,0.));
#47395=CARTESIAN_POINT('Origin',(0.288675134594813,0.5,0.));
#47396=CARTESIAN_POINT('',(0.577350269189626,0.,-0.8));
#47397=CARTESIAN_POINT('',(0.577350269189626,0.,-0.8));
#47398=CARTESIAN_POINT('',(0.577350269189626,0.,0.));
#47399=CARTESIAN_POINT('Origin',(0.288675134594813,0.5,0.));
#47400=CARTESIAN_POINT('',(0.577350269189626,0.,-0.8));
#47401=CARTESIAN_POINT('Origin',(0.,0.,-0.8));
#47402=CARTESIAN_POINT('',(-0.288675134594813,0.5,-0.8));
#47403=CARTESIAN_POINT('Origin',(0.,0.,-0.8));
#47404=CARTESIAN_POINT('Origin',(0.,0.,-0.8));
#47405=CARTESIAN_POINT('',(0.288675134594813,-0.5,-0.8));
#47406=CARTESIAN_POINT('Origin',(0.,0.,-0.8));
#47407=CARTESIAN_POINT('',(0.288675134594813,-0.5,-0.8));
#47408=CARTESIAN_POINT('',(-0.288675134594813,-0.5,-0.8));
#47409=CARTESIAN_POINT('',(0.288675134594813,-0.5,-0.8));
#47410=CARTESIAN_POINT('Origin',(0.,0.,-0.8));
#47411=CARTESIAN_POINT('',(-0.288675134594813,-0.5,-0.8));
#47412=CARTESIAN_POINT('Origin',(0.,0.,-0.8));
#47413=CARTESIAN_POINT('',(-0.577350269189626,7.07050159149938E-17,-0.8));
#47414=CARTESIAN_POINT('Origin',(0.577350269189626,0.,0.));
#47415=CARTESIAN_POINT('',(0.288675134594813,-0.5,0.));
#47416=CARTESIAN_POINT('',(0.288675134594813,-0.5,0.));
#47417=CARTESIAN_POINT('',(0.505181485540923,-0.125,0.));
#47418=CARTESIAN_POINT('Origin',(0.577350269189626,0.,0.));
#47419=CARTESIAN_POINT('',(0.288675134594813,-0.5,0.));
#47420=CARTESIAN_POINT('Origin',(0.577350269189626,0.,0.));
#47421=CARTESIAN_POINT('Origin',(0.288675134594813,-0.5,0.));
#47422=CARTESIAN_POINT('Origin',(0.288675134594813,-0.5,0.));
#47423=CARTESIAN_POINT('',(0.144337567297406,-0.5,0.));
#47424=CARTESIAN_POINT('Origin',(-0.577350269189626,1.11022302462516E-16,
0.));
#47425=CARTESIAN_POINT('Origin',(-0.288675134594813,-0.5,0.));
#47426=CARTESIAN_POINT('Origin',(0.288675134594813,-0.5,0.));
#47427=CARTESIAN_POINT('Origin',(0.75,0.,-2.));
#47428=CARTESIAN_POINT('',(-0.75,-9.18485099360515E-17,-2.));
#47429=CARTESIAN_POINT('Origin',(0.,0.,-2.));
#47430=CARTESIAN_POINT('Origin',(0.,0.,-1.875));
#47431=CARTESIAN_POINT('',(-0.875,-1.07156594925393E-16,-1.875));
#47432=CARTESIAN_POINT('Origin',(0.,0.,-0.915));
#47433=CARTESIAN_POINT('Origin',(0.,0.,-0.0695250000000001));
#47434=CARTESIAN_POINT('Origin',(0.,0.,-0.04));
#47435=CARTESIAN_POINT('',(-0.92,-1.12667505521556E-16,-6.93889390390723E-18));
#47436=CARTESIAN_POINT('Origin',(0.,0.,0.));
#47437=CARTESIAN_POINT('',(-0.96,-1.17566092718146E-16,-0.04));
#47438=CARTESIAN_POINT('Origin',(0.,0.,0.));
#47439=CARTESIAN_POINT('',(0.,0.,0.));
#47440=CARTESIAN_POINT('Origin',(-4.505,3.4,68.85));
#47441=CARTESIAN_POINT('',(-4.505,3.4,68.85));
#47442=CARTESIAN_POINT('',(-4.505,-3.4,68.85));
#47443=CARTESIAN_POINT('',(-4.505,-0.3,68.85));
#47444=CARTESIAN_POINT('',(-4.655,3.4,68.85));
#47445=CARTESIAN_POINT('',(-4.505,3.4,68.85));
#47446=CARTESIAN_POINT('',(-4.655,-3.4,68.85));
#47447=CARTESIAN_POINT('',(-4.655,-3.4,68.85));
#47448=CARTESIAN_POINT('',(-4.505,-3.4,68.85));
#47449=CARTESIAN_POINT('Origin',(-4.505,3.4,69.15));
#47450=CARTESIAN_POINT('',(-4.505,3.4,69.15));
#47451=CARTESIAN_POINT('',(-4.505,3.4,67.325));
#47452=CARTESIAN_POINT('',(-4.655,3.4,69.15));
#47453=CARTESIAN_POINT('',(-4.505,3.4,69.15));
#47454=CARTESIAN_POINT('',(-4.655,3.4,68.85));
#47455=CARTESIAN_POINT('Origin',(-4.505,-3.4,69.15));
#47456=CARTESIAN_POINT('',(-4.505,-3.4,69.15));
#47457=CARTESIAN_POINT('',(-4.505,-3.7,69.15));
#47458=CARTESIAN_POINT('',(-4.655,-3.4,69.15));
#47459=CARTESIAN_POINT('',(-4.505,-3.4,69.15));
#47460=CARTESIAN_POINT('',(-4.655,3.4,69.15));
#47461=CARTESIAN_POINT('Origin',(-4.505,-3.4,68.85));
#47462=CARTESIAN_POINT('',(-4.505,-3.4,67.175));
#47463=CARTESIAN_POINT('',(-4.655,-3.4,69.15));
#47464=CARTESIAN_POINT('Origin',(-4.655,0.,69.));
#47465=CARTESIAN_POINT('Origin',(-4.505,3.4,72.85));
#47466=CARTESIAN_POINT('',(-4.505,3.4,72.85));
#47467=CARTESIAN_POINT('',(-4.505,-3.4,72.85));
#47468=CARTESIAN_POINT('',(-4.505,-0.3,72.85));
#47469=CARTESIAN_POINT('',(-4.655,3.4,72.85));
#47470=CARTESIAN_POINT('',(-4.505,3.4,72.85));
#47471=CARTESIAN_POINT('',(-4.655,-3.4,72.85));
#47472=CARTESIAN_POINT('',(-4.655,-3.4,72.85));
#47473=CARTESIAN_POINT('',(-4.505,-3.4,72.85));
#47474=CARTESIAN_POINT('Origin',(-4.505,3.4,73.15));
#47475=CARTESIAN_POINT('',(-4.505,3.4,73.15));
#47476=CARTESIAN_POINT('',(-4.505,3.4,69.325));
#47477=CARTESIAN_POINT('',(-4.655,3.4,73.15));
#47478=CARTESIAN_POINT('',(-4.505,3.4,73.15));
#47479=CARTESIAN_POINT('',(-4.655,3.4,72.85));
#47480=CARTESIAN_POINT('Origin',(-4.505,-3.4,73.15));
#47481=CARTESIAN_POINT('',(-4.505,-3.4,73.15));
#47482=CARTESIAN_POINT('',(-4.505,-3.7,73.15));
#47483=CARTESIAN_POINT('',(-4.655,-3.4,73.15));
#47484=CARTESIAN_POINT('',(-4.505,-3.4,73.15));
#47485=CARTESIAN_POINT('',(-4.655,3.4,73.15));
#47486=CARTESIAN_POINT('Origin',(-4.505,-3.4,72.85));
#47487=CARTESIAN_POINT('',(-4.505,-3.4,69.175));
#47488=CARTESIAN_POINT('',(-4.655,-3.4,73.15));
#47489=CARTESIAN_POINT('Origin',(-4.655,0.,73.));
#47490=CARTESIAN_POINT('Origin',(-5.895,-4.,76.4));
#47491=CARTESIAN_POINT('',(-5.995,-3.9,76.4));
#47492=CARTESIAN_POINT('',(-5.895,-3.9,76.5));
#47493=CARTESIAN_POINT('',(-5.995,-3.9,76.4));
#47494=CARTESIAN_POINT('',(-5.895,-4.,76.4));
#47495=CARTESIAN_POINT('',(-5.895,-4.,76.4));
#47496=CARTESIAN_POINT('',(-5.895,-3.9,76.5));
#47497=CARTESIAN_POINT('Origin',(-4.505,-3.9,76.4));
#47498=CARTESIAN_POINT('',(-4.605,-4.,76.4));
#47499=CARTESIAN_POINT('',(-4.605,-3.9,76.5));
#47500=CARTESIAN_POINT('',(-4.605,-4.,76.4));
#47501=CARTESIAN_POINT('',(-4.505,-3.9,76.4));
#47502=CARTESIAN_POINT('',(-4.505,-3.9,76.4));
#47503=CARTESIAN_POINT('',(-4.605,-3.9,76.5));
#47504=CARTESIAN_POINT('Origin',(-5.895,-3.9,65.5));
#47505=CARTESIAN_POINT('',(-5.995,-3.9,65.6));
#47506=CARTESIAN_POINT('',(-5.895,-4.,65.6));
#47507=CARTESIAN_POINT('',(-5.995,-3.9,65.6));
#47508=CARTESIAN_POINT('',(-5.895,-3.9,65.5));
#47509=CARTESIAN_POINT('',(-5.895,-3.9,65.5));
#47510=CARTESIAN_POINT('',(-5.895,-4.,65.6));
#47511=CARTESIAN_POINT('Origin',(-5.995,3.9,76.4));
#47512=CARTESIAN_POINT('',(-5.895,4.,76.4));
#47513=CARTESIAN_POINT('',(-5.895,3.9,76.5));
#47514=CARTESIAN_POINT('',(-5.895,4.,76.4));
#47515=CARTESIAN_POINT('',(-5.995,3.9,76.4));
#47516=CARTESIAN_POINT('',(-5.995,3.9,76.4));
#47517=CARTESIAN_POINT('',(-5.895,3.9,76.5));
#47518=CARTESIAN_POINT('Origin',(-4.605,-3.9,65.5));
#47519=CARTESIAN_POINT('',(-4.605,-4.,65.6));
#47520=CARTESIAN_POINT('',(-4.505,-3.9,65.6));
#47521=CARTESIAN_POINT('',(-4.605,-4.,65.6));
#47522=CARTESIAN_POINT('',(-4.605,-3.9,65.5));
#47523=CARTESIAN_POINT('',(-4.605,-3.9,65.5));
#47524=CARTESIAN_POINT('',(-4.505,-3.9,65.6));
#47525=CARTESIAN_POINT('Origin',(-5.6225,-3.95,65.55));
#47526=CARTESIAN_POINT('',(-5.6225,-4.,65.6));
#47527=CARTESIAN_POINT('',(-5.6225,-3.9,65.5));
#47528=CARTESIAN_POINT('Origin',(-4.605,4.,76.4));
#47529=CARTESIAN_POINT('',(-4.505,3.9,76.4));
#47530=CARTESIAN_POINT('',(-4.605,3.9,76.5));
#47531=CARTESIAN_POINT('',(-4.505,3.9,76.4));
#47532=CARTESIAN_POINT('',(-4.605,4.,76.4));
#47533=CARTESIAN_POINT('',(-4.605,4.,76.4));
#47534=CARTESIAN_POINT('',(-4.605,3.9,76.5));
#47535=CARTESIAN_POINT('Origin',(-5.995,3.9,65.6));
#47536=CARTESIAN_POINT('',(-5.895,3.9,65.5));
#47537=CARTESIAN_POINT('',(-5.895,4.,65.6));
#47538=CARTESIAN_POINT('',(-5.895,3.9,65.5));
#47539=CARTESIAN_POINT('',(-5.995,3.9,65.6));
#47540=CARTESIAN_POINT('',(-5.995,3.9,65.6));
#47541=CARTESIAN_POINT('',(-5.895,4.,65.6));
#47542=CARTESIAN_POINT('Origin',(-5.945,2.,65.55));
#47543=CARTESIAN_POINT('',(-5.995,2.,65.6));
#47544=CARTESIAN_POINT('',(-5.895,2.,65.5));
#47545=CARTESIAN_POINT('Origin',(-5.945,3.95,65.5));
#47546=CARTESIAN_POINT('',(-5.895,4.,65.5));
#47547=CARTESIAN_POINT('',(-5.995,3.9,65.5));
#47548=CARTESIAN_POINT('Origin',(-4.605,3.9,65.5));
#47549=CARTESIAN_POINT('',(-4.505,3.9,65.6));
#47550=CARTESIAN_POINT('',(-4.605,4.,65.6));
#47551=CARTESIAN_POINT('',(-4.505,3.9,65.6));
#47552=CARTESIAN_POINT('',(-4.605,3.9,65.5));
#47553=CARTESIAN_POINT('',(-4.605,3.9,65.5));
#47554=CARTESIAN_POINT('',(-4.605,4.,65.6));
#47555=CARTESIAN_POINT('Origin',(-4.555,-2.,65.55));
#47556=CARTESIAN_POINT('',(-4.505,-2.,65.6));
#47557=CARTESIAN_POINT('',(-4.605,-2.,65.5));
#47558=CARTESIAN_POINT('Origin',(-4.8775,3.95,65.55));
#47559=CARTESIAN_POINT('',(-4.8775,4.,65.6));
#47560=CARTESIAN_POINT('',(-4.8775,3.9,65.5));
#47561=CARTESIAN_POINT('Origin',(-4.555,3.95,65.5));
#47562=CARTESIAN_POINT('',(-4.505,3.9,65.5));
#47563=CARTESIAN_POINT('',(-4.605,4.,65.5));
#47564=CARTESIAN_POINT('Origin',(-4.8775,3.95,76.45));
#47565=CARTESIAN_POINT('',(-4.8775,3.9,76.5));
#47566=CARTESIAN_POINT('',(-4.8775,4.,76.4));
#47567=CARTESIAN_POINT('Origin',(-4.555,-2.,76.45));
#47568=CARTESIAN_POINT('',(-4.605,-2.,76.5));
#47569=CARTESIAN_POINT('',(-4.505,-2.,76.4));
#47570=CARTESIAN_POINT('Origin',(-4.555,-3.95,65.5));
#47571=CARTESIAN_POINT('',(-4.605,-4.,65.5));
#47572=CARTESIAN_POINT('',(-4.505,-3.9,65.5));
#47573=CARTESIAN_POINT('Origin',(-5.945,2.,76.45));
#47574=CARTESIAN_POINT('',(-5.895,2.,76.5));
#47575=CARTESIAN_POINT('',(-5.995,2.,76.4));
#47576=CARTESIAN_POINT('Origin',(-5.945,-3.95,65.5));
#47577=CARTESIAN_POINT('',(-5.995,-3.9,65.5));
#47578=CARTESIAN_POINT('',(-5.895,-4.,65.5));
#47579=CARTESIAN_POINT('Origin',(-5.6225,-3.95,76.45));
#47580=CARTESIAN_POINT('',(-5.6225,-3.9,76.5));
#47581=CARTESIAN_POINT('',(-5.6225,-4.,76.4));
#47582=CARTESIAN_POINT('Origin',(-5.995,-4.,65.5));
#47583=CARTESIAN_POINT('Origin',(-5.25,0.,65.5));
#47584=CARTESIAN_POINT('Origin',(-5.995,4.,65.5));
#47585=CARTESIAN_POINT('Origin',(-4.505,4.,65.5));
#47586=CARTESIAN_POINT('Origin',(-4.505,-4.,65.5));
#47587=CARTESIAN_POINT('Origin',(-5.25,0.,76.5));
#47588=CARTESIAN_POINT('',(0.,0.,0.));
#47589=CARTESIAN_POINT('Origin',(0.,0.,-2.94));
#47590=CARTESIAN_POINT('',(-0.791106180021776,2.03161438686317E-5,-5.74466684917629));
#47591=CARTESIAN_POINT('',(-0.791090782287945,1.29766800149628E-5,-5.7731331508237));
#47592=CARTESIAN_POINT('',(-0.7911,-9.68818082805471E-17,-2.94));
#47593=CARTESIAN_POINT('',(0.342081922270278,0.713331522816647,-5.8089));
#47594=CARTESIAN_POINT('Ctrl Pts',(-0.791106180021776,2.03161438686317E-5,
-5.74466684917629));
#47595=CARTESIAN_POINT('Ctrl Pts',(-0.791135343475079,0.0283677424344691,
-5.74580749484678));
#47596=CARTESIAN_POINT('Ctrl Pts',(-0.789641156878406,0.0567121003347207,
-5.74694814051726));
#47597=CARTESIAN_POINT('Ctrl Pts',(-0.786600263288403,0.0848895237920406,
-5.74808878618774));
#47598=CARTESIAN_POINT('Ctrl Pts',(-0.772508536262909,0.215465799445913,
-5.75337462304639));
#47599=CARTESIAN_POINT('Ctrl Pts',(-0.725201825327082,0.342457217166145,
-5.75866045990504));
#47600=CARTESIAN_POINT('Ctrl Pts',(-0.650430093527711,0.450429424087558,
-5.76394629676369));
#47601=CARTESIAN_POINT('Ctrl Pts',(-0.57565836172834,0.558401631008971,
-5.76923213362234));
#47602=CARTESIAN_POINT('Ctrl Pts',(-0.473421609065425,0.647354627131565,
-5.77451797048098));
#47603=CARTESIAN_POINT('Ctrl Pts',(-0.356146177440628,0.70647482914802,
-5.77980380733963));
#47604=CARTESIAN_POINT('Ctrl Pts',(-0.238870745815832,0.765595031164475,
-5.78508964419828));
#47605=CARTESIAN_POINT('Ctrl Pts',(-0.106556635229153,0.794882439074792,
-5.79037548105694));
#47606=CARTESIAN_POINT('Ctrl Pts',(0.0247138000160614,0.790780700517692,
-5.79566131791558));
#47607=CARTESIAN_POINT('Ctrl Pts',(0.134305248873851,0.787356353897155,
-5.80007421194372));
#47608=CARTESIAN_POINT('Ctrl Pts',(0.243169278281288,0.760660484412965,
-5.80448710597186));
#47609=CARTESIAN_POINT('Ctrl Pts',(0.342095882030774,0.713340734875802,
-5.8089));
#47610=CARTESIAN_POINT('',(-0.342067962509742,0.71332231075751,-5.8089));
#47611=CARTESIAN_POINT('Origin',(0.,0.,-5.8089));
#47612=CARTESIAN_POINT('Ctrl Pts',(-0.342067962509741,0.71332231075751,
-5.8089));
#47613=CARTESIAN_POINT('Ctrl Pts',(-0.460521881974901,0.656518688787926,
-5.80361416314135));
#47614=CARTESIAN_POINT('Ctrl Pts',(-0.564494897987404,0.569670406071105,
-5.79832832628271));
#47615=CARTESIAN_POINT('Ctrl Pts',(-0.641387916838763,0.463218315988371,
-5.79304248942406));
#47616=CARTESIAN_POINT('Ctrl Pts',(-0.718280935690122,0.356766225905636,
-5.78775665256541));
#47617=CARTESIAN_POINT('Ctrl Pts',(-0.768093957380336,0.230710328456987,
-5.78247081570676));
#47618=CARTESIAN_POINT('Ctrl Pts',(-0.784767319259172,0.100431910373907,
-5.77718497884811));
#47619=CARTESIAN_POINT('Ctrl Pts',(-0.789027609334232,0.0671438515176777,
-5.77583436950664));
#47620=CARTESIAN_POINT('Ctrl Pts',(-0.791124284156975,0.0335801136080157,
-5.77448376016517));
#47621=CARTESIAN_POINT('Ctrl Pts',(-0.791090782287945,1.29766800149628E-5,
-5.7731331508237));
#47622=CARTESIAN_POINT('Origin',(0.,0.,-2.94));
#47623=CARTESIAN_POINT('',(-0.791124235703911,-1.85398115769009E-5,-5.5446668491763));
#47624=CARTESIAN_POINT('',(-0.791139506632643,-1.5767809539321E-5,-5.5731331508237));
#47625=CARTESIAN_POINT('',(-0.7911,-9.68818082805471E-17,-2.94));
#47626=CARTESIAN_POINT('Ctrl Pts',(-0.791124235703911,-1.85398115769009E-5,
-5.5446668491763));
#47627=CARTESIAN_POINT('Ctrl Pts',(-0.791015771065361,0.108758589208093,
-5.54904411920968));
#47628=CARTESIAN_POINT('Ctrl Pts',(-0.768397083456412,0.21757942619962,
-5.55342138924305));
#47629=CARTESIAN_POINT('Ctrl Pts',(-0.724790381405401,0.31721456737946,
-5.55779865927643));
#47630=CARTESIAN_POINT('Ctrl Pts',(-0.672132466488617,0.437530448659187,
-5.56308449613507));
#47631=CARTESIAN_POINT('Ctrl Pts',(-0.588869565491455,0.54445163301647,
-5.56837033299372));
#47632=CARTESIAN_POINT('Ctrl Pts',(-0.485121914936739,0.62498232476536,
-5.57365616985236));
#47633=CARTESIAN_POINT('Ctrl Pts',(-0.381374264382023,0.705513016514249,
-5.57894200671101));
#47634=CARTESIAN_POINT('Ctrl Pts',(-0.257141864269753,0.759653215654744,
-5.58422784356967));
#47635=CARTESIAN_POINT('Ctrl Pts',(-0.127524612081043,0.780822420424087,
-5.58951368042832));
#47636=CARTESIAN_POINT('Ctrl Pts',(0.00209264010766494,0.801991625193429,
-5.59479951728696));
#47637=CARTESIAN_POINT('Ctrl Pts',(0.137094744372813,0.79018983559162,-5.60008535414561));
#47638=CARTESIAN_POINT('Ctrl Pts',(0.261072793357542,0.746851507925876,
-5.60537119100425));
#47639=CARTESIAN_POINT('Ctrl Pts',(0.385050842342272,0.703513180260131,
-5.6106570278629));
#47640=CARTESIAN_POINT('Ctrl Pts',(0.498004836046584,0.628638314530449,
-5.61594286472155));
#47641=CARTESIAN_POINT('Ctrl Pts',(0.586205717365502,0.531327616596799,
-5.6212287015802));
#47642=CARTESIAN_POINT('Ctrl Pts',(0.674406598684419,0.434016918663149,
-5.62651453843885));
#47643=CARTESIAN_POINT('Ctrl Pts',(0.737854367617943,0.314270388525531,
-5.63180037529749));
#47644=CARTESIAN_POINT('Ctrl Pts',(0.768837228920146,0.186642690276987,
-5.63708621215614));
#47645=CARTESIAN_POINT('Ctrl Pts',(0.799820090222349,0.0590149920284431,
-5.64237204901479));
#47646=CARTESIAN_POINT('Ctrl Pts',(0.798338043893232,-0.0764938743310262,
-5.64765788587344));
#47647=CARTESIAN_POINT('Ctrl Pts',(0.764571226480889,-0.203413415006452,
-5.65294372273209));
#47648=CARTESIAN_POINT('Ctrl Pts',(0.730804409068546,-0.330332955681878,
-5.65822955959074));
#47649=CARTESIAN_POINT('Ctrl Pts',(0.664752820572977,-0.44866317067326,
-5.66351539644938));
#47650=CARTESIAN_POINT('Ctrl Pts',(0.574444738011475,-0.544021530895698,
-5.66880123330803));
#47651=CARTESIAN_POINT('Ctrl Pts',(0.484136655449973,-0.639379891118138,
-5.67408707016667));
#47652=CARTESIAN_POINT('Ctrl Pts',(0.369572078822538,-0.711766396571634,
-5.67937290702533));
#47653=CARTESIAN_POINT('Ctrl Pts',(0.244675826026431,-0.752382819699385,
-5.68465874388398));
#47654=CARTESIAN_POINT('Ctrl Pts',(0.119779573230324,-0.792999242827135,
-5.68994458074262));
#47655=CARTESIAN_POINT('Ctrl Pts',(-0.0154483557344541,-0.80184558362914,
-5.69523041760127));
#47656=CARTESIAN_POINT('Ctrl Pts',(-0.144571608456504,-0.777846547461446,
-5.70051625445991));
#47657=CARTESIAN_POINT('Ctrl Pts',(-0.273694861178554,-0.753847511293753,
-5.70580209131856));
#47658=CARTESIAN_POINT('Ctrl Pts',(-0.396713437657876,-0.69700309815636,
-5.71108792817721));
#47659=CARTESIAN_POINT('Ctrl Pts',(-0.49867496963204,-0.614222613923978,
-5.71637376503586));
#47660=CARTESIAN_POINT('Ctrl Pts',(-0.600636501606204,-0.531442129691597,
-5.72165960189451));
#47661=CARTESIAN_POINT('Ctrl Pts',(-0.681540989075211,-0.422725574364226,
-5.72694543875316));
#47662=CARTESIAN_POINT('Ctrl Pts',(-0.731554861252135,-0.301286729906785,
-5.7322312756118));
#47663=CARTESIAN_POINT('Ctrl Pts',(-0.770776098641365,-0.206053516811625,
-5.73637646679997));
#47664=CARTESIAN_POINT('Ctrl Pts',(-0.791000197863794,-0.102996338990715,
-5.74052165798813));
#47665=CARTESIAN_POINT('Ctrl Pts',(-0.791106180021776,2.03161438686317E-5,
-5.74466684917629));
#47666=CARTESIAN_POINT('Ctrl Pts',(-0.791090782287945,1.29766800149628E-5,
-5.7731331508237));
#47667=CARTESIAN_POINT('Ctrl Pts',(-0.790993168956811,-0.0977905234557233,
-5.76919792330652));
#47668=CARTESIAN_POINT('Ctrl Pts',(-0.772811500478589,-0.195622879430191,
-5.76526269578935));
#47669=CARTESIAN_POINT('Ctrl Pts',(-0.737372895602027,-0.286749114669279,
-5.76132746827217));
#47670=CARTESIAN_POINT('Ctrl Pts',(-0.68977140799859,-0.409150782911872,
-5.75604163141353));
#47671=CARTESIAN_POINT('Ctrl Pts',(-0.61103473072426,-0.519453180679546,
-5.75075579455488));
#47672=CARTESIAN_POINT('Ctrl Pts',(-0.510731350947639,-0.604236529687556,
-5.74546995769623));
#47673=CARTESIAN_POINT('Ctrl Pts',(-0.410427971171018,-0.689019878695568,
-5.74018412083758));
#47674=CARTESIAN_POINT('Ctrl Pts',(-0.288557888892106,-0.748284178943916,
-5.73489828397893));
#47675=CARTESIAN_POINT('Ctrl Pts',(-0.159934698591644,-0.774832740239663,
-5.72961244712028));
#47676=CARTESIAN_POINT('Ctrl Pts',(-0.0313115082911817,-0.801381301535411,
-5.72432661026163));
#47677=CARTESIAN_POINT('Ctrl Pts',(0.10406479003083,-0.795214123878558,
-5.71904077340299));
#47678=CARTESIAN_POINT('Ctrl Pts',(0.229740230761185,-0.757077413481008,
-5.71375493654434));
#47679=CARTESIAN_POINT('Ctrl Pts',(0.355415671491541,-0.718940703083458,
-5.70846909968569));
#47680=CARTESIAN_POINT('Ctrl Pts',(0.471390254630239,-0.648834459945212,
-5.70318326282704));
#47681=CARTESIAN_POINT('Ctrl Pts',(0.563567566968777,-0.555281520687494,
-5.6978974259684));
#47682=CARTESIAN_POINT('Ctrl Pts',(0.655744879307314,-0.461728581429777,
-5.69261158910975));
#47683=CARTESIAN_POINT('Ctrl Pts',(0.72412492084569,-0.344728946052588,
-5.6873257522511));
#47684=CARTESIAN_POINT('Ctrl Pts',(0.760396511630209,-0.218502514129848,
-5.68203991539245));
#47685=CARTESIAN_POINT('Ctrl Pts',(0.796668102414727,-0.0922760822071087,
-5.6767540785338));
#47686=CARTESIAN_POINT('Ctrl Pts',(0.800831242445389,0.0431771462611828,
-5.67146824167516));
#47687=CARTESIAN_POINT('Ctrl Pts',(0.772379863699283,0.171392977507774,
-5.66618240481651));
#47688=CARTESIAN_POINT('Ctrl Pts',(0.743928484953178,0.299608808754365,
-5.66089656795786));
#47689=CARTESIAN_POINT('Ctrl Pts',(0.682862587430305,0.420587242779256,
-5.65561073109921));
#47690=CARTESIAN_POINT('Ctrl Pts',(0.59660448934969,0.519624119809878,-5.65032489424056));
#47691=CARTESIAN_POINT('Ctrl Pts',(0.510346391269075,0.618660996840501,
-5.64503905738192));
#47692=CARTESIAN_POINT('Ctrl Pts',(0.398896092630719,0.695756316876854,
-5.63975322052327));
#47693=CARTESIAN_POINT('Ctrl Pts',(0.275799868283255,0.741539366466232,
-5.63446738366463));
#47694=CARTESIAN_POINT('Ctrl Pts',(0.152703643935791,0.787322416055611,
-5.62918154680598));
#47695=CARTESIAN_POINT('Ctrl Pts',(0.0179614938792174,0.801793195198013,
-5.62389570994733));
#47696=CARTESIAN_POINT('Ctrl Pts',(-0.112049263241192,0.78319290579391,
-5.61860987308868));
#47697=CARTESIAN_POINT('Ctrl Pts',(-0.242060020361602,0.764592616389807,
-5.61332403623003));
#47698=CARTESIAN_POINT('Ctrl Pts',(-0.36733938454585,0.712921258439198,
-5.60803819937139));
#47699=CARTESIAN_POINT('Ctrl Pts',(-0.472660208346534,0.634459225234524,
-5.60275236251274));
#47700=CARTESIAN_POINT('Ctrl Pts',(-0.577981032147217,0.555997192029851,
-5.59746652565409));
#47701=CARTESIAN_POINT('Ctrl Pts',(-0.663343315564336,0.450744483571114,
-5.59218068879544));
#47702=CARTESIAN_POINT('Ctrl Pts',(-0.718371649464549,0.331494115958518,
-5.58689485193679));
#47703=CARTESIAN_POINT('Ctrl Pts',(-0.766127158140359,0.228004485045039,
-5.58230761823243));
#47704=CARTESIAN_POINT('Ctrl Pts',(-0.791037034503848,0.11397269330664,
-5.57772038452807));
#47705=CARTESIAN_POINT('Ctrl Pts',(-0.791139506632643,-1.5767809539321E-5,
-5.5731331508237));
#47706=CARTESIAN_POINT('Origin',(0.,0.,-2.94));
#47707=CARTESIAN_POINT('',(-0.791036503466522,7.11594896907197E-6,-5.3446668491763));
#47708=CARTESIAN_POINT('',(-0.791033090718594,2.41426438800759E-6,-5.3731331508237));
#47709=CARTESIAN_POINT('',(-0.7911,-9.68818082805471E-17,-2.94));
#47710=CARTESIAN_POINT('Ctrl Pts',(-0.791036503466522,7.11594896907197E-6,
-5.3446668491763));
#47711=CARTESIAN_POINT('Ctrl Pts',(-0.791054774529985,0.0578788267958651,
-5.34699490671392));
#47712=CARTESIAN_POINT('Ctrl Pts',(-0.784789673957966,0.115746641424242,
-5.34932296425154));
#47713=CARTESIAN_POINT('Ctrl Pts',(-0.772199447682732,0.172203924778507,
-5.35165102178916));
#47714=CARTESIAN_POINT('Ctrl Pts',(-0.743613435082568,0.300389755442302,
-5.35693685864781));
#47715=CARTESIAN_POINT('Ctrl Pts',(-0.682420541996382,0.421304106164855,
-5.36222269550646));
#47716=CARTESIAN_POINT('Ctrl Pts',(-0.596058493308848,0.520250373632772,
-5.3675085323651));
#47717=CARTESIAN_POINT('Ctrl Pts',(-0.509696444621315,0.619196641100689,
-5.37279436922375));
#47718=CARTESIAN_POINT('Ctrl Pts',(-0.398165240332434,0.69617482531397,
-5.3780802060824));
#47719=CARTESIAN_POINT('Ctrl Pts',(-0.275021003902314,0.741828569228208,
-5.38336604294105));
#47720=CARTESIAN_POINT('Ctrl Pts',(-0.151876767472194,0.787482313142446,
-5.3886518797997));
#47721=CARTESIAN_POINT('Ctrl Pts',(-0.0171194989008363,0.801811616757642,
-5.39393771665834));
#47722=CARTESIAN_POINT('Ctrl Pts',(0.112871653199976,0.783074816741423,
-5.39922355351699));
#47723=CARTESIAN_POINT('Ctrl Pts',(0.24286280530079,0.764338016725204,-5.40450939037564));
#47724=CARTESIAN_POINT('Ctrl Pts',(0.368087840931059,0.712535113077569,
-5.40979522723429));
#47725=CARTESIAN_POINT('Ctrl Pts',(0.473326212136283,0.633962519093404,
-5.41508106409294));
#47726=CARTESIAN_POINT('Ctrl Pts',(0.578564583341508,0.555389925109238,
-5.42036690095158));
#47727=CARTESIAN_POINT('Ctrl Pts',(0.663816290121689,0.450047640788541,
-5.42565273781023));
#47728=CARTESIAN_POINT('Ctrl Pts',(0.718719365441129,0.33073955380426,-5.43093857466888));
#47729=CARTESIAN_POINT('Ctrl Pts',(0.773622440760568,0.211431466819979,
-5.43622441152752));
#47730=CARTESIAN_POINT('Ctrl Pts',(0.798176884619266,0.078157577172114,
-5.44151024838617));
#47731=CARTESIAN_POINT('Ctrl Pts',(0.789398213216727,-0.052883264658473,
-5.44679608524482));
#47732=CARTESIAN_POINT('Ctrl Pts',(0.780619541814188,-0.18392410648906,
-5.45208192210347));
#47733=CARTESIAN_POINT('Ctrl Pts',(0.738507755150412,-0.312731900502369,
-5.45736775896212));
#47734=CARTESIAN_POINT('Ctrl Pts',(0.66818135421168,-0.423650630347585,
-5.46265359582076));
#47735=CARTESIAN_POINT('Ctrl Pts',(0.597854953272949,-0.5345693601928,-5.46793943267941));
#47736=CARTESIAN_POINT('Ctrl Pts',(0.499313938059263,-0.627599025869922,
-5.47322526953806));
#47737=CARTESIAN_POINT('Ctrl Pts',(0.384535532134293,-0.691432283914052,
-5.47851110639671));
#47738=CARTESIAN_POINT('Ctrl Pts',(0.269757126209322,-0.755265541958182,
-5.48379694325536));
#47739=CARTESIAN_POINT('Ctrl Pts',(0.138741329573066,-0.789902392369319,
-5.489082780114));
#47740=CARTESIAN_POINT('Ctrl Pts',(0.00741253151014375,-0.791132879536305,
-5.49436861697265));
#47741=CARTESIAN_POINT('Ctrl Pts',(-0.123916266552779,-0.792363366703291,
-5.4996544538313));
#47742=CARTESIAN_POINT('Ctrl Pts',(-0.255558066042368,-0.760187490626126,
-5.50494029068995));
#47743=CARTESIAN_POINT('Ctrl Pts',(-0.371512389803684,-0.698516086385605,
-5.5102261275486));
#47744=CARTESIAN_POINT('Ctrl Pts',(-0.487466713564998,-0.636844682145085,
-5.51551196440724));
#47745=CARTESIAN_POINT('Ctrl Pts',(-0.587733561598039,-0.545677749741209,
-5.52079780126589));
#47746=CARTESIAN_POINT('Ctrl Pts',(-0.660125943008546,-0.436096225700483,
-5.52608363812454));
#47747=CARTESIAN_POINT('Ctrl Pts',(-0.732518324419053,-0.326514701659758,
-5.53136947498318));
#47748=CARTESIAN_POINT('Ctrl Pts',(-0.777036239207025,-0.198518585982181,
-5.53665531184184));
#47749=CARTESIAN_POINT('Ctrl Pts',(-0.788268732182809,-0.0676652390423088,
-5.54194114870048));
#47750=CARTESIAN_POINT('Ctrl Pts',(-0.790199452096383,-0.0451732452133963,
-5.54284971552576));
#47751=CARTESIAN_POINT('Ctrl Pts',(-0.791146749136153,-0.0225968340502242,
-5.54375828235103));
#47752=CARTESIAN_POINT('Ctrl Pts',(-0.791124235703911,-1.85398115769009E-5,
-5.5446668491763));
#47753=CARTESIAN_POINT('Ctrl Pts',(-0.791139506632643,-1.5767809539321E-5,
-5.5731331508237));
#47754=CARTESIAN_POINT('Ctrl Pts',(-0.791155112410987,-0.017375401876565,
-5.57243454766942));
#47755=CARTESIAN_POINT('Ctrl Pts',(-0.790595356852504,-0.0347340309708619,
-5.57173594451514));
#47756=CARTESIAN_POINT('Ctrl Pts',(-0.789453310686279,-0.0520542655584215,
-5.57103734136085));
#47757=CARTESIAN_POINT('Ctrl Pts',(-0.780812253624487,-0.183104252696313,
-5.5657515045022));
#47758=CARTESIAN_POINT('Ctrl Pts',(-0.738835755117596,-0.311956200205645,
-5.56046566764355));
#47759=CARTESIAN_POINT('Ctrl Pts',(-0.668625871952495,-0.422948720884337,
-5.5551798307849));
#47760=CARTESIAN_POINT('Ctrl Pts',(-0.598415988787394,-0.533941241563029,
-5.54989399392626));
#47761=CARTESIAN_POINT('Ctrl Pts',(-0.499972720964085,-0.627074335411082,
-5.54460815706761));
#47762=CARTESIAN_POINT('Ctrl Pts',(-0.385261411552517,-0.691028089876542,
-5.53932232020896));
#47763=CARTESIAN_POINT('Ctrl Pts',(-0.270550102140948,-0.754981844342002,
-5.53403648335032));
#47764=CARTESIAN_POINT('Ctrl Pts',(-0.139570751141121,-0.789756259424867,
-5.52875064649167));
#47765=CARTESIAN_POINT('Ctrl Pts',(-0.00824331789442176,-0.791124658030534,
-5.52346480963302));
#47766=CARTESIAN_POINT('Ctrl Pts',(0.123084115352277,-0.7924930566362,-5.51817897277437));
#47767=CARTESIAN_POINT('Ctrl Pts',(0.254759630845846,-0.760455438764667,
-5.51289313591572));
#47768=CARTESIAN_POINT('Ctrl Pts',(0.370778653329351,-0.698905835406252,
-5.50760729905707));
#47769=CARTESIAN_POINT('Ctrl Pts',(0.486797675812856,-0.637356232047837,
-5.50232146219843));
#47770=CARTESIAN_POINT('Ctrl Pts',(0.587160205286296,-0.546294643202539,
-5.49703562533978));
#47771=CARTESIAN_POINT('Ctrl Pts',(0.659667621238271,-0.436789201028132,
-5.49174978848114));
#47772=CARTESIAN_POINT('Ctrl Pts',(0.732175037190245,-0.327283758853726,
-5.48646395162249));
#47773=CARTESIAN_POINT('Ctrl Pts',(0.776827339620753,-0.199334463350209,
-5.48117811476383));
#47774=CARTESIAN_POINT('Ctrl Pts',(0.788197239095969,-0.0684929843301605,
-5.47589227790519));
#47775=CARTESIAN_POINT('Ctrl Pts',(0.799567138571185,0.0623484946898892,
-5.47060644104654));
#47776=CARTESIAN_POINT('Ctrl Pts',(0.777654635091107,0.196082157226472,
-5.46532060418789));
#47777=CARTESIAN_POINT('Ctrl Pts',(0.725123096324371,0.316453269519017,
-5.46003476732925));
#47778=CARTESIAN_POINT('Ctrl Pts',(0.672591557557635,0.436824381811562,
-5.4547489304706));
#47779=CARTESIAN_POINT('Ctrl Pts',(0.589440983504239,0.543832943860071,
-5.44946309361195));
#47780=CARTESIAN_POINT('Ctrl Pts',(0.485777957826538,0.624472539281158,
-5.4441772567533));
#47781=CARTESIAN_POINT('Ctrl Pts',(0.382114932148837,0.705112134702245,
-5.43889141989465));
#47782=CARTESIAN_POINT('Ctrl Pts',(0.257939454846829,0.759382763495911,
-5.43360558303601));
#47783=CARTESIAN_POINT('Ctrl Pts',(0.128344504715389,0.780688071335382,
-5.42831974617736));
#47784=CARTESIAN_POINT('Ctrl Pts',(-0.00125044541605168,0.801993379174853,
-5.42303390931871));
#47785=CARTESIAN_POINT('Ctrl Pts',(-0.136264868376925,0.79033336606013,
-5.41774807246006));
#47786=CARTESIAN_POINT('Ctrl Pts',(-0.26028835958063,0.747125254886002,
-5.41246223560142));
#47787=CARTESIAN_POINT('Ctrl Pts',(-0.384311850784336,0.703917143711875,
-5.40717639874277));
#47788=CARTESIAN_POINT('Ctrl Pts',(-0.497344410230873,0.629160934478343,
-5.40189056188412));
#47789=CARTESIAN_POINT('Ctrl Pts',(-0.58564743139563,0.531942913026377,
-5.39660472502547));
#47790=CARTESIAN_POINT('Ctrl Pts',(-0.673950452560386,0.434724891574412,
-5.39131888816682));
#47791=CARTESIAN_POINT('Ctrl Pts',(-0.737523935443362,0.315045057904013,
-5.38603305130817));
#47792=CARTESIAN_POINT('Ctrl Pts',(-0.76864080502364,0.187449965250839,
-5.38074721444953));
#47793=CARTESIAN_POINT('Ctrl Pts',(-0.783581726783468,0.126184538426627,
-5.37820919324092));
#47794=CARTESIAN_POINT('Ctrl Pts',(-0.79103981326595,0.0630942576475916,
-5.37567117203231));
#47795=CARTESIAN_POINT('Ctrl Pts',(-0.791033090718594,2.41426438800759E-6,
-5.3731331508237));
#47796=CARTESIAN_POINT('Origin',(0.,0.,-2.94));
#47797=CARTESIAN_POINT('',(-0.791162299475494,7.14138476723761E-6,-5.1446668491763));
#47798=CARTESIAN_POINT('',(-0.791152598342819,1.19001633874275E-5,-5.1731331508237));
#47799=CARTESIAN_POINT('',(-0.7911,-9.68818082805471E-17,-2.94));
#47800=CARTESIAN_POINT('Ctrl Pts',(-0.791162299475494,7.14138476723761E-6,
-5.1446668491763));
#47801=CARTESIAN_POINT('Ctrl Pts',(-0.791165583502069,0.00693560089265366,
-5.14494569421816));
#47802=CARTESIAN_POINT('Ctrl Pts',(-0.791076463159219,0.0138639757192367,
-5.14522453926003));
#47803=CARTESIAN_POINT('Ctrl Pts',(-0.79089440411256,0.0207899075053255,
-5.1455033843019));
#47804=CARTESIAN_POINT('Ctrl Pts',(-0.787443260018906,0.152079118424528,
-5.15078922116055));
#47805=CARTESIAN_POINT('Ctrl Pts',(-0.750595822533239,0.282490455069959,
-5.15607505801919));
#47806=CARTESIAN_POINT('Ctrl Pts',(-0.684830734336137,0.396172997589774,
-5.16136089487784));
#47807=CARTESIAN_POINT('Ctrl Pts',(-0.619065646139034,0.509855540109591,
-5.16664673173649));
#47808=CARTESIAN_POINT('Ctrl Pts',(-0.524382907230495,0.606809288503791,
-5.17193256859513));
#47809=CARTESIAN_POINT('Ctrl Pts',(-0.412290784793401,0.675249944453965,
-5.17721840545378));
#47810=CARTESIAN_POINT('Ctrl Pts',(-0.300198662356306,0.743690600404138,
-5.18250424231243));
#47811=CARTESIAN_POINT('Ctrl Pts',(-0.170697156390656,0.783618163910285,
-5.18779007917108));
#47812=CARTESIAN_POINT('Ctrl Pts',(-0.0395266008624761,0.790179616628333,
-5.19307591602973));
#47813=CARTESIAN_POINT('Ctrl Pts',(0.0916439546657044,0.79674106934638,
-5.19836175288837));
#47814=CARTESIAN_POINT('Ctrl Pts',(0.224483559756416,0.769936411276328,
-5.20364758974702));
#47815=CARTESIAN_POINT('Ctrl Pts',(0.342846149292877,0.71302362978073,-5.20893342660567));
#47816=CARTESIAN_POINT('Ctrl Pts',(0.461208738829339,0.656110848285131,
-5.21421926346432));
#47817=CARTESIAN_POINT('Ctrl Pts',(0.56509431281155,0.569089943363986,-5.21950510032297));
#47818=CARTESIAN_POINT('Ctrl Pts',(0.641876040249872,0.462537920244151,
-5.22479093718161));
#47819=CARTESIAN_POINT('Ctrl Pts',(0.718657767688194,0.355985897124317,
-5.23007677404026));
#47820=CARTESIAN_POINT('Ctrl Pts',(0.768335648582626,0.229902755805793,
-5.23536261089891));
#47821=CARTESIAN_POINT('Ctrl Pts',(0.784871556734003,0.0996133431854589,
-5.24064844775755));
#47822=CARTESIAN_POINT('Ctrl Pts',(0.801407464885379,-0.0306760694348751,
-5.2459342846162));
#47823=CARTESIAN_POINT('Ctrl Pts',(0.784801400293699,-0.165171753357019,
-5.25122012147486));
#47824=CARTESIAN_POINT('Ctrl Pts',(0.737071756494895,-0.28752635442368,
-5.2565059583335));
#47825=CARTESIAN_POINT('Ctrl Pts',(0.68934211269609,-0.409880955490341,
-5.26179179519215));
#47826=CARTESIAN_POINT('Ctrl Pts',(0.610488889690159,-0.520094473701518,
-5.26707763205079));
#47827=CARTESIAN_POINT('Ctrl Pts',(0.510096347174747,-0.60477094449851,
-5.27236346890944));
#47828=CARTESIAN_POINT('Ctrl Pts',(0.409703804659335,-0.689447415295502,
-5.27764930576809));
#47829=CARTESIAN_POINT('Ctrl Pts',(0.287771942634442,-0.748586838678309,
-5.28293514262674));
#47830=CARTESIAN_POINT('Ctrl Pts',(0.159121038401552,-0.775001079901604,
-5.28822097948539));
#47831=CARTESIAN_POINT('Ctrl Pts',(0.0304701341686633,-0.8014153211249,
-5.29350681634404));
#47832=CARTESIAN_POINT('Ctrl Pts',(-0.104899812272221,-0.795104380188685,
-5.29879265320268));
#47833=CARTESIAN_POINT('Ctrl Pts',(-0.230535184030287,-0.756835323987168,
-5.30407849006133));
#47834=CARTESIAN_POINT('Ctrl Pts',(-0.356170555788353,-0.71856626778565,
-5.30936432691998));
#47835=CARTESIAN_POINT('Ctrl Pts',(-0.4720713528636,-0.64833909631883,-5.31465016377863));
#47836=CARTESIAN_POINT('Ctrl Pts',(-0.564150347163279,-0.554689610959313,
-5.31993600063728));
#47837=CARTESIAN_POINT('Ctrl Pts',(-0.656229341462958,-0.461040125599795,
-5.32522183749592));
#47838=CARTESIAN_POINT('Ctrl Pts',(-0.72448653298707,-0.343968326347581,
-5.33050767435457));
#47839=CARTESIAN_POINT('Ctrl Pts',(-0.760625562692054,-0.217703771418954,
-5.33579351121322));
#47840=CARTESIAN_POINT('Ctrl Pts',(-0.780847767349863,-0.14705030640792,
-5.33875129053424));
#47841=CARTESIAN_POINT('Ctrl Pts',(-0.791013290219938,-0.0735184506872712,
-5.34170906985527));
#47842=CARTESIAN_POINT('Ctrl Pts',(-0.791036503466522,7.11594896907197E-6,
-5.3446668491763));
#47843=CARTESIAN_POINT('Ctrl Pts',(-0.791033090718594,2.41426438800759E-6,
-5.3731331508237));
#47844=CARTESIAN_POINT('Ctrl Pts',(-0.791025812481214,-0.0683046408737211,
-5.37038533517366));
#47845=CARTESIAN_POINT('Ctrl Pts',(-0.782268628123843,-0.13661352762463,
-5.36763751952363));
#47846=CARTESIAN_POINT('Ctrl Pts',(-0.764784413766543,-0.202610407135802,
-5.36488970387359));
#47847=CARTESIAN_POINT('Ctrl Pts',(-0.73115089665159,-0.329565335233317,
-5.35960386701494));
#47848=CARTESIAN_POINT('Ctrl Pts',(-0.665223606144103,-0.447964839792398,
-5.35431803015629));
#47849=CARTESIAN_POINT('Ctrl Pts',(-0.57501571214768,-0.543417985903174,
-5.34903219329764));
#47850=CARTESIAN_POINT('Ctrl Pts',(-0.484807818151257,-0.638871132013949,
-5.34374635643899));
#47851=CARTESIAN_POINT('Ctrl Pts',(-0.370319320665898,-0.71137791967642,
-5.33846051958035));
#47852=CARTESIAN_POINT('Ctrl Pts',(-0.245465789029923,-0.752125470274645,
-5.3331746827217));
#47853=CARTESIAN_POINT('Ctrl Pts',(-0.120612257393947,-0.792873020872871,
-5.32788884586305));
#47854=CARTESIAN_POINT('Ctrl Pts',(0.0146063083926455,-0.801861334406852,
-5.3226030090044));
#47855=CARTESIAN_POINT('Ctrl Pts',(0.143754691086471,-0.777997921212178,
-5.31731717214575));
#47856=CARTESIAN_POINT('Ctrl Pts',(0.272903073780296,-0.754134508017505,
-5.3120313352871));
#47857=CARTESIAN_POINT('Ctrl Pts',(0.395981273381354,-0.697419368094177,
-5.30674549842846));
#47858=CARTESIAN_POINT('Ctrl Pts',(0.498029680337536,-0.614745975279851,
-5.30145966156981));
#47859=CARTESIAN_POINT('Ctrl Pts',(0.600078087293719,-0.532072582465523,
-5.29617382471116));
#47860=CARTESIAN_POINT('Ctrl Pts',(0.681096701605026,-0.423440936760197,
-5.29088798785252));
#47861=CARTESIAN_POINT('Ctrl Pts',(0.731238069859886,-0.302054733132022,
-5.28560215099387));
#47862=CARTESIAN_POINT('Ctrl Pts',(0.781379438114745,-0.180668529503849,
-5.28031631413522));
#47863=CARTESIAN_POINT('Ctrl Pts',(0.800643560313157,-0.0465277679528264,
-5.27503047727657));
#47864=CARTESIAN_POINT('Ctrl Pts',(0.786688967800344,0.0840633366046011,
-5.26974464041792));
#47865=CARTESIAN_POINT('Ctrl Pts',(0.772734375287532,0.21465444116203,-5.26445880355928));
#47866=CARTESIAN_POINT('Ctrl Pts',(0.725561068063496,0.341695888725864,
-5.25917296670063));
#47867=CARTESIAN_POINT('Ctrl Pts',(0.650902752500616,0.449746354523297,
-5.25388712984198));
#47868=CARTESIAN_POINT('Ctrl Pts',(0.576244436937734,0.55779682032073,-5.24860129298333));
#47869=CARTESIAN_POINT('Ctrl Pts',(0.474101113036009,0.64685630435176,-5.24331545612469));
#47870=CARTESIAN_POINT('Ctrl Pts',(0.356887849011243,0.706100021135814,
-5.23802961926604));
#47871=CARTESIAN_POINT('Ctrl Pts',(0.239674584986477,0.765343737919869,
-5.23274378240739));
#47872=CARTESIAN_POINT('Ctrl Pts',(0.107391380838672,0.794771687456947,
-5.22745794554874));
#47873=CARTESIAN_POINT('Ctrl Pts',(-0.0238833263834611,0.790807032935806,
-5.22217210869009));
#47874=CARTESIAN_POINT('Ctrl Pts',(-0.155158033605592,0.786842378414665,
-5.21688627183145));
#47875=CARTESIAN_POINT('Ctrl Pts',(-0.285424243902055,0.749485119835303,
-5.2116004349728));
#47876=CARTESIAN_POINT('Ctrl Pts',(-0.398848676885365,0.683275866372188,
-5.20631459811415));
#47877=CARTESIAN_POINT('Ctrl Pts',(-0.512273109868676,0.617066612909072,
-5.2010287612555));
#47878=CARTESIAN_POINT('Ctrl Pts',(-0.608855765538835,0.522005364562204,
-5.19574292439686));
#47879=CARTESIAN_POINT('Ctrl Pts',(-0.676857450252979,0.409646394658744,
-5.19045708753821));
#47880=CARTESIAN_POINT('Ctrl Pts',(-0.744859134967124,0.297287424755283,
-5.18517125067956));
#47881=CARTESIAN_POINT('Ctrl Pts',(-0.78427984872525,0.167630733295234,
-5.17988541382091));
#47882=CARTESIAN_POINT('Ctrl Pts',(-0.790328178523278,0.0364355163535207,
-5.17459957696226));
#47883=CARTESIAN_POINT('Ctrl Pts',(-0.790887498907648,0.0243032151038108,
-5.17411076824941));
#47884=CARTESIAN_POINT('Ctrl Pts',(-0.791161430049627,0.0121577569090612,
-5.17362195953655));
#47885=CARTESIAN_POINT('Ctrl Pts',(-0.791152598342819,1.19001633874275E-5,
-5.1731331508237));
#47886=CARTESIAN_POINT('Origin',(0.,0.,-2.94));
#47887=CARTESIAN_POINT('',(-0.791060709844548,-1.70870917380883E-5,-4.9446668491763));
#47888=CARTESIAN_POINT('',(-0.791074454148617,-1.92722236624013E-5,-4.9731331508237));
#47889=CARTESIAN_POINT('',(-0.7911,-9.68818082805471E-17,-2.94));
#47890=CARTESIAN_POINT('Ctrl Pts',(-0.791060709844548,-1.70870917380883E-5,
-4.9446668491763));
#47891=CARTESIAN_POINT('Ctrl Pts',(-0.790991723705553,0.087364085980534,
-4.94818231858106));
#47892=CARTESIAN_POINT('Ctrl Pts',(-0.776551363288388,0.174767498638758,
-4.95169778798581));
#47893=CARTESIAN_POINT('Ctrl Pts',(-0.748137656794717,0.25736399358953,
-4.95521325739057));
#47894=CARTESIAN_POINT('Ctrl Pts',(-0.705414993109545,0.381555544457479,
-4.96049909424922));
#47895=CARTESIAN_POINT('Ctrl Pts',(-0.631101481703098,0.494879647795438,
-4.96578493110787));
#47896=CARTESIAN_POINT('Ctrl Pts',(-0.534229600452781,0.583562261211863,
-4.97107076796652));
#47897=CARTESIAN_POINT('Ctrl Pts',(-0.437357719202465,0.672244874628287,
-4.97635660482517));
#47898=CARTESIAN_POINT('Ctrl Pts',(-0.317927468108279,0.736285998123177,
-4.98164244168382));
#47899=CARTESIAN_POINT('Ctrl Pts',(-0.190455064752799,0.767901717031971,
-4.98692827854246));
#47900=CARTESIAN_POINT('Ctrl Pts',(-0.0629826613973188,0.799517435940764,
-4.99221411540111));
#47901=CARTESIAN_POINT('Ctrl Pts',(0.0725318942194566,0.798707750263462,
-4.99749995225976));
#47902=CARTESIAN_POINT('Ctrl Pts',(0.199617408602439,0.765571073704779,
-5.0027857891184));
#47903=CARTESIAN_POINT('Ctrl Pts',(0.326702922985424,0.732434397146095,
-5.00807162597705));
#47904=CARTESIAN_POINT('Ctrl Pts',(0.445359396134616,0.666970729706029,
-5.0133574628357));
#47905=CARTESIAN_POINT('Ctrl Pts',(0.541164659746473,0.5771368899595,-5.01864329969435));
#47906=CARTESIAN_POINT('Ctrl Pts',(0.636969923358331,0.487303050212971,
-5.023929136553));
#47907=CARTESIAN_POINT('Ctrl Pts',(0.709923977432854,0.373099038159977,
-5.02921497341164));
#47908=CARTESIAN_POINT('Ctrl Pts',(0.751159580104816,0.248405845195715,
-5.03450081027029));
#47909=CARTESIAN_POINT('Ctrl Pts',(0.792395182776778,0.123712652231453,
-5.03978664712894));
#47910=CARTESIAN_POINT('Ctrl Pts',(0.801912334046179,-0.0114697216440781,
-5.04507248398759));
#47911=CARTESIAN_POINT('Ctrl Pts',(0.778554266366044,-0.140710458153868,
-5.05035832084624));
#47912=CARTESIAN_POINT('Ctrl Pts',(0.755196198685909,-0.269951194663658,
-5.05564415770488));
#47913=CARTESIAN_POINT('Ctrl Pts',(0.698962912056239,-0.393250293807705,
-5.06092999456353));
#47914=CARTESIAN_POINT('Ctrl Pts',(0.616689313183004,-0.495621296673696,
-5.06621583142218));
#47915=CARTESIAN_POINT('Ctrl Pts',(0.534415714309769,-0.597992299539687,
-5.07150166828082));
#47916=CARTESIAN_POINT('Ctrl Pts',(0.42610180319297,-0.679435206127621,
-5.07678750513948));
#47917=CARTESIAN_POINT('Ctrl Pts',(0.304912655570005,-0.730050992180607,
-5.08207334199812));
#47918=CARTESIAN_POINT('Ctrl Pts',(0.183723507947039,-0.780666778233593,
-5.08735917885677));
#47919=CARTESIAN_POINT('Ctrl Pts',(0.0496591238179061,-0.800455443751631,
-5.09264501571542));
#47920=CARTESIAN_POINT('Ctrl Pts',(-0.0809855652379758,-0.787011764164759,
-5.09793085257406));
#47921=CARTESIAN_POINT('Ctrl Pts',(-0.211630254293858,-0.773568084577886,
-5.10321668943271));
#47922=CARTESIAN_POINT('Ctrl Pts',(-0.33885524827649,-0.726892059886103,
-5.10850252629136));
#47923=CARTESIAN_POINT('Ctrl Pts',(-0.447196913159535,-0.652656953974463,
-5.11378836315001));
#47924=CARTESIAN_POINT('Ctrl Pts',(-0.555538578042581,-0.578421848062822,
-5.11907420000866));
#47925=CARTESIAN_POINT('Ctrl Pts',(-0.644996913826041,-0.476627660931325,
-5.12436003686731));
#47926=CARTESIAN_POINT('Ctrl Pts',(-0.704698656366949,-0.359647024769088,
-5.12964587372595));
#47927=CARTESIAN_POINT('Ctrl Pts',(-0.761250938312779,-0.248837496656634,
-5.13465286554273));
#47928=CARTESIAN_POINT('Ctrl Pts',(-0.791103330902562,-0.124401525976414,
-5.13965985735951));
#47929=CARTESIAN_POINT('Ctrl Pts',(-0.791162299475494,7.14138476723761E-6,
-5.1446668491763));
#47930=CARTESIAN_POINT('Ctrl Pts',(-0.791152598342819,1.19001633874275E-5,
-5.1731331508237));
#47931=CARTESIAN_POINT('Ctrl Pts',(-0.791065926511851,-0.119184045267977,
-5.16833612267791));
#47932=CARTESIAN_POINT('Ctrl Pts',(-0.763746661094271,-0.238418374721096,
-5.16353909453211));
#47933=CARTESIAN_POINT('Ctrl Pts',(-0.711677133692105,-0.345632512937747,
-5.15874206638632));
#47934=CARTESIAN_POINT('Ctrl Pts',(-0.654301813224974,-0.463771582863925,
-5.15345622952767));
#47935=CARTESIAN_POINT('Ctrl Pts',(-0.566875226452784,-0.567315980292908,
-5.14817039266903));
#47936=CARTESIAN_POINT('Ctrl Pts',(-0.460023687432986,-0.643680342732655,
-5.14288455581038));
#47937=CARTESIAN_POINT('Ctrl Pts',(-0.353172148413187,-0.720044705172403,
-5.13759871895173));
#47938=CARTESIAN_POINT('Ctrl Pts',(-0.226895657145782,-0.769229032622914,
-5.13231288209308));
#47939=CARTESIAN_POINT('Ctrl Pts',(-0.0965425613568067,-0.785255188118193,
-5.12702704523443));
#47940=CARTESIAN_POINT('Ctrl Pts',(0.0338105344321687,-0.801281343613472,
-5.12174120837578));
#47941=CARTESIAN_POINT('Ctrl Pts',(0.168240234742713,-0.784149327153519,
-5.11645537151714));
#47942=CARTESIAN_POINT('Ctrl Pts',(0.290407205433014,-0.735941459392293,
-5.11116953465849));
#47943=CARTESIAN_POINT('Ctrl Pts',(0.412574176123315,-0.687733591631067,
-5.10588369779984));
#47944=CARTESIAN_POINT('Ctrl Pts',(0.522478417193373,-0.608449872568568,
-5.10059786094119));
#47945=CARTESIAN_POINT('Ctrl Pts',(0.606761555349955,-0.507726886789714,
-5.09531202408255));
#47946=CARTESIAN_POINT('Ctrl Pts',(0.691044693506536,-0.407003901010859,
-5.0900261872239));
#47947=CARTESIAN_POINT('Ctrl Pts',(0.74970672874964,-0.284841648515652,
-5.08474035036525));
#47948=CARTESIAN_POINT('Ctrl Pts',(0.775617550746048,-0.156088409545911,
-5.0794545135066));
#47949=CARTESIAN_POINT('Ctrl Pts',(0.801528372742457,-0.0273351705761713,
-5.07416867664796));
#47950=CARTESIAN_POINT('Ctrl Pts',(0.79468798149217,0.1080090548681,-5.06888283978931));
#47951=CARTESIAN_POINT('Ctrl Pts',(0.755927796227998,0.233493776169203,
-5.06359700293066));
#47952=CARTESIAN_POINT('Ctrl Pts',(0.717167610963826,0.358978497470306,
-5.05831116607201));
#47953=CARTESIAN_POINT('Ctrl Pts',(0.646487631685767,0.474603714628243,
-5.05302532921336));
#47954=CARTESIAN_POINT('Ctrl Pts',(0.552478696548582,0.566315695067557,
-5.04773949235472));
#47955=CARTESIAN_POINT('Ctrl Pts',(0.458469761411397,0.658027675506871,
-5.04245365549607));
#47956=CARTESIAN_POINT('Ctrl Pts',(0.341131870415083,0.725826419227564,
-5.03716781863742));
#47957=CARTESIAN_POINT('Ctrl Pts',(0.214726924047817,0.761471289484268,
-5.03188198177878));
#47958=CARTESIAN_POINT('Ctrl Pts',(0.0883219776805511,0.797116159740973,
-5.02659614492013));
#47959=CARTESIAN_POINT('Ctrl Pts',(-0.0471500240576684,0.80060715653369,
-5.02131030806148));
#47960=CARTESIAN_POINT('Ctrl Pts',(-0.175223059907049,0.77151996467796,
-5.01602447120283));
#47961=CARTESIAN_POINT('Ctrl Pts',(-0.30329609575643,0.74243277282223,-5.01073863434418));
#47962=CARTESIAN_POINT('Ctrl Pts',(-0.423970165716971,0.680767392318055,
-5.00545279748554));
#47963=CARTESIAN_POINT('Ctrl Pts',(-0.52257787153678,0.594018976801212,
-5.00016696062689));
#47964=CARTESIAN_POINT('Ctrl Pts',(-0.621185577356588,0.507270561284372,
-4.99488112376824));
#47965=CARTESIAN_POINT('Ctrl Pts',(-0.697726919035664,0.395439110754866,
-4.98959528690959));
#47966=CARTESIAN_POINT('Ctrl Pts',(-0.742898635803003,0.272117242272348,
-4.98430945005094));
#47967=CARTESIAN_POINT('Ctrl Pts',(-0.774735450338439,0.185200566617459,
-4.9805840169752));
#47968=CARTESIAN_POINT('Ctrl Pts',(-0.790989829011766,0.09257618163275,
-4.97685858389945));
#47969=CARTESIAN_POINT('Ctrl Pts',(-0.791074454148617,-1.92722236624013E-5,
-4.9731331508237));
#47970=CARTESIAN_POINT('Origin',(0.,0.,-2.94));
#47971=CARTESIAN_POINT('',(-0.791081199896583,1.98953686311731E-5,-4.7446668491763));
#47972=CARTESIAN_POINT('',(-0.791066624166131,1.81968424752065E-5,-4.7731331508237));
#47973=CARTESIAN_POINT('',(-0.7911,-9.68818082805471E-17,-2.94));
#47974=CARTESIAN_POINT('Ctrl Pts',(-0.791081199896583,1.98953686311731E-5,
-4.7446668491763));
#47975=CARTESIAN_POINT('Ctrl Pts',(-0.791116059373008,0.0364627458325065,
-4.7461331060853));
#47976=CARTESIAN_POINT('Ctrl Pts',(-0.78864369690631,0.0729009040620994,
-4.7475993629943));
#47977=CARTESIAN_POINT('Ctrl Pts',(-0.783625203153027,0.108984951686083,
-4.74906561990331));
#47978=CARTESIAN_POINT('Ctrl Pts',(-0.765533599223943,0.239067468446083,
-4.75435145676196));
#47979=CARTESIAN_POINT('Ctrl Pts',(-0.714352651056501,0.364547988526248,
-4.75963729362061));
#47980=CARTESIAN_POINT('Ctrl Pts',(-0.636303176013754,0.470174910969791,
-4.76492313047925));
#47981=CARTESIAN_POINT('Ctrl Pts',(-0.558253700971008,0.575801833413333,
-4.7702089673379));
#47982=CARTESIAN_POINT('Ctrl Pts',(-0.453335699052961,0.661575158220248,
-4.77549480419655));
#47983=CARTESIAN_POINT('Ctrl Pts',(-0.334301488288068,0.717069517996006,
-4.7807806410552));
#47984=CARTESIAN_POINT('Ctrl Pts',(-0.215267277523172,0.772563877771764,
-4.78606647791385));
#47985=CARTESIAN_POINT('Ctrl Pts',(-0.0821168579114289,0.797779272516364,
-4.79135231477249));
#47986=CARTESIAN_POINT('Ctrl Pts',(0.0489659273031979,0.789650882779206,
-4.79663815163114));
#47987=CARTESIAN_POINT('Ctrl Pts',(0.180048712517823,0.781522493042048,
-4.80192398848979));
#47988=CARTESIAN_POINT('Ctrl Pts',(0.309063863335332,0.740050318823134,
-4.80720982534844));
#47989=CARTESIAN_POINT('Ctrl Pts',(0.420330160101931,0.670275119051369,
-4.81249566220709));
#47990=CARTESIAN_POINT('Ctrl Pts',(0.53159645686853,0.600499919279603,-4.81778149906573));
#47991=CARTESIAN_POINT('Ctrl Pts',(0.625113899584218,0.502421693954985,
-4.82306733592438));
#47992=CARTESIAN_POINT('Ctrl Pts',(0.689515857652561,0.387961416581977,
-4.82835317278303));
#47993=CARTESIAN_POINT('Ctrl Pts',(0.753917815720905,0.273501139208968,
-4.83363900964167));
#47994=CARTESIAN_POINT('Ctrl Pts',(0.789204289141904,0.14265880978757,-4.83892484650033));
#47995=CARTESIAN_POINT('Ctrl Pts',(0.791086363497242,0.0113377334309409,
-4.84421068335897));
#47996=CARTESIAN_POINT('Ctrl Pts',(0.79296843785258,-0.119983342925686,
-4.84949652021762));
#47997=CARTESIAN_POINT('Ctrl Pts',(0.761446113142258,-0.251783166217544,
-4.85478235707627));
#47998=CARTESIAN_POINT('Ctrl Pts',(0.700350788195395,-0.36804205219612,
-4.86006819393491));
#47999=CARTESIAN_POINT('Ctrl Pts',(0.639255463248531,-0.484300938174695,
-4.86535403079356));
#48000=CARTESIAN_POINT('Ctrl Pts',(0.548587138065126,-0.585018886839986,
-4.87063986765221));
#48001=CARTESIAN_POINT('Ctrl Pts',(0.439366145635789,-0.657954078017449,
-4.87592570451086));
#48002=CARTESIAN_POINT('Ctrl Pts',(0.330145153206451,-0.730889269194912,
-4.88121154136951));
#48003=CARTESIAN_POINT('Ctrl Pts',(0.202371493531181,-0.776041702884544,
-4.88649737822815));
#48004=CARTESIAN_POINT('Ctrl Pts',(0.0715754885190008,-0.787923300933478,
-4.8917832150868));
#48005=CARTESIAN_POINT('Ctrl Pts',(-0.0592205164931791,-0.799804898982411,
-4.89706905194545));
#48006=CARTESIAN_POINT('Ctrl Pts',(-0.193038866842269,-0.778415661390645,
-4.9023548888041));
#48007=CARTESIAN_POINT('Ctrl Pts',(-0.313614535264138,-0.726355355168322,
-4.90764072566275));
#48008=CARTESIAN_POINT('Ctrl Pts',(-0.434190203686007,-0.674295048945999,
-4.91292656252139));
#48009=CARTESIAN_POINT('Ctrl Pts',(-0.541523190180656,-0.591563674093118,
-4.91821239938004));
#48010=CARTESIAN_POINT('Ctrl Pts',(-0.622567646050043,-0.488216862472354,
-4.92349823623868));
#48011=CARTESIAN_POINT('Ctrl Pts',(-0.70361210191943,-0.38487005085159,
-4.92878407309733));
#48012=CARTESIAN_POINT('Ctrl Pts',(-0.758368027163554,-0.260907802462944,
-4.93406990995598));
#48013=CARTESIAN_POINT('Ctrl Pts',(-0.780180081803669,-0.131397179069651,
-4.93935574681463));
#48014=CARTESIAN_POINT('Ctrl Pts',(-0.787485519460927,-0.0880206241891952,
-4.94112611426852));
#48015=CARTESIAN_POINT('Ctrl Pts',(-0.791095450814012,-0.0440216756909996,
-4.94289648172241));
#48016=CARTESIAN_POINT('Ctrl Pts',(-0.791060709844548,-1.70870917380883E-5,
-4.9446668491763));
#48017=CARTESIAN_POINT('Ctrl Pts',(-0.791074454148617,-1.92722236624013E-5,
-4.9731331508237));
#48018=CARTESIAN_POINT('Ctrl Pts',(-0.79110989952664,-0.0388030306590331,
-4.9715727470408));
#48019=CARTESIAN_POINT('Ctrl Pts',(-0.788308576656797,-0.0775817135126429,
-4.9700123432579));
#48020=CARTESIAN_POINT('Ctrl Pts',(-0.782627328289855,-0.115933781244964,
-4.968451939475));
#48021=CARTESIAN_POINT('Ctrl Pts',(-0.763382212153763,-0.245850649844223,
-4.96316610261635));
#48022=CARTESIAN_POINT('Ctrl Pts',(-0.711089888025977,-0.370872100607207,
-4.9578802657577));
#48023=CARTESIAN_POINT('Ctrl Pts',(-0.632106256090772,-0.475802330417557,
-4.95259442889906));
#48024=CARTESIAN_POINT('Ctrl Pts',(-0.553122624155568,-0.580732560227904,
-4.94730859204041));
#48025=CARTESIAN_POINT('Ctrl Pts',(-0.447447684412945,-0.665571569085619,
-4.94202275518176));
#48026=CARTESIAN_POINT('Ctrl Pts',(-0.327925757328409,-0.720007551557941,
-4.93673691832311));
#48027=CARTESIAN_POINT('Ctrl Pts',(-0.208403830243871,-0.774443534030264,
-4.93145108146446));
#48028=CARTESIAN_POINT('Ctrl Pts',(-0.0750349158174182,-0.798476490117193,
-4.92616524460582));
#48029=CARTESIAN_POINT('Ctrl Pts',(0.0559705856308531,-0.789185320545187,
-4.92087940774717));
#48030=CARTESIAN_POINT('Ctrl Pts',(0.186976087079124,-0.779894150973181,
-4.91559357088852));
#48031=CARTESIAN_POINT('Ctrl Pts',(0.315618175549214,-0.737278855742239,
-4.91030773402987));
#48032=CARTESIAN_POINT('Ctrl Pts',(0.426260975461859,-0.666519135072786,
-4.90502189717122));
#48033=CARTESIAN_POINT('Ctrl Pts',(0.536903775374505,-0.595759414403333,
-4.89973606031258));
#48034=CARTESIAN_POINT('Ctrl Pts',(0.629547286729707,-0.496855268295371,
-4.89445022345393));
#48035=CARTESIAN_POINT('Ctrl Pts',(0.692931101413733,-0.381828057263242,
-4.88916438659528));
#48036=CARTESIAN_POINT('Ctrl Pts',(0.75631491609776,-0.266800846231114,
-4.88387854973664));
#48037=CARTESIAN_POINT('Ctrl Pts',(0.790439034110611,-0.135650570274821,
-4.87859271287799));
#48038=CARTESIAN_POINT('Ctrl Pts',(0.791155820181074,-0.00431796404370287,
-4.87330687601934));
#48039=CARTESIAN_POINT('Ctrl Pts',(0.791872606251537,0.127014642187415,
-4.86802103916069));
#48040=CARTESIAN_POINT('Ctrl Pts',(0.759182060379613,0.258529578693358,
-4.86273520230204));
#48041=CARTESIAN_POINT('Ctrl Pts',(0.697057573497852,0.374241787951529,
-4.85744936544339));
#48042=CARTESIAN_POINT('Ctrl Pts',(0.634933086616092,0.4899539972097,-4.85216352858475));
#48043=CARTESIAN_POINT('Ctrl Pts',(0.543374658724495,0.589863479220098,
-4.8468776917261));
#48044=CARTESIAN_POINT('Ctrl Pts',(0.433510810852,0.661826679346121,-4.84159185486745));
#48045=CARTESIAN_POINT('Ctrl Pts',(0.323646962979506,0.733789879472143,
-4.83630601800881));
#48046=CARTESIAN_POINT('Ctrl Pts',(0.195477695126116,0.777806797713789,
-4.83102018115015));
#48047=CARTESIAN_POINT('Ctrl Pts',(0.0645814136211574,0.788527372787123,
-4.82573434429151));
#48048=CARTESIAN_POINT('Ctrl Pts',(-0.0663148678837991,0.799247947860457,
-4.82044850743286));
#48049=CARTESIAN_POINT('Ctrl Pts',(-0.199938163040322,0.776672179765479,
-4.81516267057421));
#48050=CARTESIAN_POINT('Ctrl Pts',(-0.320047152678255,0.723544053035068,
-4.80987683371557));
#48051=CARTESIAN_POINT('Ctrl Pts',(-0.440156142316193,0.670415926304655,
-4.80459099685692));
#48052=CARTESIAN_POINT('Ctrl Pts',(-0.54675082643554,0.586735440938804,
-4.79930515999826));
#48053=CARTESIAN_POINT('Ctrl Pts',(-0.626875093719053,0.482673588975613,
-4.79401932313962));
#48054=CARTESIAN_POINT('Ctrl Pts',(-0.706999361002566,0.378611737012422,
-4.78873348628097));
#48055=CARTESIAN_POINT('Ctrl Pts',(-0.760653211450246,0.254168518451889,
-4.78344764942233));
#48056=CARTESIAN_POINT('Ctrl Pts',(-0.781315257389323,0.124469454849486,
-4.77816181256368));
#48057=CARTESIAN_POINT('Ctrl Pts',(-0.787867511564775,0.0833398768034945,
-4.77648559198369));
#48058=CARTESIAN_POINT('Ctrl Pts',(-0.791102036830354,0.0416817593429142,
-4.7748093714037));
#48059=CARTESIAN_POINT('Ctrl Pts',(-0.791066624166131,1.81968424752065E-5,
-4.7731331508237));
#48060=CARTESIAN_POINT('Origin',(0.,0.,-2.94));
#48061=CARTESIAN_POINT('',(-0.791147068928682,-1.37605406554386E-5,-4.54466684917629));
#48062=CARTESIAN_POINT('',(-0.791158453049048,-9.36744769638833E-6,-4.5731331508237));
#48063=CARTESIAN_POINT('',(-0.7911,-9.68818082805471E-17,-2.94));
#48064=CARTESIAN_POINT('Ctrl Pts',(-0.791147068928682,-1.37605406554386E-5,
-4.54466684917629));
#48065=CARTESIAN_POINT('Ctrl Pts',(-0.791051964156756,0.116845203154218,
-4.54936973044819));
#48066=CARTESIAN_POINT('Ctrl Pts',(-0.764828877004105,0.233745430424912,
-4.55407261172009));
#48067=CARTESIAN_POINT('Ctrl Pts',(-0.71471592230546,0.339304183755074,
-4.55877549299199));
#48068=CARTESIAN_POINT('Ctrl Pts',(-0.658391110402443,0.457947695433684,
-4.56406132985064));
#48069=CARTESIAN_POINT('Ctrl Pts',(-0.571886716359079,0.562263754533416,
-4.56934716670928));
#48070=CARTESIAN_POINT('Ctrl Pts',(-0.465716965794738,0.639573206506951,
-4.57463300356793));
#48071=CARTESIAN_POINT('Ctrl Pts',(-0.359547215230401,0.716882658480484,
-4.57991884042658));
#48072=CARTESIAN_POINT('Ctrl Pts',(-0.233712108145087,0.767185503327821,
-4.58520467728523));
#48073=CARTESIAN_POINT('Ctrl Pts',(-0.103506343974174,0.784367653251803,
-4.59049051414388));
#48074=CARTESIAN_POINT('Ctrl Pts',(0.0266994201967425,0.801549803175786,
-4.59577635100253));
#48075=CARTESIAN_POINT('Ctrl Pts',(0.161275841453259,0.785611258176413,
-4.60106218786117));
#48076=CARTESIAN_POINT('Ctrl Pts',(0.283865752373001,0.738489277742304,
-4.60634802471982));
#48077=CARTESIAN_POINT('Ctrl Pts',(0.406455663292742,0.691367297308196,
-4.61163386157847));
#48078=CARTESIAN_POINT('Ctrl Pts',(0.517059063875708,0.613061881439353,
-4.61691969843712));
#48079=CARTESIAN_POINT('Ctrl Pts',(0.602232601089266,0.513090706304351,
-4.62220553529576));
#48080=CARTESIAN_POINT('Ctrl Pts',(0.687406138302824,0.413119531169349,
-4.62749137215441));
#48081=CARTESIAN_POINT('Ctrl Pts',(0.747149812146974,0.291482596768187,
-4.63277720901306));
#48082=CARTESIAN_POINT('Ctrl Pts',(0.774202043911476,0.162964333257111,
-4.63806304587171));
#48083=CARTESIAN_POINT('Ctrl Pts',(0.801254275675977,0.0344460697460355,
-4.64334888273035));
#48084=CARTESIAN_POINT('Ctrl Pts',(0.795615065360831,-0.100953522874955,
-4.648634719589));
#48085=CARTESIAN_POINT('Ctrl Pts',(0.757969833981053,-0.226777224353276,
-4.65392055644765));
#48086=CARTESIAN_POINT('Ctrl Pts',(0.720324602601275,-0.352600925831596,
-4.6592063933063));
#48087=CARTESIAN_POINT('Ctrl Pts',(0.650673350156865,-0.468848736167248,
-4.66449223016494));
#48088=CARTESIAN_POINT('Ctrl Pts',(0.557481877616328,-0.561391249343998,
-4.66977806702359));
#48089=CARTESIAN_POINT('Ctrl Pts',(0.46429040507579,-0.653933762520748,
-4.67506390388224));
#48090=CARTESIAN_POINT('Ctrl Pts',(0.347558712439126,-0.722770978538597,
-4.68034974074089));
#48091=CARTESIAN_POINT('Ctrl Pts',(0.221475019471191,-0.759536038948039,
-4.68563557759954));
#48092=CARTESIAN_POINT('Ctrl Pts',(0.0953913265032548,-0.796301099357482,
-4.69092141445819));
#48093=CARTESIAN_POINT('Ctrl Pts',(-0.0400443667959528,-0.800994004158517,
-4.69620725131683));
#48094=CARTESIAN_POINT('Ctrl Pts',(-0.168370452296446,-0.773044351576371,
-4.70149308817548));
#48095=CARTESIAN_POINT('Ctrl Pts',(-0.296696537796939,-0.745094698994224,
-4.70677892503413));
#48096=CARTESIAN_POINT('Ctrl Pts',(-0.417913015498719,-0.684502489028894,
-4.71206476189278));
#48097=CARTESIAN_POINT('Ctrl Pts',(-0.517286559893452,-0.598632436194564,
-4.71735059875143));
#48098=CARTESIAN_POINT('Ctrl Pts',(-0.616660104288183,-0.512762383360237,
-4.72263643561007));
#48099=CARTESIAN_POINT('Ctrl Pts',(-0.694190715375869,-0.401614487656911,
-4.72792227246872));
#48100=CARTESIAN_POINT('Ctrl Pts',(-0.74045489107435,-0.278698283085334,
-4.73320810932737));
#48101=CARTESIAN_POINT('Ctrl Pts',(-0.773885684080305,-0.189878237551815,
-4.73702768927701));
#48102=CARTESIAN_POINT('Ctrl Pts',(-0.790990391419302,-0.0949132504428775,
-4.74084726922665));
#48103=CARTESIAN_POINT('Ctrl Pts',(-0.791081199896583,1.98953686311731E-5,
-4.7446668491763));
#48104=CARTESIAN_POINT('Ctrl Pts',(-0.791066624166131,1.81968424752065E-5,
-4.7731331508237));
#48105=CARTESIAN_POINT('Ctrl Pts',(-0.790990365629054,-0.0897011844987339,
-4.76952353454505));
#48106=CARTESIAN_POINT('Ctrl Pts',(-0.775750614440565,-0.179445815806044,
-4.76591391826639));
#48107=CARTESIAN_POINT('Ctrl Pts',(-0.745824609176676,-0.263992100196821,
-4.76230430198773));
#48108=CARTESIAN_POINT('Ctrl Pts',(-0.70200167359448,-0.387799682996452,
-4.75701846512908));
#48109=CARTESIAN_POINT('Ctrl Pts',(-0.626685560999614,-0.50045993995144,
-4.75173262827044));
#48110=CARTESIAN_POINT('Ctrl Pts',(-0.529030610999373,-0.588279516255242,
-4.74644679141179));
#48111=CARTESIAN_POINT('Ctrl Pts',(-0.431375660999132,-0.676099092559043,
-4.74116095455315));
#48112=CARTESIAN_POINT('Ctrl Pts',(-0.311381873593517,-0.739077988211657,
-4.7358751176945));
#48113=CARTESIAN_POINT('Ctrl Pts',(-0.183633961705585,-0.769561397633862,
-4.73058928083585));
#48114=CARTESIAN_POINT('Ctrl Pts',(-0.0558860498176521,-0.800044807056067,
-4.7253034439772));
#48115=CARTESIAN_POINT('Ctrl Pts',(0.0796159865525981,-0.798032730247862,
-4.72001760711855));
#48116=CARTESIAN_POINT('Ctrl Pts',(0.206402475568996,-0.763769726225687,
-4.71473177025991));
#48117=CARTESIAN_POINT('Ctrl Pts',(0.333188964585392,-0.729506722203513,
-4.70944593340126));
#48118=CARTESIAN_POINT('Ctrl Pts',(0.451259906247936,-0.66299279096737,
-4.70416009654261));
#48119=CARTESIAN_POINT('Ctrl Pts',(0.546264301009608,-0.572312406000739,
-4.69887425968396));
#48120=CARTESIAN_POINT('Ctrl Pts',(0.641268695771284,-0.481632021034104,
-4.69358842282531));
#48121=CARTESIAN_POINT('Ctrl Pts',(0.713206543632088,-0.36678518233698,
-4.68830258596667));
#48122=CARTESIAN_POINT('Ctrl Pts',(0.753334118087197,-0.241731014033485,
-4.68301674910802));
#48123=CARTESIAN_POINT('Ctrl Pts',(0.793461692542305,-0.116676845729994,
-4.67773091224937));
#48124=CARTESIAN_POINT('Ctrl Pts',(0.801778993591721,0.0185846521798675,
-4.67244507539072));
#48125=CARTESIAN_POINT('Ctrl Pts',(0.777275090163736,0.147613044243476,
-4.66715923853207));
#48126=CARTESIAN_POINT('Ctrl Pts',(0.752771186735752,0.276641436307085,
-4.66187340167343));
#48127=CARTESIAN_POINT('Ctrl Pts',(0.695446078830367,0.39943672252444,-4.65658756481478));
#48128=CARTESIAN_POINT('Ctrl Pts',(0.61226737918954,0.501073680211048,-4.65130172795613));
#48129=CARTESIAN_POINT('Ctrl Pts',(0.529088679548712,0.602710637897657,
-4.64601589109748));
#48130=CARTESIAN_POINT('Ctrl Pts',(0.420056388172441,0.683189267053518,
-4.64073005423883));
#48131=CARTESIAN_POINT('Ctrl Pts',(0.29842289673406,0.732727747068938,-4.63544421738019));
#48132=CARTESIAN_POINT('Ctrl Pts',(0.17678940529568,0.782266227084359,-4.63015838052154));
#48133=CARTESIAN_POINT('Ctrl Pts',(0.0425547137951911,0.80086455795934,
-4.62487254366289));
#48134=CARTESIAN_POINT('Ctrl Pts',(-0.0879655460819782,0.78626219502299,
-4.61958670680424));
#48135=CARTESIAN_POINT('Ctrl Pts',(-0.218485805959148,0.77165983208664,
-4.6143008699456));
#48136=CARTESIAN_POINT('Ctrl Pts',(-0.345291634212997,0.72385677533896,
-4.60901503308695));
#48137=CARTESIAN_POINT('Ctrl Pts',(-0.452970344553351,0.648663274415231,
-4.6037291962283));
#48138=CARTESIAN_POINT('Ctrl Pts',(-0.560649054893706,0.573469773491501,
-4.59844335936965));
#48139=CARTESIAN_POINT('Ctrl Pts',(-0.649200647320564,0.470885828391724,
-4.59315752251101));
#48140=CARTESIAN_POINT('Ctrl Pts',(-0.707862068326336,0.353380062885038,
-4.58787168565236));
#48141=CARTESIAN_POINT('Ctrl Pts',(-0.762384081252103,0.244166021425364,
-4.58295884070947));
#48142=CARTESIAN_POINT('Ctrl Pts',(-0.791085453716163,0.122061757479741,
-4.57804599576659));
#48143=CARTESIAN_POINT('Ctrl Pts',(-0.791158453049048,-9.36744769638833E-6,
-4.5731331508237));
#48144=CARTESIAN_POINT('Origin',(0.,0.,-2.94));
#48145=CARTESIAN_POINT('',(-0.791032667499796,-2.47978686473971E-7,-4.34466684917629));
#48146=CARTESIAN_POINT('',(-0.791034555886587,-5.04054740280758E-6,-4.3731331508237));
#48147=CARTESIAN_POINT('',(-0.7911,-9.68818082805471E-17,-2.94));
#48148=CARTESIAN_POINT('Ctrl Pts',(-0.791032667499796,-2.47978686473971E-7,
-4.34466684917629));
#48149=CARTESIAN_POINT('Ctrl Pts',(-0.791031946004233,0.0659665420417525,
-4.34732051795244));
#48150=CARTESIAN_POINT('Ctrl Pts',(-0.782871044353607,0.131933507406664,
-4.34997418672858));
#48151=CARTESIAN_POINT('Ctrl Pts',(-0.766552074213921,0.195816486101084,
-4.35262785550472));
#48152=CARTESIAN_POINT('Ctrl Pts',(-0.734046354346008,0.323064847486256,
-4.35791369236337));
#48153=CARTESIAN_POINT('Ctrl Pts',(-0.669172219886227,0.442044665325261,
-4.36319952922202));
#48154=CARTESIAN_POINT('Ctrl Pts',(-0.57981483428916,0.538294470200906,
-4.36848536608067));
#48155=CARTESIAN_POINT('Ctrl Pts',(-0.490457448692093,0.634544275076551,
-4.37377120293932));
#48156=CARTESIAN_POINT('Ctrl Pts',(-0.376616811957741,0.708064066988836,
-4.37905703979796));
#48157=CARTESIAN_POINT('Ctrl Pts',(-0.25212974882217,0.749917841146289,
-4.38434287665661));
#48158=CARTESIAN_POINT('Ctrl Pts',(-0.127642685686599,0.791771615303741,
-4.38962871351526));
#48159=CARTESIAN_POINT('Ctrl Pts',(0.00749080385018974,0.801959371706361,
-4.39491455037391));
#48160=CARTESIAN_POINT('Ctrl Pts',(0.136845843185855,0.779242833726043,
-4.40020038723256));
#48161=CARTESIAN_POINT('Ctrl Pts',(0.266200882521519,0.756526295745724,
-4.4054862240912));
#48162=CARTESIAN_POINT('Ctrl Pts',(0.38977747165606,0.700905463382468,-4.41077206094985));
#48163=CARTESIAN_POINT('Ctrl Pts',(0.492555423998938,0.619140802241192,
-4.4160578978085));
#48164=CARTESIAN_POINT('Ctrl Pts',(0.595333376341813,0.537376141099918,
-4.42134373466715));
#48165=CARTESIAN_POINT('Ctrl Pts',(0.677312691893027,0.429467651180626,
-4.42662957152579));
#48166=CARTESIAN_POINT('Ctrl Pts',(0.72852914826412,0.308531131071399,-4.43191540838444));
#48167=CARTESIAN_POINT('Ctrl Pts',(0.779745604635215,0.187594610962168,
-4.43720124524309));
#48168=CARTESIAN_POINT('Ctrl Pts',(0.800199201826187,0.0536300606630008,
-4.44248708210174));
#48169=CARTESIAN_POINT('Ctrl Pts',(0.78740389576989,-0.0770797226061498,
-4.44777291896039));
#48170=CARTESIAN_POINT('Ctrl Pts',(0.774608589713593,-0.2077895058753,-4.45305875581904));
#48171=CARTESIAN_POINT('Ctrl Pts',(0.728564380410028,-0.335244522114434,
-4.45834459267768));
#48172=CARTESIAN_POINT('Ctrl Pts',(0.654867737384667,-0.443953179111636,
-4.46363042953633));
#48173=CARTESIAN_POINT('Ctrl Pts',(0.581171094359306,-0.552661836108837,
-4.46891626639497));
#48174=CARTESIAN_POINT('Ctrl Pts',(0.479822017612149,-0.642624133864105,
-4.47420210325363));
#48175=CARTESIAN_POINT('Ctrl Pts',(0.363139038138284,-0.702905553890879,
-4.47948794011227));
#48176=CARTESIAN_POINT('Ctrl Pts',(0.246456058664419,-0.763186973917653,
-4.48477377697092));
#48177=CARTESIAN_POINT('Ctrl Pts',(0.114439176463847,-0.793787516215932,
-4.49005961382957));
#48178=CARTESIAN_POINT('Ctrl Pts',(-0.0168655416667924,-0.790987820522495,
-4.49534545068821));
#48179=CARTESIAN_POINT('Ctrl Pts',(-0.148170259797432,-0.788188124829056,
-4.50063128754686));
#48180=CARTESIAN_POINT('Ctrl Pts',(-0.27876281385814,-0.751988191143901,
-4.50591712440551));
#48181=CARTESIAN_POINT('Ctrl Pts',(-0.392770257823586,-0.686787960931054,
-4.51120296126416));
#48182=CARTESIAN_POINT('Ctrl Pts',(-0.506777701789033,-0.621587730718207,
-4.51648879812281));
#48183=CARTESIAN_POINT('Ctrl Pts',(-0.604200035659218,-0.527387203977669,
-4.52177463498146));
#48184=CARTESIAN_POINT('Ctrl Pts',(-0.673196006628379,-0.415636037140963,
-4.5270604718401));
#48185=CARTESIAN_POINT('Ctrl Pts',(-0.74219197759754,-0.303884870304259,
-4.53234630869875));
#48186=CARTESIAN_POINT('Ctrl Pts',(-0.782761585665677,-0.174583063371387,
-4.53763214555739));
#48187=CARTESIAN_POINT('Ctrl Pts',(-0.789973774818412,-0.0434466777762086,
-4.54291798241604));
#48188=CARTESIAN_POINT('Ctrl Pts',(-0.790769180744043,-0.0289841261210445,
-4.54350093800279));
#48189=CARTESIAN_POINT('Ctrl Pts',(-0.791158857841673,-0.0144992603458212,
-4.54408389358954));
#48190=CARTESIAN_POINT('Ctrl Pts',(-0.791147068928682,-1.37605406554386E-5,
-4.54466684917629));
#48191=CARTESIAN_POINT('Ctrl Pts',(-0.791158453049048,-9.36744769638833E-6,
-4.5731331508237));
#48192=CARTESIAN_POINT('Ctrl Pts',(-0.791163995288084,-0.00927722411226468,
-4.57276015890794));
#48193=CARTESIAN_POINT('Ctrl Pts',(-0.791004520259269,-0.0185448897596832,
-4.57238716699218));
#48194=CARTESIAN_POINT('Ctrl Pts',(-0.790678799237191,-0.0278067088434459,
-4.57201417507641));
#48195=CARTESIAN_POINT('Ctrl Pts',(-0.786062859557592,-0.159060129151653,
-4.56672833821777));
#48196=CARTESIAN_POINT('Ctrl Pts',(-0.748059730613709,-0.289139383854475,
-4.56144250135912));
#48197=CARTESIAN_POINT('Ctrl Pts',(-0.681288524259648,-0.402233916188058,
-4.55615666450047));
#48198=CARTESIAN_POINT('Ctrl Pts',(-0.614517317905586,-0.515328448521644,
-4.55087082764182));
#48199=CARTESIAN_POINT('Ctrl Pts',(-0.51897803414135,-0.61143825848599,
-4.54558499078317));
#48200=CARTESIAN_POINT('Ctrl Pts',(-0.406283049379935,-0.678881624737636,
-4.54029915392453));
#48201=CARTESIAN_POINT('Ctrl Pts',(-0.293588064618524,-0.74632499098928,
-4.53501331706588));
#48202=CARTESIAN_POINT('Ctrl Pts',(-0.163737378859937,-0.785101913528223,
-4.52972748020723));
#48203=CARTESIAN_POINT('Ctrl Pts',(-0.0325137673261076,-0.790499229319128,
-4.52444164334859));
#48204=CARTESIAN_POINT('Ctrl Pts',(0.0987098442077254,-0.795896545110033,
-4.51915580648994));
#48205=CARTESIAN_POINT('Ctrl Pts',(0.231306381516804,-0.767914254152898,
-4.51386996963129));
#48206=CARTESIAN_POINT('Ctrl Pts',(0.349159323295675,-0.709953479867221,
-4.50858413277264));
#48207=CARTESIAN_POINT('Ctrl Pts',(0.467012265074544,-0.651992705581545,
-4.50329829591399));
#48208=CARTESIAN_POINT('Ctrl Pts',(0.570121611323203,-0.56405344796733,
-4.49801245905534));
#48209=CARTESIAN_POINT('Ctrl Pts',(0.645954878091993,-0.456824333950184,
-4.4927266221967));
#48210=CARTESIAN_POINT('Ctrl Pts',(0.721788144860783,-0.349595219933038,
-4.48744078533805));
#48211=CARTESIAN_POINT('Ctrl Pts',(0.770345332149699,-0.223076249512961,
-4.4821549484794));
#48212=CARTESIAN_POINT('Ctrl Pts',(0.785724529099256,-0.0926452426820873,
-4.47686911162076));
#48213=CARTESIAN_POINT('Ctrl Pts',(0.801103726048813,0.037785764148786,
-4.47158327476211));
#48214=CARTESIAN_POINT('Ctrl Pts',(0.783304932659011,0.172128807390459,
-4.46629743790346));
#48215=CARTESIAN_POINT('Ctrl Pts',(0.73449151336379,0.294055085683687,-4.46101160104481));
#48216=CARTESIAN_POINT('Ctrl Pts',(0.685678094068569,0.415981363976914,
-4.45572576418616));
#48217=CARTESIAN_POINT('Ctrl Pts',(0.605850048867929,0.525490877321699,
-4.45043992732752));
#48218=CARTESIAN_POINT('Ctrl Pts',(0.504710122775864,0.60927322982997,-4.44515409046887));
#48219=CARTESIAN_POINT('Ctrl Pts',(0.403570196683798,0.693055582338243,
-4.43986825361022));
#48220=CARTESIAN_POINT('Ctrl Pts',(0.28111838970031,0.751110774010002,-4.43458241675157));
#48221=CARTESIAN_POINT('Ctrl Pts',(0.152238176131666,0.776382453657973,
-4.42929657989292));
#48222=CARTESIAN_POINT('Ctrl Pts',(0.0233579625630229,0.801654133305943,
-4.42401074303427));
#48223=CARTESIAN_POINT('Ctrl Pts',(-0.111950657590775,0.794142300930125,
-4.41872490617563));
#48224=CARTESIAN_POINT('Ctrl Pts',(-0.237241521377244,0.754759986455616,
-4.41343906931698));
#48225=CARTESIAN_POINT('Ctrl Pts',(-0.362532385163711,0.715377671981108,
-4.40815323245834));
#48226=CARTESIAN_POINT('Ctrl Pts',(-0.477805492582847,0.644124875407914,
-4.40286739559969));
#48227=CARTESIAN_POINT('Ctrl Pts',(-0.569049908437045,0.549662058293695,
-4.39758155874104));
#48228=CARTESIAN_POINT('Ctrl Pts',(-0.660294324291243,0.455199241179475,
-4.39229572188239));
#48229=CARTESIAN_POINT('Ctrl Pts',(-0.727510048580498,0.337526403524228,
-4.38700988502374));
#48230=CARTESIAN_POINT('Ctrl Pts',(-0.762527307986792,0.210946157097699,
-4.38172404816509));
#48231=CARTESIAN_POINT('Ctrl Pts',(-0.78149810919141,0.14237058230678,-4.37886041571796));
#48232=CARTESIAN_POINT('Ctrl Pts',(-0.7910186841546,0.0711806894600302,
-4.37599678327083));
#48233=CARTESIAN_POINT('Ctrl Pts',(-0.791034555886587,-5.04054740280758E-6,
-4.3731331508237));
#48234=CARTESIAN_POINT('Origin',(0.,0.,-2.94));
#48235=CARTESIAN_POINT('',(-0.79114572203675,1.41578566767164E-5,-4.1446668491763));
#48236=CARTESIAN_POINT('',(-0.791131276639148,1.74428956908455E-5,-4.1731331508237));
#48237=CARTESIAN_POINT('',(-0.7911,-9.68818082805471E-17,-2.94));
#48238=CARTESIAN_POINT('Ctrl Pts',(-0.79114572203675,1.41578566767164E-5,
-4.1446668491763));
#48239=CARTESIAN_POINT('Ctrl Pts',(-0.79115820984817,0.015033989046388,
-4.14527130545668));
#48240=CARTESIAN_POINT('Ctrl Pts',(-0.790739241182227,0.030053123953994,
-4.14587576173707));
#48241=CARTESIAN_POINT('Ctrl Pts',(-0.789884112929677,0.0450473845182785,
-4.14648021801746));
#48242=CARTESIAN_POINT('Ctrl Pts',(-0.782406204960389,0.176168886156055,
-4.15176605487611));
#48243=CARTESIAN_POINT('Ctrl Pts',(-0.741574664137056,0.305388217716395,
-4.15705189173475));
#48244=CARTESIAN_POINT('Ctrl Pts',(-0.672352383239296,0.416999342281352,
-4.1623377285934));
#48245=CARTESIAN_POINT('Ctrl Pts',(-0.603130102341536,0.528610466846308,
-4.16762356545205));
#48246=CARTESIAN_POINT('Ctrl Pts',(-0.505517081369349,0.622613384415881,
-4.1729094023107));
#48247=CARTESIAN_POINT('Ctrl Pts',(-0.391377750300425,0.687582457077272,
-4.17819523916935));
#48248=CARTESIAN_POINT('Ctrl Pts',(-0.2772384192315,0.752551529738663,-4.183481076028));
#48249=CARTESIAN_POINT('Ctrl Pts',(-0.146572778065838,0.788486757491872,
-4.18876691288664));
#48250=CARTESIAN_POINT('Ctrl Pts',(-0.0152626562423773,0.791020372705449,
-4.19405274974529));
#48251=CARTESIAN_POINT('Ctrl Pts',(0.116047465581084,0.793553987919027,
-4.19933858660394));
#48252=CARTESIAN_POINT('Ctrl Pts',(0.248002068062344,0.762685990592973,
-4.20462442346258));
#48253=CARTESIAN_POINT('Ctrl Pts',(0.364562654228557,0.702168248963502,
-4.20991026032123));
#48254=CARTESIAN_POINT('Ctrl Pts',(0.48112324039477,0.641650507334031,-4.21519609717988));
#48255=CARTESIAN_POINT('Ctrl Pts',(0.582289810245937,0.551483021401144,
-4.22048193403853));
#48256=CARTESIAN_POINT('Ctrl Pts',(0.655766015691118,0.442625249364784,
-4.22576777089718));
#48257=CARTESIAN_POINT('Ctrl Pts',(0.7292422211363,0.333767477328423,-4.23105360775583));
#48258=CARTESIAN_POINT('Ctrl Pts',(0.775028062175496,0.206219419188591,
-4.23633944461447));
#48259=CARTESIAN_POINT('Ctrl Pts',(0.787558472800413,0.0754839759877756,
-4.24162528147312));
#48260=CARTESIAN_POINT('Ctrl Pts',(0.800088883425329,-0.0552514672130398,
-4.24691111833177));
#48261=CARTESIAN_POINT('Ctrl Pts',(0.779363863635967,-0.189174295474838,
-4.25219695519042));
#48262=CARTESIAN_POINT('Ctrl Pts',(0.727902447713082,-0.310006782706354,
-4.25748279204906));
#48263=CARTESIAN_POINT('Ctrl Pts',(0.676441031790198,-0.430839269937868,
-4.26276862890771));
#48264=CARTESIAN_POINT('Ctrl Pts',(0.594243219733788,-0.538581416139105,
-4.26805446576636));
#48265=CARTESIAN_POINT('Ctrl Pts',(0.491299791213923,-0.620137641063495,
-4.27334030262501));
#48266=CARTESIAN_POINT('Ctrl Pts',(0.388356362694056,-0.701693865987887,
-4.27862613948366));
#48267=CARTESIAN_POINT('Ctrl Pts',(0.264667317710735,-0.757064169635434,
-4.2839119763423));
#48268=CARTESIAN_POINT('Ctrl Pts',(0.135266511364388,-0.779518537056015,
-4.28919781320095));
#48269=CARTESIAN_POINT('Ctrl Pts',(0.00586570501804362,-0.801972904476595,
-4.2944836500596));
#48270=CARTESIAN_POINT('Ctrl Pts',(-0.129246862691322,-0.791511335670206,
-4.29976948691825));
#48271=CARTESIAN_POINT('Ctrl Pts',(-0.253648858116741,-0.749405387948815,
-4.3050553237769));
#48272=CARTESIAN_POINT('Ctrl Pts',(-0.378050853542157,-0.707299440227425,
-4.31034116063554));
#48273=CARTESIAN_POINT('Ctrl Pts',(-0.491742276683628,-0.633549113591034,
-4.31562699749419));
#48274=CARTESIAN_POINT('Ctrl Pts',(-0.580904439055834,-0.537118433304861,
-4.32091283435284));
#48275=CARTESIAN_POINT('Ctrl Pts',(-0.670066601428042,-0.440687753018685,
-4.32619867121149));
#48276=CARTESIAN_POINT('Ctrl Pts',(-0.734699503030983,-0.321576719082726,
-4.33148450807013));
#48277=CARTESIAN_POINT('Ctrl Pts',(-0.766947301194431,-0.194262749649077,
-4.33677034492878));
#48278=CARTESIAN_POINT('Ctrl Pts',(-0.783005614632164,-0.130864696367882,
-4.33940251301129));
#48279=CARTESIAN_POINT('Ctrl Pts',(-0.79103338314962,-0.0654325584305906,
-4.34203468109379));
#48280=CARTESIAN_POINT('Ctrl Pts',(-0.791032667499796,-2.47978686473971E-7,
-4.34466684917629));
#48281=CARTESIAN_POINT('Ctrl Pts',(-0.791034555886587,-5.04054740280758E-6,
-4.3731331508237));
#48282=CARTESIAN_POINT('Ctrl Pts',(-0.791047980996111,-0.0602175127988069,
-4.37071094641218));
#48283=CARTESIAN_POINT('Ctrl Pts',(-0.784261144919877,-0.120427006693712,
-4.36828874200067));
#48284=CARTESIAN_POINT('Ctrl Pts',(-0.770641079578282,-0.179048884627327,
-4.36586653758915));
#48285=CARTESIAN_POINT('Ctrl Pts',(-0.740918797240146,-0.306976024728015,
-4.3605807007305));
#48286=CARTESIAN_POINT('Ctrl Pts',(-0.678655438040537,-0.427342649731578,
-4.35529486387185));
#48287=CARTESIAN_POINT('Ctrl Pts',(-0.591418837274813,-0.525518729957724,
-4.3500090270132));
#48288=CARTESIAN_POINT('Ctrl Pts',(-0.504182236509089,-0.623694810183869,
-4.34472319015456));
#48289=CARTESIAN_POINT('Ctrl Pts',(-0.39197239417725,-0.6996803456326,-4.33943735329591));
#48290=CARTESIAN_POINT('Ctrl Pts',(-0.268427919185097,-0.744239631316306,
-4.33415151643726));
#48291=CARTESIAN_POINT('Ctrl Pts',(-0.144883444192945,-0.788798917000011,
-4.32886567957861));
#48292=CARTESIAN_POINT('Ctrl Pts',(-0.0100043365404776,-0.80193195291869,
-4.32357984271997));
#48293=CARTESIAN_POINT('Ctrl Pts',(0.119815446160315,-0.782042476775574,
-4.31829400586132));
#48294=CARTESIAN_POINT('Ctrl Pts',(0.249635228861107,-0.762153000632459,
-4.31300816900267));
#48295=CARTESIAN_POINT('Ctrl Pts',(0.374395686610229,-0.709241012427549,
-4.30772233214402));
#48296=CARTESIAN_POINT('Ctrl Pts',(0.478932738835162,-0.629737729766704,
-4.30243649528538));
#48297=CARTESIAN_POINT('Ctrl Pts',(0.583469791060094,-0.550234447105859,
-4.29715065842673));
#48298=CARTESIAN_POINT('Ctrl Pts',(0.667783437760838,-0.44413986998908,
-4.29186482156808));
#48299=CARTESIAN_POINT('Ctrl Pts',(0.721625728945871,-0.324349323944434,
-4.28657898470943));
#48300=CARTESIAN_POINT('Ctrl Pts',(0.775468020130904,-0.204558777899789,
-4.28129314785078));
#48301=CARTESIAN_POINT('Ctrl Pts',(0.798838955800226,-0.0710722629272758,
-4.27600731099214));
#48302=CARTESIAN_POINT('Ctrl Pts',(0.788897902327297,0.0598855268279594,
-4.27072147413349));
#48303=CARTESIAN_POINT('Ctrl Pts',(0.778956848854367,0.190843316583198,
-4.26543563727484));
#48304=CARTESIAN_POINT('Ctrl Pts',(0.735703806239186,0.319272381121158,
-4.26014980041619));
#48305=CARTESIAN_POINT('Ctrl Pts',(0.664395990069578,0.429562736977192,
-4.25486396355754));
#48306=CARTESIAN_POINT('Ctrl Pts',(0.593088173899971,0.539853092833225,
-4.2495781266989));
#48307=CARTESIAN_POINT('Ctrl Pts',(0.493725584175939,0.632004740007326,
-4.24429228984025));
#48308=CARTESIAN_POINT('Ctrl Pts',(0.378385303201064,0.694817054296532,
-4.2390064529816));
#48309=CARTESIAN_POINT('Ctrl Pts',(0.263045022226192,0.757629368585737,
-4.23372061612296));
#48310=CARTESIAN_POINT('Ctrl Pts',(0.131727050000475,0.791102349990045,
-4.2284347792643));
#48311=CARTESIAN_POINT('Ctrl Pts',(0.000392503911405343,0.791167506006503,
-4.22314894240566));
#48312=CARTESIAN_POINT('Ctrl Pts',(-0.130942042177665,0.791232662022961,
-4.21786310554701));
#48313=CARTESIAN_POINT('Ctrl Pts',(-0.262293162130093,0.75788999265157,
-4.21257726868836));
#48314=CARTESIAN_POINT('Ctrl Pts',(-0.377695709599153,0.695192151545358,
-4.20729143182972));
#48315=CARTESIAN_POINT('Ctrl Pts',(-0.493098257068215,0.632494310439145,
-4.20200559497107));
#48316=CARTESIAN_POINT('Ctrl Pts',(-0.592552232053908,0.540441297598112,
-4.19671975811242));
#48317=CARTESIAN_POINT('Ctrl Pts',(-0.663969444779212,0.430221748659288,
-4.19143392125377));
#48318=CARTESIAN_POINT('Ctrl Pts',(-0.735386657504514,0.320002199720466,
-4.18614808439512));
#48319=CARTESIAN_POINT('Ctrl Pts',(-0.778767107969428,0.191616114683848,
-4.18086224753648));
#48320=CARTESIAN_POINT('Ctrl Pts',(-0.788838094726788,0.0606682530462416,
-4.17557641067783));
#48321=CARTESIAN_POINT('Ctrl Pts',(-0.790389790846925,0.0404923463810076,
-4.17476199072645));
#48322=CARTESIAN_POINT('Ctrl Pts',(-0.791150741084666,0.0202556247378911,
-4.17394757077508));
#48323=CARTESIAN_POINT('Ctrl Pts',(-0.791131276639148,1.74428956908455E-5,
-4.1731331508237));
#48324=CARTESIAN_POINT('Origin',(0.,0.,-2.94));
#48325=CARTESIAN_POINT('',(-0.791082780681432,-2.0004826913167E-5,-3.9446668491763));
#48326=CARTESIAN_POINT('',(-0.791098791730102,-2.0404891719479E-5,-3.9731331508237));
#48327=CARTESIAN_POINT('',(-0.7911,-9.68818082805471E-17,-2.94));
#48328=CARTESIAN_POINT('Ctrl Pts',(-0.791082780681432,-2.0004826913167E-5,
-3.9446668491763));
#48329=CARTESIAN_POINT('Ctrl Pts',(-0.790990652476222,0.0954469785790556,
-3.94850792981958));
#48330=CARTESIAN_POINT('Ctrl Pts',(-0.773688524716814,0.190946450742593,
-3.95234901046286));
#48331=CARTESIAN_POINT('Ctrl Pts',(-0.739888619060256,0.280198162191953,
-3.95619009110614));
#48332=CARTESIAN_POINT('Ctrl Pts',(-0.693375462027023,0.403020365079478,
-3.96147592796479));
#48333=CARTESIAN_POINT('Ctrl Pts',(-0.615619780996831,0.514010925229607,
-3.96676176482343));
#48334=CARTESIAN_POINT('Ctrl Pts',(-0.516072434305609,0.59967943208061,
-3.97204760168208));
#48335=CARTESIAN_POINT('Ctrl Pts',(-0.416525087614387,0.685347938931613,
-3.97733343854073));
#48336=CARTESIAN_POINT('Ctrl Pts',(-0.295186075262136,0.745694392483489,
-3.98261927539938));
#48337=CARTESIAN_POINT('Ctrl Pts',(-0.166803616300752,0.773383948824665,
-3.98790511225803));
#48338=CARTESIAN_POINT('Ctrl Pts',(-0.0384211573393675,0.801073505165841,
-3.99319094911668));
#48339=CARTESIAN_POINT('Ctrl Pts',(0.0970047482311494,0.796106164296317,
-3.99847678597532));
#48340=CARTESIAN_POINT('Ctrl Pts',(0.223013681935846,0.759085684478411,
-4.00376262283397));
#48341=CARTESIAN_POINT('Ctrl Pts',(0.349022615640543,0.722065204660505,
-4.00904845969262));
#48342=CARTESIAN_POINT('Ctrl Pts',(0.46561457747942,0.652991585894218,-4.01433429655127));
#48343=CARTESIAN_POINT('Ctrl Pts',(0.558618331346661,0.560260420335145,
-4.01962013340991));
#48344=CARTESIAN_POINT('Ctrl Pts',(0.6516220852139,0.467529254776075,-4.02490597026856));
#48345=CARTESIAN_POINT('Ctrl Pts',(0.721037631109505,0.351140542424221,
-4.03019180712721));
#48346=CARTESIAN_POINT('Ctrl Pts',(0.758427817151085,0.225240815311261,
-4.03547764398585));
#48347=CARTESIAN_POINT('Ctrl Pts',(0.795818003192665,0.0993410881982974,
-4.0407634808445));
#48348=CARTESIAN_POINT('Ctrl Pts',(0.801182829380219,-0.036069653675772,
-4.04604931770315));
#48349=CARTESIAN_POINT('Ctrl Pts',(0.773870224873085,-0.164532834916077,
-4.0513351545618));
#48350=CARTESIAN_POINT('Ctrl Pts',(0.746557620365952,-0.292996016156382,
-4.05662099142045));
#48351=CARTESIAN_POINT('Ctrl Pts',(0.686567585164131,-0.414511636762924,
-4.0619068282791));
#48352=CARTESIAN_POINT('Ctrl Pts',(0.601191642108759,-0.514310011733404,
-4.06719266513774));
#48353=CARTESIAN_POINT('Ctrl Pts',(0.515815699053388,-0.614108386703885,
-4.07247850199639));
#48354=CARTESIAN_POINT('Ctrl Pts',(0.405053848144467,-0.692189516038305,
-4.07776433885504));
#48355=CARTESIAN_POINT('Ctrl Pts',(0.282368701349333,-0.739062984602079,
-4.08305017571368));
#48356=CARTESIAN_POINT('Ctrl Pts',(0.159683554554199,-0.785936453165852,
-4.08833601257233));
#48357=CARTESIAN_POINT('Ctrl Pts',(0.0250751118728523,-0.801602260958979,
-4.09362184943098));
#48358=CARTESIAN_POINT('Ctrl Pts',(-0.105095567210095,-0.784156298491206,
-4.09890768628963));
#48359=CARTESIAN_POINT('Ctrl Pts',(-0.235266246293042,-0.766710336023433,
-4.10419352314828));
#48360=CARTESIAN_POINT('Ctrl Pts',(-0.360999161777591,-0.716152603294759,
-4.10947936000693));
#48361=CARTESIAN_POINT('Ctrl Pts',(-0.467012035164418,-0.638628168594394,
-4.11476519686557));
#48362=CARTESIAN_POINT('Ctrl Pts',(-0.573024908551245,-0.561103733894028,
-4.12005103372422));
#48363=CARTESIAN_POINT('Ctrl Pts',(-0.659317739840351,-0.456612597221972,
-4.12533687058287));
#48364=CARTESIAN_POINT('Ctrl Pts',(-0.715402017927282,-0.337855193028336,
-4.13062270744152));
#48365=CARTESIAN_POINT('Ctrl Pts',(-0.76507283774313,-0.23267816611971,
-4.13530408801978));
#48366=CARTESIAN_POINT('Ctrl Pts',(-0.791049006691502,-0.116311122071119,
-4.13998546859804));
#48367=CARTESIAN_POINT('Ctrl Pts',(-0.79114572203675,1.41578566767164E-5,
-4.1446668491763));
#48368=CARTESIAN_POINT('Ctrl Pts',(-0.791131276639148,1.74428956908455E-5,
-4.1731331508237));
#48369=CARTESIAN_POINT('Ctrl Pts',(-0.791024410825469,-0.111096422019725,
-4.16866173391643));
#48370=CARTESIAN_POINT('Ctrl Pts',(-0.767393123498328,-0.222254302430152,
-4.16419031700916));
#48371=CARTESIAN_POINT('Ctrl Pts',(-0.721947197732644,-0.323633156993923,
-4.15971890010188));
#48372=CARTESIAN_POINT('Ctrl Pts',(-0.668223790931328,-0.443477067157891,
-4.15443306324324));
#48373=CARTESIAN_POINT('Ctrl Pts',(-0.584015454278886,-0.549655249247222,
-4.14914722638459));
#48374=CARTESIAN_POINT('Ctrl Pts',(-0.479557337797311,-0.629262215920062,
-4.14386138952594));
#48375=CARTESIAN_POINT('Ctrl Pts',(-0.375099221315737,-0.7088691825929,
-4.13857555266729));
#48376=CARTESIAN_POINT('Ctrl Pts',(-0.250391325005029,-0.761904933849247,
-4.13328971580864));
#48377=CARTESIAN_POINT('Ctrl Pts',(-0.120591340827875,-0.781923209232982,
-4.12800387895));
#48378=CARTESIAN_POINT('Ctrl Pts',(0.0092086433492808,-0.801941484616718,
-4.12271804209135));
#48379=CARTESIAN_POINT('Ctrl Pts',(0.144100715392882,-0.788942284127844,
-4.1174322052327));
#48380=CARTESIAN_POINT('Ctrl Pts',(0.26768934192668,-0.744505602959932,
-4.11214636837406));
#48381=CARTESIAN_POINT('Ctrl Pts',(0.391277968460475,-0.700068921792021,
-4.10686053151541));
#48382=CARTESIAN_POINT('Ctrl Pts',(0.503563149484464,-0.624194759945072,
-4.10157469465676));
#48383=CARTESIAN_POINT('Ctrl Pts',(0.590897119008789,-0.526105285439125,
-4.09628885779811));
#48384=CARTESIAN_POINT('Ctrl Pts',(0.678231088533113,-0.42801581093318,
-4.09100302093946));
#48385=CARTESIAN_POINT('Ctrl Pts',(0.740613846557776,-0.307711023768233,
-4.08571718408082));
#48386=CARTESIAN_POINT('Ctrl Pts',(0.770463045389535,-0.179813437509422,
-4.08043134722217));
#48387=CARTESIAN_POINT('Ctrl Pts',(0.800312244221295,-0.0519158512506065,
-4.07514551036352));
#48388=CARTESIAN_POINT('Ctrl Pts',(0.79762788386015,0.0835745341020731,
-4.06985967350487));
#48389=CARTESIAN_POINT('Ctrl Pts',(0.762736236408148,0.21018946284199,-4.06457383664622));
#48390=CARTESIAN_POINT('Ctrl Pts',(0.727844588956147,0.336804391581905,
-4.05928799978757));
#48391=CARTESIAN_POINT('Ctrl Pts',(0.660745654413287,0.454543863709056,
-4.05400216292893));
#48392=CARTESIAN_POINT('Ctrl Pts',(0.569595010821645,0.549097168329032,
-4.04871632607028));
#48393=CARTESIAN_POINT('Ctrl Pts',(0.478444367230003,0.643650472949008,
-4.04343048921163));
#48394=CARTESIAN_POINT('Ctrl Pts',(0.363242014589576,0.715017610061812,
-4.03814465235298));
#48395=CARTESIAN_POINT('Ctrl Pts',(0.23799028816829,0.754524220524063,-4.03285881549434));
#48396=CARTESIAN_POINT('Ctrl Pts',(0.112738561747003,0.794030830986314,
-4.02757297863569));
#48397=CARTESIAN_POINT('Ctrl Pts',(-0.0225625384551408,0.801676914798013,
-4.02228714177704));
#48398=CARTESIAN_POINT('Ctrl Pts',(-0.151467763502455,0.776533124367168,
-4.01700130491839));
#48399=CARTESIAN_POINT('Ctrl Pts',(-0.280372988549768,0.751389333936323,
-4.01171546805975));
#48400=CARTESIAN_POINT('Ctrl Pts',(-0.40288233844225,0.693455669262934,
-4.0064296312011));
#48401=CARTESIAN_POINT('Ctrl Pts',(-0.504105344788126,0.609773710466362,
-4.00114379434245));
#48402=CARTESIAN_POINT('Ctrl Pts',(-0.605328351134004,0.526091751669789,
-3.9958579574838));
#48403=CARTESIAN_POINT('Ctrl Pts',(-0.685265013933277,0.416661498750035,
-3.99057212062515));
#48404=CARTESIAN_POINT('Ctrl Pts',(-0.734199386184346,0.294783713841862,
-3.98528628376651));
#48405=CARTESIAN_POINT('Ctrl Pts',(-0.771702494165381,0.201377064943841,
-3.98123523945224));
#48406=CARTESIAN_POINT('Ctrl Pts',(-0.790996008268795,0.100659198123538,
-3.97718419513797));
#48407=CARTESIAN_POINT('Ctrl Pts',(-0.791098791730102,-2.0404891719479E-5,
-3.9731331508237));
#48408=CARTESIAN_POINT('Origin',(0.,0.,-2.94));
#48409=CARTESIAN_POINT('',(-0.791059421552401,1.68056895702706E-5,-3.7446668491763));
#48410=CARTESIAN_POINT('',(-0.791048214887112,1.35633341352688E-5,-3.7731331508237));
#48411=CARTESIAN_POINT('',(-0.7911,-9.68818082805471E-17,-2.94));
#48412=CARTESIAN_POINT('Ctrl Pts',(-0.791059421552401,1.68056895702706E-5,
-3.7446668491763));
#48413=CARTESIAN_POINT('Ctrl Pts',(-0.791093925544372,0.0445560275500737,
-3.74645871732382));
#48414=CARTESIAN_POINT('Ctrl Pts',(-0.787395328553636,0.0890895801141432,
-3.74825058547135));
#48415=CARTESIAN_POINT('Ctrl Pts',(-0.77991221789656,0.132977859383846,
-3.75004245361888));
#48416=CARTESIAN_POINT('Ctrl Pts',(-0.757837768845652,0.262444017117988,
-3.75532829047752));
#48417=CARTESIAN_POINT('Ctrl Pts',(-0.702830760007432,0.386295054067948,
-3.76061412733617));
#48418=CARTESIAN_POINT('Ctrl Pts',(-0.621577049458446,0.489477425727861,
-3.76589996419482));
#48419=CARTESIAN_POINT('Ctrl Pts',(-0.54032333890946,0.592659797387773,
-3.77118580105346));
#48420=CARTESIAN_POINT('Ctrl Pts',(-0.43282292664971,0.675173503757637,
-3.77647163791212));
#48421=CARTESIAN_POINT('Ctrl Pts',(-0.31214201123678,0.726989369613957,
-3.78175747477076));
#48422=CARTESIAN_POINT('Ctrl Pts',(-0.191461095823851,0.778805235470277,
-3.78704331162941));
#48423=CARTESIAN_POINT('Ctrl Pts',(-0.0575996772577453,0.799923260813052,
-3.79232914848806));
#48424=CARTESIAN_POINT('Ctrl Pts',(0.0731719824465547,0.787776643278716,
-3.7976149853467));
#48425=CARTESIAN_POINT('Ctrl Pts',(0.203943642150855,0.77563002574438,-3.80290082220535));
#48426=CARTESIAN_POINT('Ctrl Pts',(0.331625542993347,0.730218765332932,
-3.808186659064));
#48427=CARTESIAN_POINT('Ctrl Pts',(0.440698515944364,0.657062399437889,
-3.81347249592265));
#48428=CARTESIAN_POINT('Ctrl Pts',(0.549771488895381,0.583906033542846,
-3.8187583327813));
#48429=CARTESIAN_POINT('Ctrl Pts',(0.640235533954922,0.483004562164209,
-3.82404416963994));
#48430=CARTESIAN_POINT('Ctrl Pts',(0.701095147475853,0.36662211184877,-3.82933000649859));
#48431=CARTESIAN_POINT('Ctrl Pts',(0.761954760996783,0.250239661533333,
-3.83461584335724));
#48432=CARTESIAN_POINT('Ctrl Pts',(0.793209942979106,0.11837623228109,-3.83990168021589));
#48433=CARTESIAN_POINT('Ctrl Pts',(0.791061764608035,-0.0129407606369183,
-3.84518751707453));
#48434=CARTESIAN_POINT('Ctrl Pts',(0.788913586236965,-0.144257753554929,
-3.85047335393318));
#48435=CARTESIAN_POINT('Ctrl Pts',(0.753362047512502,-0.275028310138708,
-3.85575919079183));
#48436=CARTESIAN_POINT('Ctrl Pts',(0.688728280365558,-0.38935784894534,
-3.86104502765048));
#48437=CARTESIAN_POINT('Ctrl Pts',(0.624094513218613,-0.503687387751972,
-3.86633086450913));
#48438=CARTESIAN_POINT('Ctrl Pts',(0.530378517649187,-0.601575908781457,
-3.87161670136777));
#48439=CARTESIAN_POINT('Ctrl Pts',(0.418971057472893,-0.671125496245439,
-3.87690253822642));
#48440=CARTESIAN_POINT('Ctrl Pts',(0.307563597296602,-0.74067508370942,
-3.88218837508507));
#48441=CARTESIAN_POINT('Ctrl Pts',(0.178464672513446,-0.781885737607901,
-3.88747421194372));
#48442=CARTESIAN_POINT('Ctrl Pts',(0.0473656851313694,-0.789748485647599,
-3.89276004880236));
#48443=CARTESIAN_POINT('Ctrl Pts',(-0.0837333022507111,-0.797611233687299,
-3.89804588566101));
#48444=CARTESIAN_POINT('Ctrl Pts',(-0.216832352231711,-0.772126075868214,
-3.90333172251966));
#48445=CARTESIAN_POINT('Ctrl Pts',(-0.335753865318564,-0.716390620146778,
-3.90861755937831));
#48446=CARTESIAN_POINT('Ctrl Pts',(-0.454675378405417,-0.660655164425341,
-3.91390339623696));
#48447=CARTESIAN_POINT('Ctrl Pts',(-0.559419354598121,-0.574669410801554,
-3.91918923309561));
#48448=CARTESIAN_POINT('Ctrl Pts',(-0.637254627923676,-0.468884546450935,
-3.92447506995425));
#48449=CARTESIAN_POINT('Ctrl Pts',(-0.71508990124923,-0.363099682100315,
-3.9297609068129));
#48450=CARTESIAN_POINT('Ctrl Pts',(-0.766016471707633,-0.237515707022865,
-3.93504674367155));
#48451=CARTESIAN_POINT('Ctrl Pts',(-0.783844440418698,-0.107396796671679,
-3.94033258053019));
#48452=CARTESIAN_POINT('Ctrl Pts',(-0.788717286344795,-0.0718319259626912,
-3.94177733674556));
#48453=CARTESIAN_POINT('Ctrl Pts',(-0.791117433116371,-0.0359282635819957,
-3.94322209296093));
#48454=CARTESIAN_POINT('Ctrl Pts',(-0.791082780681432,-2.0004826913167E-5,
-3.9446668491763));
#48455=CARTESIAN_POINT('Ctrl Pts',(-0.791098791730102,-2.0404891719479E-5,
-3.9731331508237));
#48456=CARTESIAN_POINT('Ctrl Pts',(-0.791130120997783,-0.0307083987841548,
-3.97189835827932));
#48457=CARTESIAN_POINT('Ctrl Pts',(-0.789378474176348,-0.0613928376556407,
-3.97066356573494));
#48458=CARTESIAN_POINT('Ctrl Pts',(-0.785816066255412,-0.0918655900473206,
-3.96942877319056));
#48459=CARTESIAN_POINT('Ctrl Pts',(-0.770566292372547,-0.222311792131744,
-3.96414293633192));
#48460=CARTESIAN_POINT('Ctrl Pts',(-0.722134662903953,-0.348878879404003,
-3.95885709947327));
#48461=CARTESIAN_POINT('Ctrl Pts',(-0.64640782771266,-0.456183183481889,
-3.95357126261462));
#48462=CARTESIAN_POINT('Ctrl Pts',(-0.570680992521369,-0.563487487559772,
-3.94828542575597));
#48463=CARTESIAN_POINT('Ctrl Pts',(-0.467658951607378,-0.651529008443283,
-3.94299958889732));
#48464=CARTESIAN_POINT('Ctrl Pts',(-0.349863577343953,-0.709606689559761,
-3.93771375203868));
#48465=CARTESIAN_POINT('Ctrl Pts',(-0.232068203080525,-0.767684370676241,
-3.93242791518003));
#48466=CARTESIAN_POINT('Ctrl Pts',(-0.0994994954676606,-0.795798212025687,
-3.92714207832138));
#48467=CARTESIAN_POINT('Ctrl Pts',(0.0317294067653929,-0.790531100821585,
-3.92185624146273));
#48468=CARTESIAN_POINT('Ctrl Pts',(0.162958308998446,-0.785263989617483,
-3.91657040460409));
#48469=CARTESIAN_POINT('Ctrl Pts',(0.292847405851691,-0.746615925859833,
-3.91128456774544));
#48470=CARTESIAN_POINT('Ctrl Pts',(0.405609253404915,-0.679284410370338,
-3.90599873088679));
#48471=CARTESIAN_POINT('Ctrl Pts',(0.518371100958137,-0.611952894880846,
-3.90071289402814));
#48472=CARTESIAN_POINT('Ctrl Pts',(0.614005699211341,-0.515937927659511,
-3.89542705716949));
#48473=CARTESIAN_POINT('Ctrl Pts',(0.680889086697923,-0.402909702334828,
-3.89014122031085));
#48474=CARTESIAN_POINT('Ctrl Pts',(0.747772474184507,-0.289881477010141,
-3.8848553834522));
#48475=CARTESIAN_POINT('Ctrl Pts',(0.785904650904467,-0.159839993582104,
-3.87956954659355));
#48476=CARTESIAN_POINT('Ctrl Pts',(0.790650819818588,-0.0285912178835576,
-3.8742837097349));
#48477=CARTESIAN_POINT('Ctrl Pts',(0.795396988732709,0.102657557814991,
-3.86899787287626));
#48478=CARTESIAN_POINT('Ctrl Pts',(0.766757149840992,0.235113625784043,
-3.86371203601761));
#48479=CARTESIAN_POINT('Ctrl Pts',(0.708212348599448,0.352677538143735,
-3.85842619915896));
#48480=CARTESIAN_POINT('Ctrl Pts',(0.649667547357904,0.470241450503425,
-3.85314036230031));
#48481=CARTESIAN_POINT('Ctrl Pts',(0.561217783766536,0.572913207253749,
-3.84785452544167));
#48482=CARTESIAN_POINT('Ctrl Pts',(0.453613734489391,0.648213511508715,
-3.84256868858302));
#48483=CARTESIAN_POINT('Ctrl Pts',(0.346009685212246,0.723513815763681,
-3.83728285172437));
#48484=CARTESIAN_POINT('Ctrl Pts',(0.219251350249323,0.771442667523289,
-3.83199701486572));
#48485=CARTESIAN_POINT('Ctrl Pts',(0.0887456432918277,0.786174527326211,
-3.82671117800707));
#48486=CARTESIAN_POINT('Ctrl Pts',(-0.041760063665668,0.800906387129132,
-3.82142534114842));
#48487=CARTESIAN_POINT('Ctrl Pts',(-0.176013142617738,0.782441254975367,
-3.81613950428978));
#48488=CARTESIAN_POINT('Ctrl Pts',(-0.297695726965726,0.733023485821715,
-3.81085366743113));
#48489=CARTESIAN_POINT('Ctrl Pts',(-0.419378311313713,0.683605716668064,
-3.80556783057248));
#48490=CARTESIAN_POINT('Ctrl Pts',(-0.528490401057619,0.603235310514526,
-3.80028199371383));
#48491=CARTESIAN_POINT('Ctrl Pts',(-0.611769905386271,0.501680933944618,
-3.79499615685519));
#48492=CARTESIAN_POINT('Ctrl Pts',(-0.695049409714923,0.40012655737471,
-3.78971031999654));
#48493=CARTESIAN_POINT('Ctrl Pts',(-0.752496328628322,0.277388210388431,
-3.78442448313789));
#48494=CARTESIAN_POINT('Ctrl Pts',(-0.777128243796476,0.148384194959152,
-3.77913864627924));
#48495=CARTESIAN_POINT('Ctrl Pts',(-0.786456748033961,0.0995282900744009,
-3.77713681446073));
#48496=CARTESIAN_POINT('Ctrl Pts',(-0.791078729935658,0.0497737258841513,
-3.77513498264221));
#48497=CARTESIAN_POINT('Ctrl Pts',(-0.791048214887112,1.35633341352688E-5,
-3.7731331508237));
#48498=CARTESIAN_POINT('Origin',(0.,0.,-2.94));
#48499=CARTESIAN_POINT('',(-0.791163048520337,-6.61538243201809E-6,-3.54466684917629));
#48500=CARTESIAN_POINT('',(-0.791167436263867,-1.24420514395741E-6,-3.5731331508237));
#48501=CARTESIAN_POINT('',(-0.7911,-9.68818082805471E-17,-2.94));
#48502=CARTESIAN_POINT('Ctrl Pts',(-0.791163048520337,-6.61538243201809E-6,
-3.54466684917629));
#48503=CARTESIAN_POINT('Ctrl Pts',(-0.791107674076706,0.124935935430854,
-3.54969534168672));
#48504=CARTESIAN_POINT('Ctrl Pts',(-0.760988940033902,0.249904240112934,
-3.55472383419714));
#48505=CARTESIAN_POINT('Ctrl Pts',(-0.703968423943417,0.361074281556113,
-3.55975232670756));
#48506=CARTESIAN_POINT('Ctrl Pts',(-0.644029755440748,0.477933698452947,
-3.5650381635662));
#48507=CARTESIAN_POINT('Ctrl Pts',(-0.554365328477183,0.579546398998705,
-3.57032400042485));
#48508=CARTESIAN_POINT('Ctrl Pts',(-0.44587345666502,0.653561809894234,
-3.5756098372835));
#48509=CARTESIAN_POINT('Ctrl Pts',(-0.337381584852852,0.727577220789767,
-3.58089567414214));
#48510=CARTESIAN_POINT('Ctrl Pts',(-0.210062268192083,0.773995342035067,
-3.58618151100079));
#48511=CARTESIAN_POINT('Ctrl Pts',(-0.0793906052124412,0.787174256765707,
-3.59146734785944));
#48512=CARTESIAN_POINT('Ctrl Pts',(0.0512810577672008,0.800353171496347,
-3.59675318471809));
#48513=CARTESIAN_POINT('Ctrl Pts',(0.185305067065716,0.780292879712326,
-3.60203902157673));
#48514=CARTESIAN_POINT('Ctrl Pts',(0.306391398485365,0.72943162095211,-3.60732485843538));
#48515=CARTESIAN_POINT('Ctrl Pts',(0.427477729905014,0.678570362191895,
-3.61261069529403));
#48516=CARTESIAN_POINT('Ctrl Pts',(0.535626383445797,0.596908136455485,
-3.61789653215268));
#48517=CARTESIAN_POINT('Ctrl Pts',(0.61769236969609,0.49437062527002,-3.62318236901133));
#48518=CARTESIAN_POINT('Ctrl Pts',(0.699758355946382,0.391833114084555,
-3.62846820586998));
#48519=CARTESIAN_POINT('Ctrl Pts',(0.755741674906185,0.268420317450034,
-3.63375404272862));
#48520=CARTESIAN_POINT('Ctrl Pts',(0.778837802331684,0.139132513704717,
-3.63903987958727));
#48521=CARTESIAN_POINT('Ctrl Pts',(0.801933929757183,0.00984470995939934,
-3.64432571644592));
#48522=CARTESIAN_POINT('Ctrl Pts',(0.792142865648378,-0.125318100896716,
-3.64961155330457));
#48523=CARTESIAN_POINT('Ctrl Pts',(0.75065467044361,-0.249927478384903,
-3.65489739016321));
#48524=CARTESIAN_POINT('Ctrl Pts',(0.709166475238842,-0.374536855873091,
-3.66018322702186));
#48525=CARTESIAN_POINT('Ctrl Pts',(0.635981148938111,-0.488592799993352,
-3.66546906388051));
#48526=CARTESIAN_POINT('Ctrl Pts',(0.539994043520502,-0.578232316351325,
-3.67075490073916));
#48527=CARTESIAN_POINT('Ctrl Pts',(0.444006938102892,-0.667871832709299,
-3.67604073759781));
#48528=CARTESIAN_POINT('Ctrl Pts',(0.325218053568405,-0.733094921304985,
-3.68132657445645));
#48529=CARTESIAN_POINT('Ctrl Pts',(0.19806565223748,-0.765974004855506,
-3.6866124113151));
#48530=CARTESIAN_POINT('Ctrl Pts',(0.0709132509065556,-0.798853088406027,
-3.69189824817375));
#48531=CARTESIAN_POINT('Ctrl Pts',(-0.0646026672208058,-0.799388166911383,
-3.69718408503239));
#48532=CARTESIAN_POINT('Ctrl Pts',(-0.192010743042395,-0.767514203951268,
-3.70246992189104));
#48533=CARTESIAN_POINT('Ctrl Pts',(-0.31941881886398,-0.735640240991153,
-3.70775575874969));
#48534=CARTESIAN_POINT('Ctrl Pts',(-0.438719052379794,-0.671357236565569,
-3.71304159560834));
#48535=CARTESIAN_POINT('Ctrl Pts',(-0.535411029067541,-0.582478504893938,
-3.71832743246699));
#48536=CARTESIAN_POINT('Ctrl Pts',(-0.632103005755294,-0.493599773222301,
-3.72361326932564));
#48537=CARTESIAN_POINT('Ctrl Pts',(-0.706186725614977,-0.380125314304615,
-3.72889910618428));
#48538=CARTESIAN_POINT('Ctrl Pts',(-0.74865764091302,-0.255847445586608,
-3.73418494304293));
#48539=CARTESIAN_POINT('Ctrl Pts',(-0.776731161370101,-0.173699056145654,
-3.73767891175405));
#48540=CARTESIAN_POINT('Ctrl Pts',(-0.79099214212198,-0.086830347552772,
-3.74117288046517));
#48541=CARTESIAN_POINT('Ctrl Pts',(-0.791059421552401,1.68056895702706E-5,
-3.7446668491763));
#48542=CARTESIAN_POINT('Ctrl Pts',(-0.791048214887112,1.35633341352688E-5,
-3.7731331508237));
#48543=CARTESIAN_POINT('Ctrl Pts',(-0.790998154950857,-0.0816179818839992,
-3.76984914578357));
#48544=CARTESIAN_POINT('Ctrl Pts',(-0.778427108402436,-0.163264593632743,
-3.76656514074343));
#48545=CARTESIAN_POINT('Ctrl Pts',(-0.753573596205868,-0.240983426237628,
-3.7632811357033));
#48546=CARTESIAN_POINT('Ctrl Pts',(-0.713570122024198,-0.366077348132835,
-3.75799529884465));
#48547=CARTESIAN_POINT('Ctrl Pts',(-0.641746262237952,-0.480995508050975,
-3.752709461986));
#48548=CARTESIAN_POINT('Ctrl Pts',(-0.5468318886068,-0.571770113089685,
-3.74742362512736));
#48549=CARTESIAN_POINT('Ctrl Pts',(-0.451917514975644,-0.662544718128397,
-3.74213778826871));
#48550=CARTESIAN_POINT('Ctrl Pts',(-0.333912627499583,-0.729175768287678,
-3.73685195141006));
#48551=CARTESIAN_POINT('Ctrl Pts',(-0.207160197132085,-0.76356455479813,
-3.73156611455141));
#48552=CARTESIAN_POINT('Ctrl Pts',(-0.0804077667645874,-0.797953341308583,
-3.72628027769276));
#48553=CARTESIAN_POINT('Ctrl Pts',(0.0550922064943439,-0.800099864170207,
-3.72099444083412));
#48554=CARTESIAN_POINT('Ctrl Pts',(0.182870301570576,-0.769743223044774,
-3.71570860397547));
#48555=CARTESIAN_POINT('Ctrl Pts',(0.310648396646807,-0.739386581919342,
-3.71042276711682));
#48556=CARTESIAN_POINT('Ctrl Pts',(0.430704613540337,-0.676526776806852,
-3.70513693025817));
#48557=CARTESIAN_POINT('Ctrl Pts',(0.528446651300607,-0.588804138359307,
-3.69985109339953));
#48558=CARTESIAN_POINT('Ctrl Pts',(0.626188689060877,-0.501081499911761,
-3.69456525654088));
#48559=CARTESIAN_POINT('Ctrl Pts',(0.701616547687885,-0.388496028129161,
-3.68927941968223));
#48560=CARTESIAN_POINT('Ctrl Pts',(0.745562305339503,-0.264731988011871,
-3.68399358282358));
#48561=CARTESIAN_POINT('Ctrl Pts',(0.78950806299112,-0.140967947894581,
-3.67870774596493));
#48562=CARTESIAN_POINT('Ctrl Pts',(0.801971719667347,-0.00602533944260349,
-3.67342190910629));
#48563=CARTESIAN_POINT('Ctrl Pts',(0.781438373150955,0.123694161491399,
-3.66813607224764));
#48564=CARTESIAN_POINT('Ctrl Pts',(0.760905026634563,0.253413662425401,
-3.66285023538899));
#48565=CARTESIAN_POINT('Ctrl Pts',(0.707374676925553,0.377910055841426,
-3.65756439853034));
#48566=CARTESIAN_POINT('Ctrl Pts',(0.627353700729391,0.482051357016042,
-3.65227856167169));
#48567=CARTESIAN_POINT('Ctrl Pts',(0.547332724533233,0.586192658190656,
-3.64699272481305));
#48568=CARTESIAN_POINT('Ctrl Pts',(0.440821121849916,0.669978867123868,
-3.6417068879544));
#48569=CARTESIAN_POINT('Ctrl Pts',(0.32076490581645,0.723226141546637,-3.63642105109575));
#48570=CARTESIAN_POINT('Ctrl Pts',(0.200708689782987,0.776473415969404,
-3.6311352142371));
#48571=CARTESIAN_POINT('Ctrl Pts',(0.067107860399371,0.799181755881737,
-3.62584937737845));
#48572=CARTESIAN_POINT('Ctrl Pts',(-0.063798993779351,0.788591063234052,
-3.62056354051981));
#48573=CARTESIAN_POINT('Ctrl Pts',(-0.19470584795808,0.778000370586367,
-3.61527770366116));
#48574=CARTESIAN_POINT('Ctrl Pts',(-0.322918726931912,0.73411064537866,
-3.60999186680251));
#48575=CARTESIAN_POINT('Ctrl Pts',(-0.432853923633158,0.662256489145445,
-3.60470602994387));
#48576=CARTESIAN_POINT('Ctrl Pts',(-0.542789120334404,0.59040233291223,
-3.59942019308522));
#48577=CARTESIAN_POINT('Ctrl Pts',(-0.634446634763061,0.490583745653509,
-3.59413435622657));
#48578=CARTESIAN_POINT('Ctrl Pts',(-0.696685902360868,0.374933234151754,
-3.58884851936792));
#48579=CARTESIAN_POINT('Ctrl Pts',(-0.75836727558384,0.26031937960796,-3.58361006318651));
#48580=CARTESIAN_POINT('Ctrl Pts',(-0.791155431195283,0.130156154124652,
-3.57837160700511));
#48581=CARTESIAN_POINT('Ctrl Pts',(-0.791167436263867,-1.24420514395741E-6,
-3.5731331508237));
#48582=CARTESIAN_POINT('Origin',(0.,0.,-2.94));
#48583=CARTESIAN_POINT('',(-0.791037041324519,-7.57978170876084E-6,-3.3446668491763));
#48584=CARTESIAN_POINT('',(-0.791044053170824,-1.18405052558484E-5,-3.3731331508237));
#48585=CARTESIAN_POINT('',(-0.7911,-9.68818082805471E-17,-2.94));
#48586=CARTESIAN_POINT('Ctrl Pts',(-0.791037041324519,-7.57978170876084E-6,
-3.3446668491763));
#48587=CARTESIAN_POINT('Ctrl Pts',(-0.791012114368536,0.0740523149147727,
-3.34764612919096));
#48588=CARTESIAN_POINT('Ctrl Pts',(-0.780696222431574,0.148119012240718,
-3.35062540920562));
#48589=CARTESIAN_POINT('Ctrl Pts',(-0.760182848009542,0.219244649427855,
-3.35360468922029));
#48590=CARTESIAN_POINT('Ctrl Pts',(-0.723788031113677,0.345435713305053,
-3.35889052607894));
#48591=CARTESIAN_POINT('Ctrl Pts',(-0.655293746461191,0.46236895641775,
-3.36417636293758));
#48592=CARTESIAN_POINT('Ctrl Pts',(-0.563025170714357,0.555831661434206,
-3.36946219979623));
#48593=CARTESIAN_POINT('Ctrl Pts',(-0.470756594967522,0.649294366450663,
-3.37474803665488));
#48594=CARTESIAN_POINT('Ctrl Pts',(-0.354713728126337,0.71928653337088,
-3.38003387351353));
#48595=CARTESIAN_POINT('Ctrl Pts',(-0.229001066233802,0.757300924583103,
-3.38531971037218));
#48596=CARTESIAN_POINT('Ctrl Pts',(-0.103288404341268,0.795315315795325,
-3.39060554723082));
#48597=CARTESIAN_POINT('Ctrl Pts',(0.0320940526026171,0.801351931299553,
-3.39589138408947));
#48598=CARTESIAN_POINT('Ctrl Pts',(0.160691167110856,0.774677047241747,
-3.40117722094812));
#48599=CARTESIAN_POINT('Ctrl Pts',(0.289288281619095,0.748002163183941,
-3.40646305780677));
#48600=CARTESIAN_POINT('Ctrl Pts',(0.41110005369169,0.6886157795641,-3.41174889466542));
#48601=CARTESIAN_POINT('Ctrl Pts',(0.511320802428493,0.603736048049579,
-3.41703473152406));
#48602=CARTESIAN_POINT('Ctrl Pts',(0.611541551165295,0.518856316535058,
-3.42232056838271));
#48603=CARTESIAN_POINT('Ctrl Pts',(0.690171276566308,0.408483237125855,
-3.42760640524136));
#48604=CARTESIAN_POINT('Ctrl Pts',(0.73765288407699,0.286032168336954,-3.43289224210001));
#48605=CARTESIAN_POINT('Ctrl Pts',(0.785134491587671,0.163581099548057,
-3.43817807895865));
#48606=CARTESIAN_POINT('Ctrl Pts',(0.801467981208026,0.0290520413794619,
-3.4434639158173));
#48607=CARTESIAN_POINT('Ctrl Pts',(0.784668089681554,-0.101203595519831,
-3.44874975267595));
#48608=CARTESIAN_POINT('Ctrl Pts',(0.767868198155081,-0.231459232419131,
-3.4540355895346));
#48609=CARTESIAN_POINT('Ctrl Pts',(0.717934925481783,-0.357441448049119,
-3.45932142639325));
#48610=CARTESIAN_POINT('Ctrl Pts',(0.64093743959938,-0.463837662582968,
-3.46460726325189));
#48611=CARTESIAN_POINT('Ctrl Pts',(0.56393995371698,-0.570233877116814,
-3.46989310011054));
#48612=CARTESIAN_POINT('Ctrl Pts',(0.45987825462548,-0.657044090554512,
-3.47517893696919));
#48613=CARTESIAN_POINT('Ctrl Pts',(0.341400580540787,-0.713716906285016,
-3.48046477382784));
#48614=CARTESIAN_POINT('Ctrl Pts',(0.222922906456093,-0.770389722015521,
-3.48575061068648));
#48615=CARTESIAN_POINT('Ctrl Pts',(0.0900292573782051,-0.796925140038832,
-3.49103644754513));
#48616=CARTESIAN_POINT('Ctrl Pts',(-0.0411277327690323,-0.790097897926529,
-3.49632228440378));
#48617=CARTESIAN_POINT('Ctrl Pts',(-0.17228472291627,-0.783270655814226,
-3.50160812126243));
#48618=CARTESIAN_POINT('Ctrl Pts',(-0.301705054132859,-0.743080753566308,
-3.50689395812107));
#48619=CARTESIAN_POINT('Ctrl Pts',(-0.413658258883671,-0.674413095637956,
-3.51217979497972));
#48620=CARTESIAN_POINT('Ctrl Pts',(-0.525611463634484,-0.605745437709604,
-3.51746563183837));
#48621=CARTESIAN_POINT('Ctrl Pts',(-0.620097541919521,-0.508600024100816,
-3.52275146869702));
#48622=CARTESIAN_POINT('Ctrl Pts',(-0.685632129782885,-0.39478444918718,
-3.52803730555567));
#48623=CARTESIAN_POINT('Ctrl Pts',(-0.751166717646251,-0.28096887427354,
-3.53332314241432));
#48624=CARTESIAN_POINT('Ctrl Pts',(-0.787749815087943,-0.15048313805505,
-3.53860897927296));
#48625=CARTESIAN_POINT('Ctrl Pts',(-0.790934908787902,-0.0191872033218446,
-3.54389481613161));
#48626=CARTESIAN_POINT('Ctrl Pts',(-0.791089977111837,-0.0127949767638775,
-3.54415216047984));
#48627=CARTESIAN_POINT('Ctrl Pts',(-0.791165882431311,-0.00640082979925586,
-3.54440950482807));
#48628=CARTESIAN_POINT('Ctrl Pts',(-0.791163048520337,-6.61538243201809E-6,
-3.54466684917629));
#48629=CARTESIAN_POINT('Ctrl Pts',(-0.791167436263867,-1.24420514395741E-6,
-3.5731331508237));
#48630=CARTESIAN_POINT('Ctrl Pts',(-0.791167544847056,-0.00117848907790079,
-3.57308577014646));
#48631=CARTESIAN_POINT('Ctrl Pts',(-0.79116497207817,-0.0023557334739497,
-3.57303838946922));
#48632=CARTESIAN_POINT('Ctrl Pts',(-0.791159715084089,-0.00353296588344793,
-3.57299100879198));
#48633=CARTESIAN_POINT('Ctrl Pts',(-0.790573239442549,-0.13486621867211,
-3.56770517193333));
#48634=CARTESIAN_POINT('Ctrl Pts',(-0.756579267392514,-0.266050288504648,
-3.56241933507468));
#48635=CARTESIAN_POINT('Ctrl Pts',(-0.693309615540358,-0.381140333235874,
-3.55713349821603));
#48636=CARTESIAN_POINT('Ctrl Pts',(-0.630039963688201,-0.496230377967099,
-3.55184766135739));
#48637=CARTESIAN_POINT('Ctrl Pts',(-0.537494632033922,-0.595226397597014,
-3.54656182449874));
#48638=CARTESIAN_POINT('Ctrl Pts',(-0.426922095383839,-0.666095864791955,
-3.54127598764009));
#48639=CARTESIAN_POINT('Ctrl Pts',(-0.316349558733757,-0.736965331986896,
-3.53599015078144));
#48640=CARTESIAN_POINT('Ctrl Pts',(-0.18774981708787,-0.779708246746866,
-3.53070431392279));
#48641=CARTESIAN_POINT('Ctrl Pts',(-0.0567535989566851,-0.789129397263424,
-3.52541847706415));
#48642=CARTESIAN_POINT('Ctrl Pts',(0.0742426191744998,-0.798550547779982,
-3.5201326402055));
#48643=CARTESIAN_POINT('Ctrl Pts',(0.207635313790985,-0.77464993405313,
-3.51484680334685));
#48644=CARTESIAN_POINT('Ctrl Pts',(0.327211194195991,-0.720332569729222,
-3.50956096648821));
#48645=CARTESIAN_POINT('Ctrl Pts',(0.446787074600998,-0.666015205405313,
-3.50427512962956));
#48646=CARTESIAN_POINT('Ctrl Pts',(0.552546140794528,-0.581281090484348,
-3.49898929277091));
#48647=CARTESIAN_POINT('Ctrl Pts',(0.631633847113903,-0.476429281006071,
-3.49370345591226));
#48648=CARTESIAN_POINT('Ctrl Pts',(0.710721553433278,-0.371577471527794,
-3.48841761905361));
#48649=CARTESIAN_POINT('Ctrl Pts',(0.763137899878498,-0.246607967492202,
-3.48313178219496));
#48650=CARTESIAN_POINT('Ctrl Pts',(0.782511911902399,-0.116710258121227,
-3.47784594533632));
#48651=CARTESIAN_POINT('Ctrl Pts',(0.8018859239263,0.0131874512497518,-3.47256010847767));
#48652=CARTESIAN_POINT('Ctrl Pts',(0.788217601528883,0.148013365956107,
-3.46727427161902));
#48653=CARTESIAN_POINT('Ctrl Pts',(0.743168268705463,0.271379993752664,
-3.46198843476038));
#48654=CARTESIAN_POINT('Ctrl Pts',(0.698118935882044,0.394746621549218,
-3.45670259790173));
#48655=CARTESIAN_POINT('Ctrl Pts',(0.621688592632625,0.506653962435966,
-3.45141676104308));
#48656=CARTESIAN_POINT('Ctrl Pts',(0.523167008361145,0.593500175216756,
-3.44613092418443));
#48657=CARTESIAN_POINT('Ctrl Pts',(0.424645424089665,0.680346387997547,
-3.44084508732578));
#48658=CARTESIAN_POINT('Ctrl Pts',(0.304032598796122,0.74213147267238,-3.43555925046714));
#48659=CARTESIAN_POINT('Ctrl Pts',(0.17598848671464,0.771345726094183,-3.43027341360849));
#48660=CARTESIAN_POINT('Ctrl Pts',(0.0479443746331568,0.800559979515985,
-3.42498757674984));
#48661=CARTESIAN_POINT('Ctrl Pts',(-0.0875310242362685,0.797203401684758,
-3.41970173989119));
#48662=CARTESIAN_POINT('Ctrl Pts',(-0.213971275727604,0.761683969756075,
-3.41441590303254));
#48663=CARTESIAN_POINT('Ctrl Pts',(-0.34041152721894,0.726164537827391,
-3.40913006617389));
#48664=CARTESIAN_POINT('Ctrl Pts',(-0.457816631332189,0.658482251801251,
-3.40384422931525));
#48665=CARTESIAN_POINT('Ctrl Pts',(-0.551916518122767,0.566863593506508,
-3.3985583924566));
#48666=CARTESIAN_POINT('Ctrl Pts',(-0.646016404913346,0.475244935211765,
-3.39327255559795));
#48667=CARTESIAN_POINT('Ctrl Pts',(-0.716811074381257,0.359689904648418,
-3.38798671873931));
#48668=CARTESIAN_POINT('Ctrl Pts',(-0.755695748287589,0.234243703522489,
-3.38270088188066));
#48669=CARTESIAN_POINT('Ctrl Pts',(-0.779157066531176,0.158554930764511,
-3.37951163819501));
#48670=CARTESIAN_POINT('Ctrl Pts',(-0.791001902275285,0.0792653862822654,
-3.37632239450935));
#48671=CARTESIAN_POINT('Ctrl Pts',(-0.791044053170824,-1.18405052558484E-5,
-3.3731331508237));
#48672=CARTESIAN_POINT('Origin',(0.,0.,-2.94));
#48673=CARTESIAN_POINT('',(-0.791122594563005,1.8755956602709E-5,-3.1446668491763));
#48674=CARTESIAN_POINT('',(-0.791106220557104,2.01772645531753E-5,-3.1731331508237));
#48675=CARTESIAN_POINT('',(-0.7911,-9.68818082805471E-17,-2.94));
#48676=CARTESIAN_POINT('Ctrl Pts',(-0.791122594563005,1.8755956602709E-5,
-3.1446668491763));
#48677=CARTESIAN_POINT('Ctrl Pts',(-0.791145783735659,0.0231314904601002,
-3.1455969166952));
#48678=CARTESIAN_POINT('Ctrl Pts',(-0.790153058855057,0.046242239724187,
-3.14652698421411));
#48679=CARTESIAN_POINT('Ctrl Pts',(-0.788129997515042,0.0692624409588715,
-3.14745705173302));
#48680=CARTESIAN_POINT('Ctrl Pts',(-0.776632367524814,0.200092757796941,
-3.15274288859167));
#48681=CARTESIAN_POINT('Ctrl Pts',(-0.731855173927621,0.32799840000426,
-3.15802872545032));
#48682=CARTESIAN_POINT('Ctrl Pts',(-0.659240886106545,0.437433003780121,
-3.16331456230897));
#48683=CARTESIAN_POINT('Ctrl Pts',(-0.586626598285466,0.546867607555985,
-3.16860039916762));
#48684=CARTESIAN_POINT('Ctrl Pts',(-0.486175216240504,0.637831172900387,
-3.17388623602626));
#48685=CARTESIAN_POINT('Ctrl Pts',(-0.3700961601552,0.699267481689959,-3.17917207288491));
#48686=CARTESIAN_POINT('Ctrl Pts',(-0.2540171040699,0.76070379047953,-3.18445790974356));
#48687=CARTESIAN_POINT('Ctrl Pts',(-0.122310373944261,0.792612842714271,
-3.18974374660221));
#48688=CARTESIAN_POINT('Ctrl Pts',(0.00901566103487368,0.791116234548847,
-3.19502958346085));
#48689=CARTESIAN_POINT('Ctrl Pts',(0.140341696014012,0.789619626383422,
-3.2003154203195));
#48690=CARTESIAN_POINT('Ctrl Pts',(0.271287035846645,0.754717357817829,
-3.20560125717815));
#48691=CARTESIAN_POINT('Ctrl Pts',(0.385935854960777,0.690651644873401,
-3.2108870940368));
#48692=CARTESIAN_POINT('Ctrl Pts',(0.500584674074912,0.626585931928972,
-3.21617293089545));
#48693=CARTESIAN_POINT('Ctrl Pts',(0.598936972470544,0.533356774605708,
-3.22145876775409));
#48694=CARTESIAN_POINT('Ctrl Pts',(0.669038464276404,0.422295763688569,
-3.22674460461274));
#48695=CARTESIAN_POINT('Ctrl Pts',(0.739139956082262,0.311234752771435,
-3.23203044147139));
#48696=CARTESIAN_POINT('Ctrl Pts',(0.780990641298351,0.182341888260418,
-3.23731627833004));
#48697=CARTESIAN_POINT('Ctrl Pts',(0.789503754662005,0.051283526450878,
-3.24260211518869));
#48698=CARTESIAN_POINT('Ctrl Pts',(0.798016868025659,-0.0797748353586617,
-3.24788795204733));
#48699=CARTESIAN_POINT('Ctrl Pts',(0.773192409536883,-0.212998694466734,
-3.25317378890598));
#48700=CARTESIAN_POINT('Ctrl Pts',(0.71804768207741,-0.332195281384159,
-3.25845962576463));
#48701=CARTESIAN_POINT('Ctrl Pts',(0.662902954617938,-0.45139186830158,
-3.26374546262328));
#48702=CARTESIAN_POINT('Ctrl Pts',(0.577437958187772,-0.556561183028352,
-3.26903129948193));
#48703=CARTESIAN_POINT('Ctrl Pts',(0.472040584234078,-0.6349203615782,-3.27431713634057));
#48704=CARTESIAN_POINT('Ctrl Pts',(0.366643210280383,-0.713279540128047,
-3.27960297319922));
#48705=CARTESIAN_POINT('Ctrl Pts',(0.241313458803161,-0.764828582500967,
-3.28488881005787));
#48706=CARTESIAN_POINT('Ctrl Pts',(0.111284605503879,-0.783301931115,-3.29017464691652));
#48707=CARTESIAN_POINT('Ctrl Pts',(-0.0187442477954065,-0.801775279729033,
-3.29546048377516));
#48708=CARTESIAN_POINT('Ctrl Pts',(-0.153472202916751,-0.787172934584176,
-3.30074632063381));
#48709=CARTESIAN_POINT('Ctrl Pts',(-0.276523674168264,-0.741269746000149,
-3.30603215749246));
#48710=CARTESIAN_POINT('Ctrl Pts',(-0.399575145419777,-0.695366557416121,
-3.31131799435111));
#48711=CARTESIAN_POINT('Ctrl Pts',(-0.510950132801457,-0.618162525392924,
-3.31660383120975));
#48712=CARTESIAN_POINT('Ctrl Pts',(-0.597111500325757,-0.519041457775161,
-3.3218896680684));
#48713=CARTESIAN_POINT('Ctrl Pts',(-0.683272867850058,-0.419920390157398,
-3.32717550492705));
#48714=CARTESIAN_POINT('Ctrl Pts',(-0.744220615516977,-0.298882286945071,
-3.3324613417857));
#48715=CARTESIAN_POINT('Ctrl Pts',(-0.772546814780815,-0.170638793018057,
-3.33774717864434));
#48716=CARTESIAN_POINT('Ctrl Pts',(-0.78490739088697,-0.114677756662999,
-3.34005373548833));
#48717=CARTESIAN_POINT('Ctrl Pts',(-0.791056339759254,-0.0573447069184797,
-3.34236029233231));
#48718=CARTESIAN_POINT('Ctrl Pts',(-0.791037041324519,-7.57978170876084E-6,
-3.3446668491763));
#48719=CARTESIAN_POINT('Ctrl Pts',(-0.791044053170824,-1.18405052558484E-5,
-3.3731331508237));
#48720=CARTESIAN_POINT('Ctrl Pts',(-0.791071762963029,-0.0521283009703081,
-3.3710365576507));
#48721=CARTESIAN_POINT('Ctrl Pts',(-0.78599872629567,-0.104239438117949,
-3.36893996447771));
#48722=CARTESIAN_POINT('Ctrl Pts',(-0.775772042088009,-0.155318753968962,
-3.36684337130471));
#48723=CARTESIAN_POINT('Ctrl Pts',(-0.749988983637343,-0.284097638645987,
-3.36155753444606));
#48724=CARTESIAN_POINT('Ctrl Pts',(-0.691448188391254,-0.406318036311524,
-3.35627169758742));
#48725=CARTESIAN_POINT('Ctrl Pts',(-0.607265030498785,-0.507124599436057,
-3.35098586072877));
#48726=CARTESIAN_POINT('Ctrl Pts',(-0.523081872606318,-0.607931162560587,
-3.34570002387012));
#48727=CARTESIAN_POINT('Ctrl Pts',(-0.413256352067474,-0.687323891144112,
-3.34041418701147));
#48728=CARTESIAN_POINT('Ctrl Pts',(-0.291137274043885,-0.735652950977678,
-3.33512835015283));
#48729=CARTESIAN_POINT('Ctrl Pts',(-0.169018196020292,-0.783982010811247,
-3.32984251329418));
#48730=CARTESIAN_POINT('Ctrl Pts',(-0.0346055605119571,-0.801247401894854,
-3.32455667643553));
#48731=CARTESIAN_POINT('Ctrl Pts',(0.0957633724903723,-0.785350592480289,
-3.31927083957688));
#48732=CARTESIAN_POINT('Ctrl Pts',(0.226132305492698,-0.769453783065725,
-3.31398500271823));
#48733=CARTESIAN_POINT('Ctrl Pts',(0.352457535989015,-0.720394773152992,
-3.30869916585959));
#48734=CARTESIAN_POINT('Ctrl Pts',(0.459384792216076,-0.644136467916903,
-3.30341332900094));
#48735=CARTESIAN_POINT('Ctrl Pts',(0.566312048443142,-0.56787816268081,
-3.29812749214229));
#48736=CARTESIAN_POINT('Ctrl Pts',(0.653841330400947,-0.46442056212136,
-3.29284165528365));
#48737=CARTESIAN_POINT('Ctrl Pts',(0.71133384188748,-0.346338478955874,
-3.287555818425));
#48738=CARTESIAN_POINT('Ctrl Pts',(0.768826353374009,-0.228256395790395,
-3.28226998156635));
#48739=CARTESIAN_POINT('Ctrl Pts',(0.79628209438927,-0.0955498300188732,
-3.2769841447077));
#48740=CARTESIAN_POINT('Ctrl Pts',(0.790363941324987,0.0356513235813738,
-3.27169830784905));
#48741=CARTESIAN_POINT('Ctrl Pts',(0.784445788260703,0.166852477181624,
-3.2664124709904));
#48742=CARTESIAN_POINT('Ctrl Pts',(0.745153741116876,0.296548218610608,
-3.26112663413176));
#48743=CARTESIAN_POINT('Ctrl Pts',(0.677263574041,0.408974605442786,-3.25584079727311));
#48744=CARTESIAN_POINT('Ctrl Pts',(0.609373406965123,0.521400992274967,
-3.25055496041446));
#48745=CARTESIAN_POINT('Ctrl Pts',(0.512885119957205,0.616558024510333,
-3.24526912355581));
#48746=CARTESIAN_POINT('Ctrl Pts',(0.399526436567544,0.682879786714698,
-3.23998328669717));
#48747=CARTESIAN_POINT('Ctrl Pts',(0.286167753177889,0.749201548919059,
-3.23469744983852));
#48748=CARTESIAN_POINT('Ctrl Pts',(0.15593867340649,0.786688041092416,-3.22941161297987));
#48749=CARTESIAN_POINT('Ctrl Pts',(0.0246679645901216,0.790782946289847,
-3.22412577612122));
#48750=CARTESIAN_POINT('Ctrl Pts',(-0.106602744226251,0.794877851487278,
-3.21883993926257));
#48751=CARTESIAN_POINT('Ctrl Pts',(-0.238915082087602,0.765581169708787,
-3.21355410240393));
#48752=CARTESIAN_POINT('Ctrl Pts',(-0.35618707087149,0.706453782751469,
-3.20826826554528));
#48753=CARTESIAN_POINT('Ctrl Pts',(-0.473459059655378,0.64732639579415,
-3.20298242868663));
#48754=CARTESIAN_POINT('Ctrl Pts',(-0.575690699361802,0.558368303658006,
-3.19769659182798));
#48755=CARTESIAN_POINT('Ctrl Pts',(-0.650456187380403,0.450391968088266,
-3.19241075496933));
#48756=CARTESIAN_POINT('Ctrl Pts',(-0.725221675399004,0.342415632518525,
-3.18712491811069));
#48757=CARTESIAN_POINT('Ctrl Pts',(-0.772521011729782,0.215421053515189,
-3.18183908125204));
#48758=CARTESIAN_POINT('Ctrl Pts',(-0.786605171721123,0.0848438591852945,
-3.17655324439339));
#48759=CARTESIAN_POINT('Ctrl Pts',(-0.789642795110382,0.05668141713378,
-3.1754132132035));
#48760=CARTESIAN_POINT('Ctrl Pts',(-0.791135368568485,0.0283523247683521,
-3.1742731820136));
#48761=CARTESIAN_POINT('Ctrl Pts',(-0.791106220557104,2.01772645531753E-5,
-3.1731331508237));
#48762=CARTESIAN_POINT('Origin',(0.,0.,-2.94));
#48763=CARTESIAN_POINT('',(-0.791107863766246,-2.00924285314041E-5,-2.9446668491763));
#48764=CARTESIAN_POINT('',(-0.791124187626007,-1.85461628832581E-5,-2.9731331508237));
#48765=CARTESIAN_POINT('',(-0.7911,-9.68818082805471E-17,-2.94));
#48766=CARTESIAN_POINT('Ctrl Pts',(-0.791107863766246,-2.00924285314041E-5,
-2.9446668491763));
#48767=CARTESIAN_POINT('Ctrl Pts',(-0.791001312710621,0.103530253044447,
-2.9488335410581));
#48768=CARTESIAN_POINT('Ctrl Pts',(-0.770561409006878,0.207121421232705,
-2.9530002329399));
#48769=CARTESIAN_POINT('Ctrl Pts',(-0.73094283724062,0.302768471603754,
-2.9571669248217));
#48770=CARTESIAN_POINT('Ctrl Pts',(-0.680682987731794,0.424105666340949,
-2.96245276168035));
#48771=CARTESIAN_POINT('Ctrl Pts',(-0.599558358653987,0.53265816484695,
-2.967738598539));
#48772=CARTESIAN_POINT('Ctrl Pts',(-0.497429289043663,0.61523189214487,
-2.97302443539765));
#48773=CARTESIAN_POINT('Ctrl Pts',(-0.395300219433336,0.697805619442793,
-2.9783102722563));
#48774=CARTESIAN_POINT('Ctrl Pts',(-0.272166709290493,0.754400575532634,
-2.98359610911494));
#48775=CARTESIAN_POINT('Ctrl Pts',(-0.142995090918413,0.778137894388827,
-2.98888194597359));
#48776=CARTESIAN_POINT('Ctrl Pts',(-0.013823472546338,0.801875213245019,
-2.99416778283224));
#48777=CARTESIAN_POINT('Ctrl Pts',(0.121386254054973,0.792754894867565,
-2.99945361969088));
#48778=CARTESIAN_POINT('Ctrl Pts',(0.246199946005947,0.751885473524598,
-3.00473945654953));
#48779=CARTESIAN_POINT('Ctrl Pts',(0.371013637956925,0.71101605218163,-3.01002529340818));
#48780=CARTESIAN_POINT('Ctrl Pts',(0.485431295257566,0.638397527873147,
-3.01531113026683));
#48781=CARTESIAN_POINT('Ctrl Pts',(0.575545958879919,0.542856360308726,
-3.02059696712548));
#48782=CARTESIAN_POINT('Ctrl Pts',(0.665660622502271,0.447315192744304,
-3.02588280398412));
#48783=CARTESIAN_POINT('Ctrl Pts',(0.731472292446335,0.328851381923943,
-3.03116864084277));
#48784=CARTESIAN_POINT('Ctrl Pts',(0.764981851975537,0.201863678899196,
-3.03645447770142));
#48785=CARTESIAN_POINT('Ctrl Pts',(0.79849141150474,0.0748759758744486,
-3.04174031456007));
#48786=CARTESIAN_POINT('Ctrl Pts',(0.799698860619082,-0.0606356193546861,
-3.04702615141872));
#48787=CARTESIAN_POINT('Ctrl Pts',(0.768457439231372,-0.188200273115115,
-3.05231198827736));
#48788=CARTESIAN_POINT('Ctrl Pts',(0.737216017843662,-0.315764926875544,
-3.05759782513601));
#48789=CARTESIAN_POINT('Ctrl Pts',(0.6735257259539,-0.435382639167268,-3.06288366199466));
#48790=CARTESIAN_POINT('Ctrl Pts',(0.585127836200294,-0.532514407330171,
-3.06816949885331));
#48791=CARTESIAN_POINT('Ctrl Pts',(0.496729946446687,-0.629646175493074,
-3.07345533571196));
#48792=CARTESIAN_POINT('Ctrl Pts',(0.383624458829236,-0.704291999527155,
-3.0787411725706));
#48793=CARTESIAN_POINT('Ctrl Pts',(0.259558843967787,-0.747379010428274,
-3.08402700942925));
#48794=CARTESIAN_POINT('Ctrl Pts',(0.135493229106338,-0.790466021329393,
-3.0893128462879));
#48795=CARTESIAN_POINT('Ctrl Pts',(0.00046748700088986,-0.801994219097549,
-3.09459868314655));
#48796=CARTESIAN_POINT('Ctrl Pts',(-0.129106601968846,-0.780562402398873,
-3.09988452000519));
#48797=CARTESIAN_POINT('Ctrl Pts',(-0.258680690938578,-0.759130585700196,
-3.10517035686384));
#48798=CARTESIAN_POINT('Ctrl Pts',(-0.382803126772598,-0.704738754534689,
-3.11045619372249));
#48799=CARTESIAN_POINT('Ctrl Pts',(-0.486387377633802,-0.623997994859883,
-3.11574203058114));
#48800=CARTESIAN_POINT('Ctrl Pts',(-0.589971628495012,-0.543257235185072,
-3.12102786743978));
#48801=CARTESIAN_POINT('Ctrl Pts',(-0.673017694383403,-0.436167547000958,
-3.12631370429843));
#48802=CARTESIAN_POINT('Ctrl Pts',(-0.725431694135968,-0.315745207174489,
-3.13159954115708));
#48803=CARTESIAN_POINT('Ctrl Pts',(-0.768623207457408,-0.216511736739724,
-3.13595531049682));
#48804=CARTESIAN_POINT('Ctrl Pts',(-0.791013993106437,-0.10822471912554,
-3.14031107983656));
#48805=CARTESIAN_POINT('Ctrl Pts',(-0.791122594563005,1.8755956602709E-5,
-3.1446668491763));
#48806=CARTESIAN_POINT('Ctrl Pts',(-0.791106220557104,2.01772645531753E-5,
-3.1731331508237));
#48807=CARTESIAN_POINT('Ctrl Pts',(-0.791000221710857,-0.10301172113433,
-3.16898734515495));
#48808=CARTESIAN_POINT('Ctrl Pts',(-0.770769978441601,-0.206084022690134,
-3.1648415394862));
#48809=CARTESIAN_POINT('Ctrl Pts',(-0.731537412905569,-0.301329039654824,
-3.16069573381745));
#48810=CARTESIAN_POINT('Ctrl Pts',(-0.681516510446771,-0.422764934508594,
-3.1554098969588));
#48811=CARTESIAN_POINT('Ctrl Pts',(-0.600605721877271,-0.531476914559684,
-3.15012406010015));
#48812=CARTESIAN_POINT('Ctrl Pts',(-0.498639394867715,-0.614251520556384,
-3.14483822324151));
#48813=CARTESIAN_POINT('Ctrl Pts',(-0.396673067858159,-0.697026126553084,
-3.13955238638286));
#48814=CARTESIAN_POINT('Ctrl Pts',(-0.273651202408545,-0.753863358495396,
-3.13426654952421));
#48815=CARTESIAN_POINT('Ctrl Pts',(-0.144526560904618,-0.777854902801901,
-3.12898071266556));
#48816=CARTESIAN_POINT('Ctrl Pts',(-0.0154019194006878,-0.801846447108407,
-3.12369487580691));
#48817=CARTESIAN_POINT('Ctrl Pts',(0.119825498157559,-0.792992303779106,
-3.11840903894826));
#48818=CARTESIAN_POINT('Ctrl Pts',(0.244719398633153,-0.752368654684988,
-3.11312320208962));
#48819=CARTESIAN_POINT('Ctrl Pts',(0.36961329910874,-0.711745005590873,
-3.10783736523097));
#48820=CARTESIAN_POINT('Ctrl Pts',(0.484173682501678,-0.639351850731945,
-3.10255152837232));
#48821=CARTESIAN_POINT('Ctrl Pts',(0.574476242060206,-0.543988257160257,
-3.09726569151368));
#48822=CARTESIAN_POINT('Ctrl Pts',(0.664778801618738,-0.448624663588567,
-3.09197985465503));
#48823=CARTESIAN_POINT('Ctrl Pts',(0.73082353734286,-0.330290631304114,
-3.08669401779638));
#48824=CARTESIAN_POINT('Ctrl Pts',(0.764583004383618,-0.203369137352724,
-3.08140818093773));
#48825=CARTESIAN_POINT('Ctrl Pts',(0.798342471424376,-0.0764476434013388,
-3.07612234407908));
#48826=CARTESIAN_POINT('Ctrl Pts',(0.799816669781773,0.0590613122169849,
-3.07083650722044));
#48827=CARTESIAN_POINT('Ctrl Pts',(0.768826417180635,0.186687216662146,
-3.06555067036179));
#48828=CARTESIAN_POINT('Ctrl Pts',(0.737836164579496,0.31431312110731,-3.06026483350314));
#48829=CARTESIAN_POINT('Ctrl Pts',(0.674381461019825,0.434055974379303,
-3.05497899664449));
#48830=CARTESIAN_POINT('Ctrl Pts',(0.586174944422666,0.531361563486629,
-3.04969315978585));
#48831=CARTESIAN_POINT('Ctrl Pts',(0.497968427825508,0.628667152593956,
-3.0444073229272));
#48832=CARTESIAN_POINT('Ctrl Pts',(0.385010098190864,0.703535477536607,
-3.03912148606855));
#48833=CARTESIAN_POINT('Ctrl Pts',(0.261029539738131,0.746866625311354,
-3.0338356492099));
#48834=CARTESIAN_POINT('Ctrl Pts',(0.137048981285398,0.790197773086102,
-3.02854981235125));
#48835=CARTESIAN_POINT('Ctrl Pts',(0.00204619401457248,0.801991743692947,
-3.0232639754926));
#48836=CARTESIAN_POINT('Ctrl Pts',(-0.127569831753022,0.780815032287658,
-3.01797813863396));
#48837=CARTESIAN_POINT('Ctrl Pts',(-0.257185857520617,0.759638320882368,
-3.01269230177531));
#48838=CARTESIAN_POINT('Ctrl Pts',(-0.381415121784982,0.705490927464944,
-3.00740646491666));
#48839=CARTESIAN_POINT('Ctrl Pts',(-0.485158108186877,0.624954227668236,
-3.00212062805802));
#48840=CARTESIAN_POINT('Ctrl Pts',(-0.588901094588771,0.544417527871529,
-2.99683479119937));
#48841=CARTESIAN_POINT('Ctrl Pts',(-0.672157803128195,0.437491521695538,
-2.99154895434072));
#48842=CARTESIAN_POINT('Ctrl Pts',(-0.724808749961695,0.317172591184729,
-2.98626311748207));
#48843=CARTESIAN_POINT('Ctrl Pts',(-0.768403560959603,0.217548912019442,
-2.98188646192928));
#48844=CARTESIAN_POINT('Ctrl Pts',(-0.791015717938958,0.108743331083034,
-2.97750980637649));
#48845=CARTESIAN_POINT('Ctrl Pts',(-0.791124187626007,-1.85461628832581E-5,
-2.9731331508237));
#48846=CARTESIAN_POINT('Origin',(0.,0.,-2.94));
#48847=CARTESIAN_POINT('',(-0.79104321788868,1.14421256602881E-5,-2.74466684917629));
#48848=CARTESIAN_POINT('',(-0.791036517039322,7.12926283942606E-6,-2.7731331508237));
#48849=CARTESIAN_POINT('',(-0.7911,-9.68818082805471E-17,-2.94));
#48850=CARTESIAN_POINT('Ctrl Pts',(-0.79104321788868,1.14421256602881E-5,
-2.74466684917629));
#48851=CARTESIAN_POINT('Ctrl Pts',(-0.791070225503421,0.0526472450371811,
-2.74678432856234));
#48852=CARTESIAN_POINT('Ctrl Pts',(-0.785894891195464,0.105277808041528,
-2.74890180794839));
#48853=CARTESIAN_POINT('Ctrl Pts',(-0.775464798820223,0.156845543453911,
-2.75101928733444));
#48854=CARTESIAN_POINT('Ctrl Pts',(-0.749428291886831,0.28557342546107,
-2.75630512419308));
#48855=CARTESIAN_POINT('Ctrl Pts',(-0.690647021806916,0.407678350270431,
-2.76159096105174));
#48856=CARTESIAN_POINT('Ctrl Pts',(-0.606265591379539,0.508319005566248,
-2.76687679791038));
#48857=CARTESIAN_POINT('Ctrl Pts',(-0.52188416095216,0.608959660862067,
-2.77216263476903));
#48858=CARTESIAN_POINT('Ctrl Pts',(-0.411902570177317,0.688136046644342,
-2.77744847162768));
#48859=CARTESIAN_POINT('Ctrl Pts',(-0.289688593861968,0.736224624212554,
-2.78273430848632));
#48860=CARTESIAN_POINT('Ctrl Pts',(-0.16747461754662,0.784313201780766,
-2.78802014534497));
#48861=CARTESIAN_POINT('Ctrl Pts',(-0.0330282556907639,0.801313971134916,
-2.79330598220362));
#48862=CARTESIAN_POINT('Ctrl Pts',(0.0973091324268148,0.785160564124932,
-2.79859181906227));
#48863=CARTESIAN_POINT('Ctrl Pts',(0.227646520544393,0.769007157114948,
-2.80387765592092));
#48864=CARTESIAN_POINT('Ctrl Pts',(0.353874934923697,0.71969957374083,-2.80916349277956));
#48865=CARTESIAN_POINT('Ctrl Pts',(0.460651871371306,0.643230932179692,
-2.81444932963821));
#48866=CARTESIAN_POINT('Ctrl Pts',(0.567428807818914,0.566762290618553,
-2.81973516649686));
#48867=CARTESIAN_POINT('Ctrl Pts',(0.654754266334829,0.463132590870392,
-2.82502100335551));
#48868=CARTESIAN_POINT('Ctrl Pts',(0.712014224552845,0.344937563546001,
-2.83030684021416));
#48869=CARTESIAN_POINT('Ctrl Pts',(0.769274182770862,0.226742536221606,
-2.8355926770728));
#48870=CARTESIAN_POINT('Ctrl Pts',(0.796468640690977,0.0939821813209887,
-2.84087851393145));
#48871=CARTESIAN_POINT('Ctrl Pts',(0.790292232506861,-0.0372070685483761,
-2.8461643507901));
#48872=CARTESIAN_POINT('Ctrl Pts',(0.784115824322744,-0.168396318417734,
-2.85145018764875));
#48873=CARTESIAN_POINT('Ctrl Pts',(0.744568550034392,-0.298014463255841,
-2.85673602450739));
#48874=CARTESIAN_POINT('Ctrl Pts',(0.676457205517293,-0.410306992158768,
-2.86202186136604));
#48875=CARTESIAN_POINT('Ctrl Pts',(0.608345861000192,-0.522599521061702,
-2.86730769822469));
#48876=CARTESIAN_POINT('Ctrl Pts',(0.511670446254346,-0.617566434029459,
-2.87259353508334));
#48877=CARTESIAN_POINT('Ctrl Pts',(0.398181429377058,-0.683664923782026,
-2.87787937194199));
#48878=CARTESIAN_POINT('Ctrl Pts',(0.28469241249978,-0.749763413534587,
-2.88316520880063));
#48879=CARTESIAN_POINT('Ctrl Pts',(0.154389793491068,-0.786993480071955,
-2.88845104565928));
#48880=CARTESIAN_POINT('Ctrl Pts',(0.0231112780559711,-0.790829973848526,
-2.89373688251793));
#48881=CARTESIAN_POINT('Ctrl Pts',(-0.108167237379137,-0.794666467625097,
-2.89902271937658));
#48882=CARTESIAN_POINT('Ctrl Pts',(-0.240421649240631,-0.765109388640866,
-2.90430855623523));
#48883=CARTESIAN_POINT('Ctrl Pts',(-0.35757702005456,-0.705751268818939,
-2.90959439309387));
#48884=CARTESIAN_POINT('Ctrl Pts',(-0.474732390868486,-0.646393148997013,
-2.91488022995252));
#48885=CARTESIAN_POINT('Ctrl Pts',(-0.576788720634849,-0.557233988337392,
-2.92016606681117));
#48886=CARTESIAN_POINT('Ctrl Pts',(-0.65134151488935,-0.449110687572994,
-2.92545190366982));
#48887=CARTESIAN_POINT('Ctrl Pts',(-0.725894309143851,-0.340987386808595,
-2.93073774052846));
#48888=CARTESIAN_POINT('Ctrl Pts',(-0.772943567886491,-0.213899945939417,
-2.93602357738711));
#48889=CARTESIAN_POINT('Ctrl Pts',(-0.786770662287891,-0.0832952800206322,
-2.94130941424576));
#48890=CARTESIAN_POINT('Ctrl Pts',(-0.789698206905234,-0.0556429782708374,
-2.94242855922261));
#48891=CARTESIAN_POINT('Ctrl Pts',(-0.791136482651938,-0.0278330078717755,
-2.94354770419945));
#48892=CARTESIAN_POINT('Ctrl Pts',(-0.791107863766246,-2.00924285314041E-5,
-2.9446668491763));
#48893=CARTESIAN_POINT('Ctrl Pts',(-0.791124187626007,-1.85461628832581E-5,
-2.9731331508237));
#48894=CARTESIAN_POINT('Ctrl Pts',(-0.79114672049626,-0.0226121143313561,
-2.97222396951784));
#48895=CARTESIAN_POINT('Ctrl Pts',(-0.790198139977264,-0.045203796531612,
-2.97131478821199));
#48896=CARTESIAN_POINT('Ctrl Pts',(-0.788264810819136,-0.067710890144367,
-2.97040560690613));
#48897=CARTESIAN_POINT('Ctrl Pts',(-0.777024739715503,-0.19856358611703,
-2.96511977004748));
#48898=CARTESIAN_POINT('Ctrl Pts',(-0.732499412380662,-0.326557123216728,
-2.95983393318883));
#48899=CARTESIAN_POINT('Ctrl Pts',(-0.660100684970037,-0.436134454408224,
-2.95454809633018));
#48900=CARTESIAN_POINT('Ctrl Pts',(-0.587701957559412,-0.54571178559972,
-2.94926225947154));
#48901=CARTESIAN_POINT('Ctrl Pts',(-0.487429830073004,-0.636872910883013,
-2.94397642261289));
#48902=CARTESIAN_POINT('Ctrl Pts',(-0.371471935097405,-0.69853759959995,
-2.93869058575424));
#48903=CARTESIAN_POINT('Ctrl Pts',(-0.255514040121806,-0.760202288316887,
-2.93340474889559));
#48904=CARTESIAN_POINT('Ctrl Pts',(-0.123870377657018,-0.792370540467468,
-2.92811891203694));
#48905=CARTESIAN_POINT('Ctrl Pts',(0.00745834870471288,-0.791132447605627,
-2.9228330751783));
#48906=CARTESIAN_POINT('Ctrl Pts',(0.138787075066443,-0.789894354743785,
-2.91754723831965));
#48907=CARTESIAN_POINT('Ctrl Pts',(0.269800865325114,-0.755249916869522,
-2.912261401461));
#48908=CARTESIAN_POINT('Ctrl Pts',(0.384575574062887,-0.691410011826609,
-2.90697556460235));
#48909=CARTESIAN_POINT('Ctrl Pts',(0.499350282800658,-0.627570106783698,
-2.90168972774371));
#48910=CARTESIAN_POINT('Ctrl Pts',(0.597885910017537,-0.534534734572132,
-2.89640389088506));
#48911=CARTESIAN_POINT('Ctrl Pts',(0.668205887036723,-0.423611932255616,
-2.89111805402641));
#48912=CARTESIAN_POINT('Ctrl Pts',(0.738525864055913,-0.312689129939094,
-2.88583221716776));
#48913=CARTESIAN_POINT('Ctrl Pts',(0.780630190877411,-0.183878897517624,
-2.88054638030912));
#48914=CARTESIAN_POINT('Ctrl Pts',(0.789401273225829,-0.0528375477223508,
-2.87526054345047));
#48915=CARTESIAN_POINT('Ctrl Pts',(0.798172355574245,0.078203802072915,
-2.86997470659182));
#48916=CARTESIAN_POINT('Ctrl Pts',(0.773610193449577,0.211476269241981,
-2.86468886973317));
#48917=CARTESIAN_POINT('Ctrl Pts',(0.718700208773271,0.330781176201317,
-2.85940303287452));
#48918=CARTESIAN_POINT('Ctrl Pts',(0.663790224096964,0.450086083160657,
-2.85411719601588));
#48919=CARTESIAN_POINT('Ctrl Pts',(0.578532416869019,0.555423429910273,
-2.84883135915723));
#48920=CARTESIAN_POINT('Ctrl Pts',(0.473289495607546,0.633989928916403,
-2.84354552229858));
#48921=CARTESIAN_POINT('Ctrl Pts',(0.368046574346073,0.712556427922533,
-2.83825968543993));
#48922=CARTESIAN_POINT('Ctrl Pts',(0.242818539051075,0.764352079185176,
-2.83297384858128));
#48923=CARTESIAN_POINT('Ctrl Pts',(0.112826302272981,0.783081350905049,
-2.82768801172263));
#48924=CARTESIAN_POINT('Ctrl Pts',(-0.0171659345051129,0.801810622624923,
-2.82240217486399));
#48925=CARTESIAN_POINT('Ctrl Pts',(-0.1519223727663,0.787473514802027,-2.81711633800534));
#48926=CARTESIAN_POINT('Ctrl Pts',(-0.275063964819311,0.7418126393354,-2.81183050114669));
#48927=CARTESIAN_POINT('Ctrl Pts',(-0.398205556872314,0.696151763868776,
-2.80654466428805));
#48928=CARTESIAN_POINT('Ctrl Pts',(-0.50973230271714,0.619167120758426,
-2.8012588274294));
#48929=CARTESIAN_POINT('Ctrl Pts',(-0.596088620797797,0.520215852099155,
-2.79597299057075));
#48930=CARTESIAN_POINT('Ctrl Pts',(-0.682444938878462,0.421264583439876,
-2.7906871537121));
#48931=CARTESIAN_POINT('Ctrl Pts',(-0.743630829194953,0.300346689231674,
-2.78540131685345));
#48932=CARTESIAN_POINT('Ctrl Pts',(-0.772209418018207,0.172159203482865,
-2.78011547999481));
#48933=CARTESIAN_POINT('Ctrl Pts',(-0.784793052344291,0.115716093019316,
-2.77778803693777));
#48934=CARTESIAN_POINT('Ctrl Pts',(-0.791054817880501,0.0578635619115849,
-2.77546059388074));
#48935=CARTESIAN_POINT('Ctrl Pts',(-0.791036517039322,7.12926283942606E-6,
-2.7731331508237));
#48936=CARTESIAN_POINT('Origin',(0.,0.,-2.94));
#48937=CARTESIAN_POINT('',(-0.791167260441282,1.79117177186508E-6,-2.5446668491763));
#48938=CARTESIAN_POINT('',(-0.791162320258143,7.12643492048928E-6,-2.5731331508237));
#48939=CARTESIAN_POINT('',(-0.7911,-9.68818082805471E-17,-2.94));
#48940=CARTESIAN_POINT('Ctrl Pts',(-0.791167260441282,1.79117177186508E-6,
-2.5446668491763));
#48941=CARTESIAN_POINT('Ctrl Pts',(-0.791167483212997,0.00169798683385348,
-2.54473511606659));
#48942=CARTESIAN_POINT('Ctrl Pts',(-0.791162142242542,0.00339418108704642,
-2.54480338295688));
#48943=CARTESIAN_POINT('Ctrl Pts',(-0.791151229004,0.00509033948775599,
-2.54487164984718));
#48944=CARTESIAN_POINT('Ctrl Pts',(-0.790306227887311,0.136422183579185,
-2.55015748670582));
#48945=CARTESIAN_POINT('Ctrl Pts',(-0.756054088695197,0.267539083083683,
-2.55544332356447));
#48946=CARTESIAN_POINT('Ctrl Pts',(-0.69255800710569,0.382504360111667,
-2.56072916042312));
#48947=CARTESIAN_POINT('Ctrl Pts',(-0.629061925516182,0.497469637139652,
-2.56601499728176));
#48948=CARTESIAN_POINT('Ctrl Pts',(-0.53632190152928,0.596283291691123,
-2.57130083414041));
#48949=CARTESIAN_POINT('Ctrl Pts',(-0.425610073941255,0.666934962099274,
-2.57658667099906));
#48950=CARTESIAN_POINT('Ctrl Pts',(-0.31489824635323,0.737586632507426,
-2.58187250785771));
#48951=CARTESIAN_POINT('Ctrl Pts',(-0.186214615164082,0.780076318772257,
-2.58715834471636));
#48952=CARTESIAN_POINT('Ctrl Pts',(-0.0552001052864145,0.789239587886346,
-2.592444181575));
#48953=CARTESIAN_POINT('Ctrl Pts',(0.0758144045912454,0.798402857000435,
-2.59773001843365));
#48954=CARTESIAN_POINT('Ctrl Pts',(0.209159793157424,0.774239708963784,
-2.6030158552923));
#48955=CARTESIAN_POINT('Ctrl Pts',(0.328628519556054,0.719687067304282,
-2.60830169215095));
#48956=CARTESIAN_POINT('Ctrl Pts',(0.448097245954693,0.665134425644775,
-2.6135875290096));
#48957=CARTESIAN_POINT('Ctrl Pts',(0.553689310185781,0.580192290362409,
-2.61887336586824));
#48958=CARTESIAN_POINT('Ctrl Pts',(0.632570464934848,0.475185001449699,
-2.62415920272689));
#48959=CARTESIAN_POINT('Ctrl Pts',(0.711451619683911,0.370177712536995,
-2.62944503958554));
#48960=CARTESIAN_POINT('Ctrl Pts',(0.763621864950956,0.245105269993949,
-2.63473087644419));
#48961=CARTESIAN_POINT('Ctrl Pts',(0.782740138696053,0.115169674761737,
-2.64001671330283));
#48962=CARTESIAN_POINT('Ctrl Pts',(0.801858412441151,-0.0147659204704824,
-2.64530255016148));
#48963=CARTESIAN_POINT('Ctrl Pts',(0.787924714664298,-0.149564668391867,
-2.65058838702013));
#48964=CARTESIAN_POINT('Ctrl Pts',(0.742632624561765,-0.272842378759507,
-2.65587422387878));
#48965=CARTESIAN_POINT('Ctrl Pts',(0.697340534459234,-0.396120089127139,
-2.66116006073743));
#48966=CARTESIAN_POINT('Ctrl Pts',(0.620690052031027,-0.507876761941027,
-2.66644589759607));
#48967=CARTESIAN_POINT('Ctrl Pts',(0.52199770362238,-0.594528869041363,
-2.67173173445472));
#48968=CARTESIAN_POINT('Ctrl Pts',(0.423305355213725,-0.681180976141705,
-2.67701757131337));
#48969=CARTESIAN_POINT('Ctrl Pts',(0.302571140824627,-0.74272851752849,
-2.68230340817202));
#48970=CARTESIAN_POINT('Ctrl Pts',(0.17446976899565,-0.771690662388269,
-2.68758924503066));
#48971=CARTESIAN_POINT('Ctrl Pts',(0.0463683971666843,-0.800652807248045,
-2.69287508188931));
#48972=CARTESIAN_POINT('Ctrl Pts',(-0.0891001321021591,-0.797029555580821,
-2.69816091874796));
#48973=CARTESIAN_POINT('Ctrl Pts',(-0.215470219614348,-0.761261297564762,
-2.70344675560661));
#48974=CARTESIAN_POINT('Ctrl Pts',(-0.341840307126537,-0.725493039548704,
-2.70873259246526));
#48975=CARTESIAN_POINT('Ctrl Pts',(-0.459111952882072,-0.657579775183812,
-2.7140184293239));
#48976=CARTESIAN_POINT('Ctrl Pts',(-0.553031308208128,-0.565776060692079,
-2.71930426618255));
#48977=CARTESIAN_POINT('Ctrl Pts',(-0.646950663534187,-0.473972346200343,
-2.7245901030412));
#48978=CARTESIAN_POINT('Ctrl Pts',(-0.717517728430766,-0.358278181581765,
-2.72987593989985));
#48979=CARTESIAN_POINT('Ctrl Pts',(-0.756155388985624,-0.232755679669995,
-2.7351617767585));
#48980=CARTESIAN_POINT('Ctrl Pts',(-0.779314999056162,-0.157516854192255,
-2.7383301342311));
#48981=CARTESIAN_POINT('Ctrl Pts',(-0.791002806738258,-0.0787468402830678,
-2.7414984917037));
#48982=CARTESIAN_POINT('Ctrl Pts',(-0.79104321788868,1.14421256602881E-5,
-2.74466684917629));
#48983=CARTESIAN_POINT('Ctrl Pts',(-0.791036517039322,7.12926283942606E-6,
-2.7731331508237));
#48984=CARTESIAN_POINT('Ctrl Pts',(-0.791013254990033,-0.0735337082730062,
-2.77017475702209));
#48985=CARTESIAN_POINT('Ctrl Pts',(-0.780843450574848,-0.14708084942872,
-2.76721636322048));
#48986=CARTESIAN_POINT('Ctrl Pts',(-0.760612952173891,-0.217747821126159,
-2.76425796941886));
#48987=CARTESIAN_POINT('Ctrl Pts',(-0.724466610176304,-0.34401028269698,
-2.75897213256022));
#48988=CARTESIAN_POINT('Ctrl Pts',(-0.65620263885111,-0.461078128549208,
-2.75368629570157));
#48989=CARTESIAN_POINT('Ctrl Pts',(-0.564118221296634,-0.554722280984812,
-2.74840045884292));
#48990=CARTESIAN_POINT('Ctrl Pts',(-0.472033803742163,-0.64836643342041,
-2.74311462198427));
#48991=CARTESIAN_POINT('Ctrl Pts',(-0.356128939958412,-0.718586892439387,
-2.73782878512563));
#48992=CARTESIAN_POINT('Ctrl Pts',(-0.230491352328523,-0.75684867253741,
-2.73254294826698));
#48993=CARTESIAN_POINT('Ctrl Pts',(-0.104853764698629,-0.795110452635434,
-2.72725711140833));
#48994=CARTESIAN_POINT('Ctrl Pts',(0.0305165467774051,-0.801413553812501,
-2.72197127454968));
#48995=CARTESIAN_POINT('Ctrl Pts',(0.15916592084036,-0.774991862062378,
-2.71668543769103));
#48996=CARTESIAN_POINT('Ctrl Pts',(0.287815294903315,-0.748570170312255,
-2.71139960083238));
#48997=CARTESIAN_POINT('Ctrl Pts',(0.409743731553193,-0.68942368563494,
-2.70611376397374));
#48998=CARTESIAN_POINT('Ctrl Pts',(0.510131369827653,-0.604741401044805,
-2.70082792711509));
#48999=CARTESIAN_POINT('Ctrl Pts',(0.610519008102113,-0.520059116454669,
-2.69554209025644));
#49000=CARTESIAN_POINT('Ctrl Pts',(0.689365848001159,-0.40984103195171,
-2.69025625339779));
#49001=CARTESIAN_POINT('Ctrl Pts',(0.737088405665489,-0.287483667107157,
-2.68497041653915));
#49002=CARTESIAN_POINT('Ctrl Pts',(0.784810963329821,-0.165126302262599,
-2.6796845796805));
#49003=CARTESIAN_POINT('Ctrl Pts',(0.801409238759436,-0.0306296570764548,
-2.67439874282185));
#49004=CARTESIAN_POINT('Ctrl Pts',(0.784865785156526,0.0996587974566231,
-2.6691129059632));
#49005=CARTESIAN_POINT('Ctrl Pts',(0.768322331553618,0.229947251989694,
-2.66382706910455));
#49006=CARTESIAN_POINT('Ctrl Pts',(0.718637148918179,0.3560275158697,-2.65854123224591));
#49007=CARTESIAN_POINT('Ctrl Pts',(0.641849250943637,0.462575091939637,
-2.65325539538726));
#49008=CARTESIAN_POINT('Ctrl Pts',(0.56506135296909,0.56912266800958,-2.64796955852861));
#49009=CARTESIAN_POINT('Ctrl Pts',(0.461170739655441,0.656137556269456,
-2.64268372166996));
#49010=CARTESIAN_POINT('Ctrl Pts',(0.342804854500712,0.713043482790928,
-2.63739788481132));
#49011=CARTESIAN_POINT('Ctrl Pts',(0.224438969345987,0.769949409312398,
-2.63211204795267));
#49012=CARTESIAN_POINT('Ctrl Pts',(0.0915978123501881,0.796746374095458,
-2.62682621109402));
#49013=CARTESIAN_POINT('Ctrl Pts',(-0.0395723627427169,0.790177324862483,
-2.62154037423537));
#49014=CARTESIAN_POINT('Ctrl Pts',(-0.170742537835622,0.783608275629508,
-2.61625453737672));
#49015=CARTESIAN_POINT('Ctrl Pts',(-0.300241731025636,0.743673212380498,
-2.61096870051808));
#49016=CARTESIAN_POINT('Ctrl Pts',(-0.412329889454358,0.675226065020025,
-2.60568286365943));
#49017=CARTESIAN_POINT('Ctrl Pts',(-0.524418047883078,0.606778917659555,
-2.60039702680078));
#49018=CARTESIAN_POINT('Ctrl Pts',(-0.619095171550508,0.509819686187622,
-2.59511118994213));
#49019=CARTESIAN_POINT('Ctrl Pts',(-0.684853675781432,0.39613333536643,
-2.58982535308349));
#49020=CARTESIAN_POINT('Ctrl Pts',(-0.75061218001236,0.282446984545231,
-2.58453951622484));
#49021=CARTESIAN_POINT('Ctrl Pts',(-0.787452064806777,0.152033514374769,
-2.57925367936619));
#49022=CARTESIAN_POINT('Ctrl Pts',(-0.79089560548025,0.0207441040273998,
-2.57396784250754));
#49023=CARTESIAN_POINT('Ctrl Pts',(-0.791076863108889,0.013833424165714,
-2.57368961194626));
#49024=CARTESIAN_POINT('Ctrl Pts',(-0.791165591053067,0.00692031737765905,
-2.57341138138498));
#49025=CARTESIAN_POINT('Ctrl Pts',(-0.791162320258143,7.12643492048928E-6,
-2.5731331508237));
#49026=CARTESIAN_POINT('Origin',(0.,0.,-2.94));
#49027=CARTESIAN_POINT('',(-0.791049211918833,-1.3923086196882E-5,-2.3446668491763));
#49028=CARTESIAN_POINT('',(-0.791060671368687,-1.7079190050548E-5,-2.3731331508237));
#49029=CARTESIAN_POINT('',(-0.7911,-9.68818082805471E-17,-2.94));
#49030=CARTESIAN_POINT('Ctrl Pts',(-0.791049211918833,-1.3923086196882E-5,
-2.3446668491763));
#49031=CARTESIAN_POINT('Ctrl Pts',(-0.790997411345824,0.0821365012599493,
-2.34797174042948));
#49032=CARTESIAN_POINT('Ctrl Pts',(-0.778263259369705,0.164302615906683,
-2.35127663168267));
#49033=CARTESIAN_POINT('Ctrl Pts',(-0.753097766892199,0.242466352743269,
-2.35458152293585));
#49034=CARTESIAN_POINT('Ctrl Pts',(-0.712848125523398,0.367481286527303,
-2.3598673597945));
#49035=CARTESIAN_POINT('Ctrl Pts',(-0.640798190910364,0.48225784030536,
-2.36515319665315));
#49036=CARTESIAN_POINT('Ctrl Pts',(-0.545705313205766,0.572845432773656,
-2.3704390335118));
#49037=CARTESIAN_POINT('Ctrl Pts',(-0.450612435501175,0.663433025241947,
-2.37572487037045));
#49038=CARTESIAN_POINT('Ctrl Pts',(-0.332476614705023,0.729831656400481,
-2.38101070722909));
#49039=CARTESIAN_POINT('Ctrl Pts',(-0.205656736135409,0.763970866979082,
-2.38629654408774));
#49040=CARTESIAN_POINT('Ctrl Pts',(-0.0788368575657881,0.798110077557686,
-2.39158238094639));
#49041=CARTESIAN_POINT('Ctrl Pts',(0.0566670787772957,0.799989867556354,
-2.39686821780504));
#49042=CARTESIAN_POINT('Ctrl Pts',(0.184385170124397,0.769381756833913,
-2.40215405466368));
#49043=CARTESIAN_POINT('Ctrl Pts',(0.312103261471486,0.738773646111475,
-2.40743989152233));
#49044=CARTESIAN_POINT('Ctrl Pts',(0.432035507822595,0.675677634667934,
-2.41272572838098));
#49045=CARTESIAN_POINT('Ctrl Pts',(0.529604676297028,0.587762762987721,
-2.41801156523963));
#49046=CARTESIAN_POINT('Ctrl Pts',(0.627173844771468,0.499847891307504,
-2.42329740209827));
#49047=CARTESIAN_POINT('Ctrl Pts',(0.70237993536923,0.387114159390612,-2.42858323895692));
#49048=CARTESIAN_POINT('Ctrl Pts',(0.746081981169035,0.263263852599493,
-2.43386907581557));
#49049=CARTESIAN_POINT('Ctrl Pts',(0.789784026968842,0.139413545808374,
-2.43915491267422));
#49050=CARTESIAN_POINT('Ctrl Pts',(0.801982027970691,0.00444666414302769,
-2.44444074953287));
#49051=CARTESIAN_POINT('Ctrl Pts',(0.781193371226918,-0.125232166242399,
-2.44972658639151));
#49052=CARTESIAN_POINT('Ctrl Pts',(0.760404714483145,-0.254910996627825,
-2.45501242325016));
#49053=CARTESIAN_POINT('Ctrl Pts',(0.706629399993748,-0.379301775733332,
-2.46029826010881));
#49054=CARTESIAN_POINT('Ctrl Pts',(0.626403578847316,-0.483285355786739,
-2.46558409696746));
#49055=CARTESIAN_POINT('Ctrl Pts',(0.546177757700884,-0.587268935840146,
-2.4708699338261));
#49056=CARTESIAN_POINT('Ctrl Pts',(0.439501429897416,-0.670845316841453,
-2.47615577068475));
#49057=CARTESIAN_POINT('Ctrl Pts',(0.31934063018203,-0.723856160176581,
-2.4814416075434));
#49058=CARTESIAN_POINT('Ctrl Pts',(0.199179830466644,-0.776867003511709,
-2.48672744440205));
#49059=CARTESIAN_POINT('Ctrl Pts',(0.0655345588393392,-0.799312309180659,
-2.4920132812607));
#49060=CARTESIAN_POINT('Ctrl Pts',(-0.0653511943871243,-0.788463949780088,
-2.49729911811934));
#49061=CARTESIAN_POINT('Ctrl Pts',(-0.196236947613588,-0.777615590379518,
-2.50258495497799));
#49062=CARTESIAN_POINT('Ctrl Pts',(-0.32436318243921,-0.733473565909427,
-2.50787079183664));
#49063=CARTESIAN_POINT('Ctrl Pts',(-0.434156723008419,-0.661403143761225,
-2.51315662869529));
#49064=CARTESIAN_POINT('Ctrl Pts',(-0.543950263577628,-0.589332721613023,
-2.51844246555394));
#49065=CARTESIAN_POINT('Ctrl Pts',(-0.635411109890424,-0.489333901786708,
-2.52372830241258));
#49066=CARTESIAN_POINT('Ctrl Pts',(-0.697422601526189,-0.373561097534371,
-2.52901413927123));
#49067=CARTESIAN_POINT('Ctrl Pts',(-0.758633211142775,-0.25928350577878,
-2.53423170923958));
#49068=CARTESIAN_POINT('Ctrl Pts',(-0.79115023422254,-0.129636742368248,
-2.53944927920794));
#49069=CARTESIAN_POINT('Ctrl Pts',(-0.791167260441282,1.79117177186508E-6,
-2.5446668491763));
#49070=CARTESIAN_POINT('Ctrl Pts',(-0.791162320258143,7.12643492048928E-6,
-2.5731331508237));
#49071=CARTESIAN_POINT('Ctrl Pts',(-0.791103452342327,-0.124416798601764,
-2.56812554452633));
#49072=CARTESIAN_POINT('Ctrl Pts',(-0.761243465869951,-0.248867983834946,
-2.56311793822897));
#49073=CARTESIAN_POINT('Ctrl Pts',(-0.704677825615191,-0.359687835082198,
-2.5581103319316));
#49074=CARTESIAN_POINT('Ctrl Pts',(-0.644969308524131,-0.476665013320157,
-2.55282449507295));
#49075=CARTESIAN_POINT('Ctrl Pts',(-0.555505077789481,-0.578454019271802,
-2.5475386582143));
#49076=CARTESIAN_POINT('Ctrl Pts',(-0.447159114059393,-0.65268285049746,
-2.54225282135565));
#49077=CARTESIAN_POINT('Ctrl Pts',(-0.338813150329307,-0.726911681723116,
-2.53696698449701));
#49078=CARTESIAN_POINT('Ctrl Pts',(-0.211585453603786,-0.773580338222786,
-2.53168114763836));
#49079=CARTESIAN_POINT('Ctrl Pts',(-0.0809399864155768,-0.787016451682503,
-2.52639531077971));
#49080=CARTESIAN_POINT('Ctrl Pts',(0.0497054807726323,-0.80045256514222,
-2.52110947392107));
#49081=CARTESIAN_POINT('Ctrl Pts',(0.183768718423527,-0.780656135561986,
-2.51582363706242));
#49082=CARTESIAN_POINT('Ctrl Pts',(0.304954934307039,-0.730033331199104,
-2.51053780020377));
#49083=CARTESIAN_POINT('Ctrl Pts',(0.426141150190555,-0.67941052683622,
-2.50525196334512));
#49084=CARTESIAN_POINT('Ctrl Pts',(0.534450344306686,-0.597961347690689,
-2.49996612648647));
#49085=CARTESIAN_POINT('Ctrl Pts',(0.616718014248558,-0.495585580420968,
-2.49468028962783));
#49086=CARTESIAN_POINT('Ctrl Pts',(0.698985684190429,-0.393209813151246,
-2.48939445276918));
#49087=CARTESIAN_POINT('Ctrl Pts',(0.75521182995804,-0.269907457757338,
-2.48410861591053));
#49088=CARTESIAN_POINT('Ctrl Pts',(0.778562412785546,-0.14066536893429,
-2.47882277905188));
#49089=CARTESIAN_POINT('Ctrl Pts',(0.801912995613052,-0.0114232801112452,
-2.47353694219323));
#49090=CARTESIAN_POINT('Ctrl Pts',(0.792388015500453,0.123758542140946,
-2.46825110533458));
#49091=CARTESIAN_POINT('Ctrl Pts',(0.751145191555912,0.248449346592627,
-2.46296526847594));
#49092=CARTESIAN_POINT('Ctrl Pts',(0.709902367611368,0.373140151044316,
-2.45767943161729));
#49093=CARTESIAN_POINT('Ctrl Pts',(0.636941699834886,0.487339937695493,
-2.45239359475864));
#49094=CARTESIAN_POINT('Ctrl Pts',(0.541131233957833,0.577168228729843,
-2.4471077579));
#49095=CARTESIAN_POINT('Ctrl Pts',(0.445320768080786,0.666996519764187,
-2.44182192104135));
#49096=CARTESIAN_POINT('Ctrl Pts',(0.326660504103166,0.732453315181701,
-2.4365360841827));
#49097=CARTESIAN_POINT('Ctrl Pts',(0.199573071086925,0.765582631671333,
-2.43125024732405));
#49098=CARTESIAN_POINT('Ctrl Pts',(0.0724856380706798,0.798711948160966,
-2.4259644104654));
#49099=CARTESIAN_POINT('Ctrl Pts',(-0.0630289639841951,0.799513785722722,
-2.42067857360676));
#49100=CARTESIAN_POINT('Ctrl Pts',(-0.19049953593827,0.767890684555539,
-2.41539273674811));
#49101=CARTESIAN_POINT('Ctrl Pts',(-0.317970107892348,0.736267583388355,
-2.41010689988946));
#49102=CARTESIAN_POINT('Ctrl Pts',(-0.437396649745624,0.672219543492232,
-2.40482106303081));
#49103=CARTESIAN_POINT('Ctrl Pts',(-0.534263394757312,0.58353132018964,
-2.39953522617216));
#49104=CARTESIAN_POINT('Ctrl Pts',(-0.631130139768997,0.49484309688705,
-2.39424938931352));
#49105=CARTESIAN_POINT('Ctrl Pts',(-0.705437087939093,0.381514690177995,
-2.38896355245487));
#49106=CARTESIAN_POINT('Ctrl Pts',(-0.748152559122481,0.257320665509696,
-2.38367771559622));
#49107=CARTESIAN_POINT('Ctrl Pts',(-0.77655651638456,0.174736962903699,
-2.38016286067205));
#49108=CARTESIAN_POINT('Ctrl Pts',(-0.790991733797414,0.0873488318552603,
-2.37664800574787));
#49109=CARTESIAN_POINT('Ctrl Pts',(-0.791060671368687,-1.7079190050548E-5,
-2.3731331508237));
#49110=CARTESIAN_POINT('Origin',(0.,0.,-2.94));
#49111=CARTESIAN_POINT('',(-0.791097165546451,2.04205267731045E-5,-2.14466684917629));
#49112=CARTESIAN_POINT('',(-0.791081243560257,1.98986687146829E-5,-2.1731331508237));
#49113=CARTESIAN_POINT('',(-0.7911,-9.68818082805471E-17,-2.94));
#49114=CARTESIAN_POINT('Ctrl Pts',(-0.791097165546451,2.04205267731045E-5,
-2.14466684917629));
#49115=CARTESIAN_POINT('Ctrl Pts',(-0.791128923376164,0.0312276790823086,
-2.14592252793373));
#49116=CARTESIAN_POINT('Ctrl Pts',(-0.789317367433578,0.0624312734019356,
-2.14717820669116));
#49117=CARTESIAN_POINT('Ctrl Pts',(-0.785633709697737,0.0934122738038864,
-2.14843388544859));
#49118=CARTESIAN_POINT('Ctrl Pts',(-0.770127184864448,0.223828204529152,
-2.15371972230724));
#49119=CARTESIAN_POINT('Ctrl Pts',(-0.721446504630274,0.350299710200771,
-2.15900555916588));
#49120=CARTESIAN_POINT('Ctrl Pts',(-0.645508589874747,0.457454739956378,
-2.16429139602453));
#49121=CARTESIAN_POINT('Ctrl Pts',(-0.569570675119224,0.564609769711979,
-2.16957723288318));
#49122=CARTESIAN_POINT('Ctrl Pts',(-0.466375525842352,0.652448323551568,
-2.17486306974183));
#49123=CARTESIAN_POINT('Ctrl Pts',(-0.348466054971509,0.710294014646916,
-2.18014890660048));
#49124=CARTESIAN_POINT('Ctrl Pts',(-0.230556584100659,0.768139705742269,
-2.18543474345912));
#49125=CARTESIAN_POINT('Ctrl Pts',(-0.097932791635837,0.795992534093376,
-2.19072058031777));
#49126=CARTESIAN_POINT('Ctrl Pts',(0.0332854883741506,0.790467111886595,
-2.19600641717642));
#49127=CARTESIAN_POINT('Ctrl Pts',(0.164503768384138,0.784941689679814,
-2.20129225403507));
#49128=CARTESIAN_POINT('Ctrl Pts',(0.29431653593929,0.746038016915144,-2.20657809089371));
#49129=CARTESIAN_POINT('Ctrl Pts',(0.406945624607212,0.67848466255597,-2.21186392775236));
#49130=CARTESIAN_POINT('Ctrl Pts',(0.51957471327513,0.610931308196797,-2.21714976461101));
#49131=CARTESIAN_POINT('Ctrl Pts',(0.615020123055817,0.514728272243123,
-2.22243560146966));
#49132=CARTESIAN_POINT('Ctrl Pts',(0.681680887502828,0.40156860724414,-2.22772143832831));
#49133=CARTESIAN_POINT('Ctrl Pts',(0.748341651949842,0.288408942245151,
-2.23300727518695));
#49134=CARTESIAN_POINT('Ctrl Pts',(0.786217771063174,0.158292648200854,
-2.2382931120456));
#49135=CARTESIAN_POINT('Ctrl Pts',(0.790705570470584,0.0270347838428554,
-2.24357894890425));
#49136=CARTESIAN_POINT('Ctrl Pts',(0.795193369877993,-0.104223080515135,
-2.2488647857629));
#49137=CARTESIAN_POINT('Ctrl Pts',(0.766292849579479,-0.236622515186834,
-2.25415062262155));
#49138=CARTESIAN_POINT('Ctrl Pts',(0.70751673970045,-0.354070955818585,
-2.25943645948019));
#49139=CARTESIAN_POINT('Ctrl Pts',(0.648740629821416,-0.471519396450344,
-2.26472229633884));
#49140=CARTESIAN_POINT('Ctrl Pts',(0.560088930361871,-0.574016843042153,
-2.27000813319749));
#49141=CARTESIAN_POINT('Ctrl Pts',(0.452336862395436,-0.649105185335084,
-2.27529397005613));
#49142=CARTESIAN_POINT('Ctrl Pts',(0.344584794429007,-0.72419352762801,
-2.28057980691478));
#49143=CARTESIAN_POINT('Ctrl Pts',(0.217732357955687,-0.771872765622055,
-2.28586564377343));
#49144=CARTESIAN_POINT('Ctrl Pts',(0.0871979042881309,-0.786347699302541,
-2.29115148063208));
#49145=CARTESIAN_POINT('Ctrl Pts',(-0.0433365493794288,-0.800822632983027,
-2.29643731749073));
#49146=CARTESIAN_POINT('Ctrl Pts',(-0.177553020241233,-0.782093262349958,
-2.30172315434938));
#49147=CARTESIAN_POINT('Ctrl Pts',(-0.299138091249714,-0.732436059375915,
-2.30700899120802));
#49148=CARTESIAN_POINT('Ctrl Pts',(-0.420723162258195,-0.682778856401872,
-2.31229482806667));
#49149=CARTESIAN_POINT('Ctrl Pts',(-0.529676833413351,-0.602193821086856,
-2.31758066492532));
#49150=CARTESIAN_POINT('Ctrl Pts',(-0.612756268981202,-0.500475707237502,
-2.32286650178397));
#49151=CARTESIAN_POINT('Ctrl Pts',(-0.69583570454905,-0.398757593388151,
-2.32815233864261));
#49152=CARTESIAN_POINT('Ctrl Pts',(-0.753040904529592,-0.275906401004465,
-2.33343817550126));
#49153=CARTESIAN_POINT('Ctrl Pts',(-0.77741883045758,-0.146854147917619,
-2.33872401235991));
#49154=CARTESIAN_POINT('Ctrl Pts',(-0.786554819049114,-0.0984899057997243,
-2.34070495796537));
#49155=CARTESIAN_POINT('Ctrl Pts',(-0.791080261084932,-0.0492547330337058,
-2.34268590357083));
#49156=CARTESIAN_POINT('Ctrl Pts',(-0.791049211918833,-1.3923086196882E-5,
-2.3446668491763));
#49157=CARTESIAN_POINT('Ctrl Pts',(-0.791060671368687,-1.7079190050548E-5,
-2.3731331508237));
#49158=CARTESIAN_POINT('Ctrl Pts',(-0.791095406000973,-0.0440369472892742,
-2.37136216888922));
#49159=CARTESIAN_POINT('Ctrl Pts',(-0.78748295578056,-0.0880511743694083,
-2.36959118695475));
#49160=CARTESIAN_POINT('Ctrl Pts',(-0.780172469530915,-0.131442361535027,
-2.36782020502028));
#49161=CARTESIAN_POINT('Ctrl Pts',(-0.758352914559283,-0.260951721283921,
-2.36253436816163));
#49162=CARTESIAN_POINT('Ctrl Pts',(-0.703589810419337,-0.384910798154171,
-2.35724853130298));
#49163=CARTESIAN_POINT('Ctrl Pts',(-0.62253936965279,-0.488252915866539,
-2.35196269444433));
#49164=CARTESIAN_POINT('Ctrl Pts',(-0.541488928886243,-0.591595033578908,
-2.34667685758569));
#49165=CARTESIAN_POINT('Ctrl Pts',(-0.434151151493092,-0.674320192133397,
-2.34139102072704));
#49166=CARTESIAN_POINT('Ctrl Pts',(-0.313572468483857,-0.726373515230843,
-2.33610518386839));
#49167=CARTESIAN_POINT('Ctrl Pts',(-0.192993785474619,-0.77842683832829,
-2.33081934700974));
#49168=CARTESIAN_POINT('Ctrl Pts',(-0.059174196849305,-0.799808325968691,
-2.32553351015109));
#49169=CARTESIAN_POINT('Ctrl Pts',(0.0716211196209889,-0.787919153114142,
-2.32024767329245));
#49170=CARTESIAN_POINT('Ctrl Pts',(0.202416436091275,-0.776029980259594,
-2.3149618364338));
#49171=CARTESIAN_POINT('Ctrl Pts',(0.330187480406542,-0.730870146910091,
-2.30967599957515));
#49172=CARTESIAN_POINT('Ctrl Pts',(0.43940424854316,-0.657928630614363,
-2.3043901627165));
#49173=CARTESIAN_POINT('Ctrl Pts',(0.548621016679781,-0.584987114318634,
-2.29910432585786));
#49174=CARTESIAN_POINT('Ctrl Pts',(0.639283508637765,-0.484263915076674,
-2.29381848899921));
#49175=CARTESIAN_POINT('Ctrl Pts',(0.700372100429191,-0.368001491247351,
-2.28853265214056));
#49176=CARTESIAN_POINT('Ctrl Pts',(0.761460692220617,-0.251739067418028,
-2.28324681528191));
#49177=CARTESIAN_POINT('Ctrl Pts',(0.792975383845487,-0.11993741900134,
-2.27796097842326));
#49178=CARTESIAN_POINT('Ctrl Pts',(0.791085704242379,0.0113835479183653,
-2.27267514156462));
#49179=CARTESIAN_POINT('Ctrl Pts',(0.789196024639272,0.142704514838074,
-2.26738930470597));
#49180=CARTESIAN_POINT('Ctrl Pts',(0.75390197380819,0.273544800260791,-2.26210346784732));
#49181=CARTESIAN_POINT('Ctrl Pts',(0.689493387168049,0.388001347512353,
-2.25681763098867));
#49182=CARTESIAN_POINT('Ctrl Pts',(0.625084800527912,0.502457894763909,
-2.25153179413003));
#49183=CARTESIAN_POINT('Ctrl Pts',(0.531561678078721,0.600530703844302,
-2.24624595727138));
#49184=CARTESIAN_POINT('Ctrl Pts',(0.420291340763339,0.670299459569546,
-2.24096012041273));
#49185=CARTESIAN_POINT('Ctrl Pts',(0.309021003447957,0.74006821529479,-2.23567428355408));
#49186=CARTESIAN_POINT('Ctrl Pts',(0.180003451266383,0.781532917664886,
-2.23038844669544));
#49187=CARTESIAN_POINT('Ctrl Pts',(0.0489201957475688,0.78965371592103,
-2.22510260983679));
#49188=CARTESIAN_POINT('Ctrl Pts',(-0.0821630597712489,0.797774514177174,
-2.21981677297814));
#49189=CARTESIAN_POINT('Ctrl Pts',(-0.215312018627309,0.772551408319364,
-2.21453093611949));
#49190=CARTESIAN_POINT('Ctrl Pts',(-0.334343015125024,0.717050155049826,
-2.20924509926084));
#49191=CARTESIAN_POINT('Ctrl Pts',(-0.453374011622743,0.661548901780285,
-2.20395926240219));
#49192=CARTESIAN_POINT('Ctrl Pts',(-0.558287045762119,0.575769501099013,
-2.19867342554355));
#49193=CARTESIAN_POINT('Ctrl Pts',(-0.636330403326168,0.470138058896137,
-2.1933875886849));
#49194=CARTESIAN_POINT('Ctrl Pts',(-0.714373760890212,0.364506616693267,
-2.18810175182625));
#49195=CARTESIAN_POINT('Ctrl Pts',(-0.765547441878935,0.239023132968793,
-2.1828159149676));
#49196=CARTESIAN_POINT('Ctrl Pts',(-0.783631512222635,0.10893956889734,
-2.17753007810896));
#49197=CARTESIAN_POINT('Ctrl Pts',(-0.788645813927934,0.0728703530207205,
-2.17606443568054));
#49198=CARTESIAN_POINT('Ctrl Pts',(-0.791116097488508,0.036447470611259,
-2.17459879325212));
#49199=CARTESIAN_POINT('Ctrl Pts',(-0.791081243560257,1.98986687146829E-5,
-2.1731331508237));
#49200=CARTESIAN_POINT('Origin',(0.,0.,-2.94));
#49201=CARTESIAN_POINT('',(-0.791132802071856,-1.71669250316198E-5,-1.94466684917629));
#49202=CARTESIAN_POINT('',(-0.791147029519077,-1.37720429744394E-5,-1.9731331508237));
#49203=CARTESIAN_POINT('',(-0.7911,-9.68818082805471E-17,-2.94));
#49204=CARTESIAN_POINT('Ctrl Pts',(-0.791132802071856,-1.71669250316198E-5,
-1.94466684917629));
#49205=CARTESIAN_POINT('Ctrl Pts',(-0.791026522766624,0.111615095251917,
-1.94915915229662));
#49206=CARTESIAN_POINT('Ctrl Pts',(-0.767167347256203,0.223291341687766,
-1.95365145541694));
#49207=CARTESIAN_POINT('Ctrl Pts',(-0.721308735469413,0.32505366763991,
-1.95814375853727));
#49208=CARTESIAN_POINT('Ctrl Pts',(-0.667349522572057,0.444791592470935,
-1.96342959539592));
#49209=CARTESIAN_POINT('Ctrl Pts',(-0.582932339520027,0.550803806769426,
-1.96871543225456));
#49210=CARTESIAN_POINT('Ctrl Pts',(-0.47831772068937,0.630204995842756,
-1.97400126911321));
#49211=CARTESIAN_POINT('Ctrl Pts',(-0.373703101858712,0.709606184916085,
-1.97928710597186));
#49212=CARTESIAN_POINT('Ctrl Pts',(-0.248891047249423,0.762396348764255,
-1.98457294283051));
#49213=CARTESIAN_POINT('Ctrl Pts',(-0.119051908803644,0.782159076991918,
-1.98985877968915));
#49214=CARTESIAN_POINT('Ctrl Pts',(0.0107872296421378,0.801921805219581,
-1.9951446165478));
#49215=CARTESIAN_POINT('Ctrl Pts',(0.145653451924402,0.788657097826737,
-2.00043045340645));
#49216=CARTESIAN_POINT('Ctrl Pts',(0.269154366590807,0.743977221194132,
-2.0057162902651));
#49217=CARTESIAN_POINT('Ctrl Pts',(0.392655281257209,0.699297344561529,
-2.01100212712375));
#49218=CARTESIAN_POINT('Ctrl Pts',(0.504790888307744,0.623202298689167,
-2.01628796398239));
#49219=CARTESIAN_POINT('Ctrl Pts',(0.591931601805962,0.524941099071189,
-2.02157380084104));
#49220=CARTESIAN_POINT('Ctrl Pts',(0.67907231530418,0.426679899453212,-2.02685963769969));
#49221=CARTESIAN_POINT('Ctrl Pts',(0.741218135250083,0.306252546089617,
-2.03214547455834));
#49222=CARTESIAN_POINT('Ctrl Pts',(0.770815512723548,0.178296449923644,
-2.03743131141698));
#49223=CARTESIAN_POINT('Ctrl Pts',(0.800412890197013,0.0503403537576715,
-2.04271714827563));
#49224=CARTESIAN_POINT('Ctrl Pts',(0.797461825198041,-0.0851444852106823,
-2.04800298513428));
#49225=CARTESIAN_POINT('Ctrl Pts',(0.762321006595096,-0.211690485413207,
-2.05328882199293));
#49226=CARTESIAN_POINT('Ctrl Pts',(0.727180187992152,-0.338236485615732,
-2.05857465885158));
#49227=CARTESIAN_POINT('Ctrl Pts',(0.659849615785234,-0.455843647052432,
-2.06386049571022));
#49228=CARTESIAN_POINT('Ctrl Pts',(0.568513022547629,-0.550217340606783,
-2.06914633256887));
#49229=CARTESIAN_POINT('Ctrl Pts',(0.477176429310023,-0.644591034161134,
-2.07443216942752));
#49230=CARTESIAN_POINT('Ctrl Pts',(0.361833815041726,-0.715731259833139,
-2.07971800628617));
#49231=CARTESIAN_POINT('Ctrl Pts',(0.236504563189749,-0.754991238559142,
-2.08500384314482));
#49232=CARTESIAN_POINT('Ctrl Pts',(0.111175311337768,-0.794251217285145,
-2.09028968000346));
#49233=CARTESIAN_POINT('Ctrl Pts',(-0.0241405780978863,-0.801630949065144,
-2.09557551686211));
#49234=CARTESIAN_POINT('Ctrl Pts',(-0.152996058615766,-0.776233460215857,
-2.10086135372076));
#49235=CARTESIAN_POINT('Ctrl Pts',(-0.281851539133642,-0.75083597136657,
-2.10614719057941));
#49236=CARTESIAN_POINT('Ctrl Pts',(-0.404246610733737,-0.692661261887995,
-2.11143302743805));
#49237=CARTESIAN_POINT('Ctrl Pts',(-0.505304695044117,-0.608780209827005,
-2.1167188642967));
#49238=CARTESIAN_POINT('Ctrl Pts',(-0.606362779354498,-0.524899157766015,
-2.12200470115535));
#49239=CARTESIAN_POINT('Ctrl Pts',(-0.686083876375167,-0.415311763122608,
-2.127290538014));
#49240=CARTESIAN_POINT('Ctrl Pts',(-0.734778240169299,-0.293337887911449,
-2.13257637487265));
#49241=CARTESIAN_POINT('Ctrl Pts',(-0.771904997951733,-0.200339557757781,
-2.13660653297386));
#49242=CARTESIAN_POINT('Ctrl Pts',(-0.790995237347112,-0.10014069563447,
-2.14063669107508));
#49243=CARTESIAN_POINT('Ctrl Pts',(-0.791097165546451,2.04205267731045E-5,
-2.14466684917629));
#49244=CARTESIAN_POINT('Ctrl Pts',(-0.791081243560257,1.98986687146829E-5,
-2.1731331508237));
#49245=CARTESIAN_POINT('Ctrl Pts',(-0.790990396857139,-0.0949285039861595,
-2.16931295639347));
#49246=CARTESIAN_POINT('Ctrl Pts',(-0.773880064045768,-0.189908766546335,
-2.16549276196324));
#49247=CARTESIAN_POINT('Ctrl Pts',(-0.740438748222271,-0.278741164435588,
-2.16167256753301));
#49248=CARTESIAN_POINT('Ctrl Pts',(-0.694167454179532,-0.401654689278622,
-2.15638673067437));
#49249=CARTESIAN_POINT('Ctrl Pts',(-0.61663040639538,-0.512798094546253,
-2.15110089381572));
#49250=CARTESIAN_POINT('Ctrl Pts',(-0.517251889303895,-0.598662392030284,
-2.14581505695707));
#49251=CARTESIAN_POINT('Ctrl Pts',(-0.41787337221241,-0.684526689514316,
-2.14052922009842));
#49252=CARTESIAN_POINT('Ctrl Pts',(-0.296653385813593,-0.745111879214747,
-2.13524338323977));
#49253=CARTESIAN_POINT('Ctrl Pts',(-0.168325682082346,-0.773054099899473,
-2.12995754638113));
#49254=CARTESIAN_POINT('Ctrl Pts',(-0.0399979783510983,-0.800996320584199,
-2.12467170952248));
#49255=CARTESIAN_POINT('Ctrl Pts',(0.095437442712579,-0.79629557225322,
-2.11938587266383));
#49256=CARTESIAN_POINT('Ctrl Pts',(0.221519006067722,-0.759523210027606,
-2.11410003580518));
#49257=CARTESIAN_POINT('Ctrl Pts',(0.347600569422865,-0.722750847801993,
-2.10881419894653));
#49258=CARTESIAN_POINT('Ctrl Pts',(0.464328275069475,-0.653906871681745,
-2.10352836208789));
#49259=CARTESIAN_POINT('Ctrl Pts',(0.557514387843661,-0.561358961776846,
-2.09824252522924));
#49260=CARTESIAN_POINT('Ctrl Pts',(0.650700500617848,-0.468811051871947,
-2.09295668837059));
#49261=CARTESIAN_POINT('Ctrl Pts',(0.720345020519613,-0.352559208182397,
-2.08767085151194));
#49262=CARTESIAN_POINT('Ctrl Pts',(0.757982964891162,-0.226733326960715,
-2.08238501465329));
#49263=CARTESIAN_POINT('Ctrl Pts',(0.795620909262712,-0.100907445739033,
-2.07709917779465));
#49264=CARTESIAN_POINT('Ctrl Pts',(0.801252278104046,0.0344924730147816,
-2.071813340936));
#49265=CARTESIAN_POINT('Ctrl Pts',(0.774192603496531,0.163009169408146,
-2.06652750407735));
#49266=CARTESIAN_POINT('Ctrl Pts',(0.747132928889016,0.29152586580151,-2.0612416672187));
#49267=CARTESIAN_POINT('Ctrl Pts',(0.687382210832651,0.413159339834423,
-2.05595583036006));
#49268=CARTESIAN_POINT('Ctrl Pts',(0.602202884230443,0.513125581943063,
-2.05066999350141));
#49269=CARTESIAN_POINT('Ctrl Pts',(0.517023557628235,0.613091824051702,
-2.04538415664276));
#49270=CARTESIAN_POINT('Ctrl Pts',(0.406415622480184,0.691390834236067,
-2.04009831978411));
#49271=CARTESIAN_POINT('Ctrl Pts',(0.283822982975207,0.738505714910133,
-2.03481248292547));
#49272=CARTESIAN_POINT('Ctrl Pts',(0.16123034347023,0.785620595584199,-2.02952664606682));
#49273=CARTESIAN_POINT('Ctrl Pts',(0.0266529996083376,0.801551346747966,
-2.02424080920817));
#49274=CARTESIAN_POINT('Ctrl Pts',(-0.103551769049521,0.784361656218983,
-2.01895497234952));
#49275=CARTESIAN_POINT('Ctrl Pts',(-0.233756537707379,0.76717196569,-2.01366913549088));
#49276=CARTESIAN_POINT('Ctrl Pts',(-0.359588731161204,0.716861833468259,
-2.00838329863223));
#49277=CARTESIAN_POINT('Ctrl Pts',(-0.46575400411459,0.639546233098982,
-2.00309746177358));
#49278=CARTESIAN_POINT('Ctrl Pts',(-0.571919277067976,0.562230632729704,
-1.99781162491493));
#49279=CARTESIAN_POINT('Ctrl Pts',(-0.658417629520933,0.457909564212886,
-1.99252578805628));
#49280=CARTESIAN_POINT('Ctrl Pts',(-0.714735570182623,0.339262790968288,
-1.98723995119764));
#49281=CARTESIAN_POINT('Ctrl Pts',(-0.764835864461531,0.233714928511718,
-1.98253768440632));
#49282=CARTESIAN_POINT('Ctrl Pts',(-0.791051877136207,0.116829938905797,
-1.97783541761501));
#49283=CARTESIAN_POINT('Ctrl Pts',(-0.791147029519077,-1.37720429744394E-5,
-1.9731331508237));
#49284=CARTESIAN_POINT('Origin',(0.,0.,-2.94));
#49285=CARTESIAN_POINT('',(-0.79103421667841,4.57183632199265E-6,-1.74466684917629));
#49286=CARTESIAN_POINT('',(-0.791032665677869,-2.33805119084811E-7,-1.7731331508237));
#49287=CARTESIAN_POINT('',(-0.7911,-9.68818082805471E-17,-2.94));
#49288=CARTESIAN_POINT('Ctrl Pts',(-0.79103421667841,4.57183632199265E-6,
-1.74466684917629));
#49289=CARTESIAN_POINT('Ctrl Pts',(-0.791046491980383,0.0607363198089551,
-1.74710993980086));
#49290=CARTESIAN_POINT('Ctrl Pts',(-0.784141006924924,0.121465321068842,
-1.74955303042543));
#49291=CARTESIAN_POINT('Ctrl Pts',(-0.770287134004301,0.18056552798937,
-1.75199612105));
#49292=CARTESIAN_POINT('Ctrl Pts',(-0.740313087449333,0.30843391279368,
-1.75728195790865));
#49293=CARTESIAN_POINT('Ctrl Pts',(-0.677812909732563,0.42867774074456,
-1.7625677947673));
#49294=CARTESIAN_POINT('Ctrl Pts',(-0.590383220390283,0.526681907599112,
-1.76785363162595));
#49295=CARTESIAN_POINT('Ctrl Pts',(-0.502953531048003,0.624686074453665,
-1.77313946848459));
#49296=CARTESIAN_POINT('Ctrl Pts',(-0.390594330080212,0.70045058021189,
-1.77842530534324));
#49297=CARTESIAN_POINT('Ctrl Pts',(-0.266962380272803,0.744766585065227,
-1.78371114220189));
#49298=CARTESIAN_POINT('Ctrl Pts',(-0.143330430465394,0.789082589918563,
-1.78899697906054));
#49299=CARTESIAN_POINT('Ctrl Pts',(-0.00842573181836657,0.801950093867011,
-1.79428281591919));
#49300=CARTESIAN_POINT('Ctrl Pts',(0.12135464758435,0.781805108847671,-1.79956865277783));
#49301=CARTESIAN_POINT('Ctrl Pts',(0.251135026987067,0.761660123828331,
-1.80485448963648));
#49302=CARTESIAN_POINT('Ctrl Pts',(0.375791087145474,0.708502649841203,
-1.81014032649513));
#49303=CARTESIAN_POINT('Ctrl Pts',(0.480171436551409,0.628793742200729,
-1.81542616335378));
#49304=CARTESIAN_POINT('Ctrl Pts',(0.584551785957344,0.549084834560255,
-1.82071200021242));
#49305=CARTESIAN_POINT('Ctrl Pts',(0.668656424610807,0.442824493266436,
-1.82599783707107));
#49306=CARTESIAN_POINT('Ctrl Pts',(0.722262806521882,0.322928191748221,
-1.83128367392972));
#49307=CARTESIAN_POINT('Ctrl Pts',(0.775869188432956,0.203031890230006,
-1.83656951078837));
#49308=CARTESIAN_POINT('Ctrl Pts',(0.798977313601642,0.0694996284873965,
-1.84185534764702));
#49309=CARTESIAN_POINT('Ctrl Pts',(0.788778491852706,-0.0614383390173576,
-1.84714118450566));
#49310=CARTESIAN_POINT('Ctrl Pts',(0.778579670103769,-0.192376306522112,
-1.85242702136431));
#49311=CARTESIAN_POINT('Ctrl Pts',(0.73507390143721,-0.32071997978901,-1.85771285822296));
#49312=CARTESIAN_POINT('Ctrl Pts',(0.663549119172057,-0.430869754283854,
-1.86299869508161));
#49313=CARTESIAN_POINT('Ctrl Pts',(0.592024336906903,-0.541019528778699,
-1.86828453194025));
#49314=CARTESIAN_POINT('Ctrl Pts',(0.492480541043156,-0.632975404501489,
-1.8735703687989));
#49315=CARTESIAN_POINT('Ctrl Pts',(0.37701683868739,-0.695560552401304,
-1.87885620565755));
#49316=CARTESIAN_POINT('Ctrl Pts',(0.261553136331624,-0.758145700301119,
-1.8841420425162));
#49317=CARTESIAN_POINT('Ctrl Pts',(0.130169527483839,-0.791360120377959,
-1.88942787937485));
#49318=CARTESIAN_POINT('Ctrl Pts',(-0.00116489262803629,-0.791166747112014,
-1.89471371623349));
#49319=CARTESIAN_POINT('Ctrl Pts',(-0.132499312739904,-0.79097337384607,
-1.89999955309214));
#49320=CARTESIAN_POINT('Ctrl Pts',(-0.263784544115863,-0.757372207237345,
-1.90528538995079));
#49321=CARTESIAN_POINT('Ctrl Pts',(-0.379063448873576,-0.69444732013214,
-1.91057122680944));
#49322=CARTESIAN_POINT('Ctrl Pts',(-0.494342353631296,-0.631522433026931,
-1.91585706366809));
#49323=CARTESIAN_POINT('Ctrl Pts',(-0.593614931770767,-0.539273825425238,
-1.92114290052673));
#49324=CARTESIAN_POINT('Ctrl Pts',(-0.664815041497486,-0.428913906640175,
-1.92642873738538));
#49325=CARTESIAN_POINT('Ctrl Pts',(-0.736015151224201,-0.318553987855117,
-1.93171457424403));
#49326=CARTESIAN_POINT('Ctrl Pts',(-0.779142792538166,-0.190082757886691,
-1.93700041110267));
#49327=CARTESIAN_POINT('Ctrl Pts',(-0.78895599182381,-0.0591153252206997,
-1.94228624796132));
#49328=CARTESIAN_POINT('Ctrl Pts',(-0.790429193688017,-0.0394539018318772,
-1.94307978169965));
#49329=CARTESIAN_POINT('Ctrl Pts',(-0.791151575563343,-0.0197362205930797,
-1.94387331543797));
#49330=CARTESIAN_POINT('Ctrl Pts',(-0.791132802071856,-1.71669250316198E-5,
-1.94466684917629));
#49331=CARTESIAN_POINT('Ctrl Pts',(-0.791147029519077,-1.37720429744394E-5,
-1.9731331508237));
#49332=CARTESIAN_POINT('Ctrl Pts',(-0.791158838309378,-0.0145145426908869,
-1.97254958075636));
#49333=CARTESIAN_POINT('Ctrl Pts',(-0.790768338829755,-0.0290146775731718,
-1.97196601068903));
#49334=CARTESIAN_POINT('Ctrl Pts',(-0.789971256028148,-0.043492427722329,
-1.97138244062169));
#49335=CARTESIAN_POINT('Ctrl Pts',(-0.78275147234156,-0.174628395195968,
-1.96609660376304));
#49336=CARTESIAN_POINT('Ctrl Pts',(-0.742174376097962,-0.303927852170872,
-1.9608107669044));
#49337=CARTESIAN_POINT('Ctrl Pts',(-0.673171933466268,-0.415675022840148,
-1.95552493004575));
#49338=CARTESIAN_POINT('Ctrl Pts',(-0.604169490834576,-0.52742219350942,
-1.9502390931871));
#49339=CARTESIAN_POINT('Ctrl Pts',(-0.506741701814794,-0.621617077873063,
-1.94495325632845));
#49340=CARTESIAN_POINT('Ctrl Pts',(-0.392730482261924,-0.686810705305464,
-1.93966741946981));
#49341=CARTESIAN_POINT('Ctrl Pts',(-0.27871926270905,-0.752004332737866,
-1.93438158261116));
#49342=CARTESIAN_POINT('Ctrl Pts',(-0.14812461262309,-0.788196703239019,
-1.92909574575251));
#49343=CARTESIAN_POINT('Ctrl Pts',(-0.0168197327919539,-0.790988794616383,
-1.92380990889386));
#49344=CARTESIAN_POINT('Ctrl Pts',(0.114485147039182,-0.793780885993746,
-1.91852407203521));
#49345=CARTESIAN_POINT('Ctrl Pts',(0.246500256615497,-0.763172698247319,
-1.91323823517657));
#49346=CARTESIAN_POINT('Ctrl Pts',(0.363179744594969,-0.702884520910657,
-1.90795239831792));
#49347=CARTESIAN_POINT('Ctrl Pts',(0.479859232574441,-0.642596343573996,
-1.90266656145927));
#49348=CARTESIAN_POINT('Ctrl Pts',(0.581203098957073,-0.552628176647096,
-1.89738072460062));
#49349=CARTESIAN_POINT('Ctrl Pts',(0.654893446044485,-0.443915251988317,
-1.89209488774197));
#49350=CARTESIAN_POINT('Ctrl Pts',(0.728583793131896,-0.335202327329538,
-1.88680905088333));
#49351=CARTESIAN_POINT('Ctrl Pts',(0.774620620924088,-0.207744644938874,
-1.88152321402468));
#49352=CARTESIAN_POINT('Ctrl Pts',(0.787408357085573,-0.0770341210871483,
-1.87623737716603));
#49353=CARTESIAN_POINT('Ctrl Pts',(0.800196093247058,0.0536764027645815,
-1.87095154030738));
#49354=CARTESIAN_POINT('Ctrl Pts',(0.779734737777836,0.18763976807737,-1.86566570344874));
#49355=CARTESIAN_POINT('Ctrl Pts',(0.72851127772938,0.308573321661119,-1.86037986659009));
#49356=CARTESIAN_POINT('Ctrl Pts',(0.677287817680926,0.429506875244866,
-1.85509402973144));
#49357=CARTESIAN_POINT('Ctrl Pts',(0.595302253053237,0.537410617099569,
-1.84980819287279));
#49358=CARTESIAN_POINT('Ctrl Pts',(0.492519565782321,0.619169325743342,
-1.84452235601415));
#49359=CARTESIAN_POINT('Ctrl Pts',(0.389736878511398,0.700928034387121,
-1.8392365191555));
#49360=CARTESIAN_POINT('Ctrl Pts',(0.266157068597242,0.75654170981997,-1.83395068229685));
#49361=CARTESIAN_POINT('Ctrl Pts',(0.13680071410188,0.779250756330134,-1.8286648454382));
#49362=CARTESIAN_POINT('Ctrl Pts',(0.00744435960653334,0.801959802840296,
-1.82337900857955));
#49363=CARTESIAN_POINT('Ctrl Pts',(-0.127688539470023,0.79176422042778,
-1.81809317172091));
#49364=CARTESIAN_POINT('Ctrl Pts',(-0.252173178293266,0.749903236937503,
-1.81280733486226));
#49365=CARTESIAN_POINT('Ctrl Pts',(-0.376657817116519,0.708042253447222,
-1.80752149800361));
#49366=CARTESIAN_POINT('Ctrl Pts',(-0.490494195686453,0.634515868879179,
-1.80223566114496));
#49367=CARTESIAN_POINT('Ctrl Pts',(-0.579846006828024,0.53826088933292,
-1.79694982428631));
#49368=CARTESIAN_POINT('Ctrl Pts',(-0.669197817969591,0.442005909786664,
-1.79166398742767));
#49369=CARTESIAN_POINT('Ctrl Pts',(-0.73406506168279,0.323022335262195,
-1.78637815056902));
#49370=CARTESIAN_POINT('Ctrl Pts',(-0.766563412052733,0.195772091785175,
-1.78109231371037));
#49371=CARTESIAN_POINT('Ctrl Pts',(-0.782874904509492,0.131902961107212,
-1.77843925941482));
#49372=CARTESIAN_POINT('Ctrl Pts',(-0.791031985578626,0.0659512810282034,
-1.77578620511926));
#49373=CARTESIAN_POINT('Ctrl Pts',(-0.791032665677869,-2.33805119084811E-7,
-1.7731331508237));
#49374=CARTESIAN_POINT('Origin',(0.,0.,-2.94));
#49375=CARTESIAN_POINT('',(-0.791157484722713,9.84224722326565E-6,-1.54466684917629));
#49376=CARTESIAN_POINT('',(-0.791145759608552,1.41466495050277E-5,-1.5731331508237));
#49377=CARTESIAN_POINT('',(-0.7911,-9.68818082805471E-17,-2.94));
#49378=CARTESIAN_POINT('Ctrl Pts',(-0.791157484722713,9.84224722326565E-6,
-1.54466684917629));
#49379=CARTESIAN_POINT('Ctrl Pts',(-0.791163583645489,0.0097967005803917,
-1.54506072730511));
#49380=CARTESIAN_POINT('Ctrl Pts',(-0.790985743924691,0.0195833369757562,
-1.54545460543392));
#49381=CARTESIAN_POINT('Ctrl Pts',(-0.7906225317606,0.0293630887867682,
-1.54584848356274));
#49382=CARTESIAN_POINT('Ctrl Pts',(-0.785748231554505,0.160607168641227,
-1.55113432042139));
#49383=CARTESIAN_POINT('Ctrl Pts',(-0.747489118033617,0.290611363217802,
-1.55642015728003));
#49384=CARTESIAN_POINT('Ctrl Pts',(-0.680495416842589,0.403574238978249,
-1.56170599413868));
#49385=CARTESIAN_POINT('Ctrl Pts',(-0.61350171565156,0.516537114738695,
-1.56699183099733));
#49386=CARTESIAN_POINT('Ctrl Pts',(-0.517773426790394,0.612458671683009,
-1.57227766785598));
#49387=CARTESIAN_POINT('Ctrl Pts',(-0.404945899403756,0.679680069787782,
-1.57756350471462));
#49388=CARTESIAN_POINT('Ctrl Pts',(-0.292118372017125,0.74690146789255,
-1.58284934157327));
#49389=CARTESIAN_POINT('Ctrl Pts',(-0.162191606105027,0.785422707157778,
-1.58813517843192));
#49390=CARTESIAN_POINT('Ctrl Pts',(-0.0309576240947823,0.7905617017166,
-1.59342101529057));
#49391=CARTESIAN_POINT('Ctrl Pts',(0.100276357915478,0.795700696275423,
-1.59870685214922));
#49392=CARTESIAN_POINT('Ctrl Pts',(0.232817556023881,0.767457446127832,
-1.60399268900786));
#49393=CARTESIAN_POINT('Ctrl Pts',(0.350556175159501,0.709264793126081,
-1.60927852586651));
#49394=CARTESIAN_POINT('Ctrl Pts',(0.468294794295108,0.651072140124337,
-1.61456436272516));
#49395=CARTESIAN_POINT('Ctrl Pts',(0.571230834457931,0.562930084268443,
-1.61985019958381));
#49396=CARTESIAN_POINT('Ctrl Pts',(0.646852876284771,0.455551901711275,
-1.62513603644245));
#49397=CARTESIAN_POINT('Ctrl Pts',(0.72247491811162,0.348173719154094,-1.6304218733011));
#49398=CARTESIAN_POINT('Ctrl Pts',(0.770782961602475,0.221559409895639,
-1.63570771015975));
#49399=CARTESIAN_POINT('Ctrl Pts',(0.785905378222046,0.0910983819411992,
-1.6409935470184));
#49400=CARTESIAN_POINT('Ctrl Pts',(0.801027794841615,-0.0393626460132327,
-1.64627938387705));
#49401=CARTESIAN_POINT('Ctrl Pts',(0.782964584589898,-0.173670392663664,
-1.6515652207357));
#49402=CARTESIAN_POINT('Ctrl Pts',(0.733911250598238,-0.295500346795009,
-1.65685105759434));
#49403=CARTESIAN_POINT('Ctrl Pts',(0.684857916606581,-0.417330300926347,
-1.66213689445299));
#49404=CARTESIAN_POINT('Ctrl Pts',(0.604814458874985,-0.526682462538616,
-1.66742273131164));
#49405=CARTESIAN_POINT('Ctrl Pts',(0.503509804855647,-0.610265561149299,
-1.67270856817029));
#49406=CARTESIAN_POINT('Ctrl Pts',(0.402205150836304,-0.693848659759987,
-1.67799440502893));
#49407=CARTESIAN_POINT('Ctrl Pts',(0.279639300529219,-0.751662695369081,
-1.68328024188758));
#49408=CARTESIAN_POINT('Ctrl Pts',(0.150709589701088,-0.776680628239671,
-1.68856607874623));
#49409=CARTESIAN_POINT('Ctrl Pts',(0.021779878872957,-0.801698561110261,
-1.69385191560488));
#49410=CARTESIAN_POINT('Ctrl Pts',(-0.113513692476217,-0.793920391242345,
-1.69913775246353));
#49411=CARTESIAN_POINT('Ctrl Pts',(-0.238726790509447,-0.754291520702506,
-1.70442358932217));
#49412=CARTESIAN_POINT('Ctrl Pts',(-0.363939888542678,-0.714662650162667,
-1.70970942618082));
#49413=CARTESIAN_POINT('Ctrl Pts',(-0.479072513259962,-0.643183078950906,
-1.71499526303947));
#49414=CARTESIAN_POINT('Ctrl Pts',(-0.570130804513331,-0.548540832076904,
-1.72028109989812));
#49415=CARTESIAN_POINT('Ctrl Pts',(-0.6611890957667,-0.453898585202903,
-1.72556693675676));
#49416=CARTESIAN_POINT('Ctrl Pts',(-0.728173053556152,-0.336093662666664,
-1.73085277361541));
#49417=CARTESIAN_POINT('Ctrl Pts',(-0.762941074754295,-0.209444730569673,
-1.73613861047406));
#49418=CARTESIAN_POINT('Ctrl Pts',(-0.781639468967064,-0.141332379697595,
-1.73898135670814));
#49419=CARTESIAN_POINT('Ctrl Pts',(-0.79101993330795,-0.070662044498731,
-1.74182410294222));
#49420=CARTESIAN_POINT('Ctrl Pts',(-0.79103421667841,4.57183632199265E-6,
-1.74466684917629));
#49421=CARTESIAN_POINT('Ctrl Pts',(-0.791032665677869,-2.33805119084811E-7,
-1.7731331508237));
#49422=CARTESIAN_POINT('Ctrl Pts',(-0.791033340580539,-0.0654478194626728,
-1.77050036826061));
#49423=CARTESIAN_POINT('Ctrl Pts',(-0.783001782864027,-0.130895242390146,
-1.76786758569752));
#49424=CARTESIAN_POINT('Ctrl Pts',(-0.766936048205097,-0.194307165548313,
-1.76523480313443));
#49425=CARTESIAN_POINT('Ctrl Pts',(-0.734680876960827,-0.321619266975207,
-1.75994896627578));
#49426=CARTESIAN_POINT('Ctrl Pts',(-0.670041077445598,-0.440726557399418,
-1.75466312941713));
#49427=CARTESIAN_POINT('Ctrl Pts',(-0.580873330740293,-0.537152073676115,
-1.74937729255848));
#49428=CARTESIAN_POINT('Ctrl Pts',(-0.491705584034995,-0.633577589952803,
-1.74409145569984));
#49429=CARTESIAN_POINT('Ctrl Pts',(-0.378009890139618,-0.707321332081983,
-1.73880561884119));
#49430=CARTESIAN_POINT('Ctrl Pts',(-0.253605456630702,-0.749420075116088,
-1.73351978198254));
#49431=CARTESIAN_POINT('Ctrl Pts',(-0.129201023121776,-0.791518818150198,
-1.72823394512389));
#49432=CARTESIAN_POINT('Ctrl Pts',(0.005912150000697,-0.801972562089233,
-1.72294810826524));
#49433=CARTESIAN_POINT('Ctrl Pts',(0.135311655504476,-0.779510700699169,
-1.7176622714066));
#49434=CARTESIAN_POINT('Ctrl Pts',(0.264711161008255,-0.757048839309105,
-1.71237643454795));
#49435=CARTESIAN_POINT('Ctrl Pts',(0.388396998893335,-0.701671372589941,
-1.7070905976893));
#49436=CARTESIAN_POINT('Ctrl Pts',(0.491335703867856,-0.620109186131402,
-1.70180476083066));
#49437=CARTESIAN_POINT('Ctrl Pts',(0.594274408842377,-0.538546999672864,
-1.69651892397201));
#49438=CARTESIAN_POINT('Ctrl Pts',(0.676465980906336,-0.430800093474953,
-1.69123308711336));
#49439=CARTESIAN_POINT('Ctrl Pts',(0.727920398833092,-0.309964626340722,
-1.68594725025471));
#49440=CARTESIAN_POINT('Ctrl Pts',(0.779374816759847,-0.189129159206491,
-1.68066141339606));
#49441=CARTESIAN_POINT('Ctrl Pts',(0.800092080549398,-0.0552051311359448,
-1.67537557653742));
#49442=CARTESIAN_POINT('Ctrl Pts',(0.787554098628381,0.0755295859482219,
-1.67008973967877));
#49443=CARTESIAN_POINT('Ctrl Pts',(0.775016116707365,0.206264303032389,
-1.66480390282012));
#49444=CARTESIAN_POINT('Ctrl Pts',(0.729222889075781,0.333809709130172,
-1.65951806596147));
#49445=CARTESIAN_POINT('Ctrl Pts',(0.655740379549484,0.44266322554304,-1.65423222910282));
#49446=CARTESIAN_POINT('Ctrl Pts',(0.582257870023187,0.551516741955908,
-1.64894639224418));
#49447=CARTESIAN_POINT('Ctrl Pts',(0.481086078602161,0.641678368683872,
-1.64366055538553));
#49448=CARTESIAN_POINT('Ctrl Pts',(0.364521988036041,0.702189359687345,
-1.63837471852688));
#49449=CARTESIAN_POINT('Ctrl Pts',(0.247957897469928,0.762700350690814,
-1.63308888166823));
#49450=CARTESIAN_POINT('Ctrl Pts',(0.116001507758712,0.79356070596981,-1.62780304480958));
#49451=CARTESIAN_POINT('Ctrl Pts',(-0.015308466894889,0.791019486145062,
-1.62251720795094));
#49452=CARTESIAN_POINT('Ctrl Pts',(-0.146618441548498,0.788478266320315,
-1.61723137109229));
#49453=CARTESIAN_POINT('Ctrl Pts',(-0.277282001144486,0.752535471391821,
-1.61194553423364));
#49454=CARTESIAN_POINT('Ctrl Pts',(-0.391417569249487,0.687559788747637,
-1.60665969737499));
#49455=CARTESIAN_POINT('Ctrl Pts',(-0.505553137354487,0.622584106103453,
-1.60137386051635));
#49456=CARTESIAN_POINT('Ctrl Pts',(-0.603160713968495,0.528575535743582,
-1.5960880236577));
#49457=CARTESIAN_POINT('Ctrl Pts',(-0.672376530851428,0.416960402652422,
-1.59080218679905));
#49458=CARTESIAN_POINT('Ctrl Pts',(-0.74159234773436,0.305345269561261,
-1.5855163499404));
#49459=CARTESIAN_POINT('Ctrl Pts',(-0.782416404886214,0.176123573738817,
-1.58023051308176));
#49460=CARTESIAN_POINT('Ctrl Pts',(-0.789886719134465,0.0450016394686068,
-1.57494467622311));
#49461=CARTESIAN_POINT('Ctrl Pts',(-0.790740110588152,0.0300225724068191,
-1.5743408344233));
#49462=CARTESIAN_POINT('Ctrl Pts',(-0.791158227354029,0.0150187067579734,
-1.5737369926235));
#49463=CARTESIAN_POINT('Ctrl Pts',(-0.791145759608552,1.41466495050277E-5,
-1.5731331508237));
#49464=CARTESIAN_POINT('Origin',(0.,0.,-2.94));
#49465=CARTESIAN_POINT('',(-0.791067994997204,-1.8415035504149E-5,-1.3446668491763));
#49466=CARTESIAN_POINT('',(-0.791082733992286,-2.00018711214563E-5,-1.3731331508237));
#49467=CARTESIAN_POINT('',(-0.7911,-9.68818082805471E-17,-2.94));
#49468=CARTESIAN_POINT('Ctrl Pts',(-0.791067994997204,-1.8415035504149E-5,
-1.3446668491763));
#49469=CARTESIAN_POINT('Ctrl Pts',(-0.790990174960068,0.0902196588333193,
-1.348297351668));
#49470=CARTESIAN_POINT('Ctrl Pts',(-0.775570000219954,0.180483650617083,
-1.35192785415971));
#49471=CARTESIAN_POINT('Ctrl Pts',(-0.745303502796337,0.265459728452642,
-1.35555835665142));
#49472=CARTESIAN_POINT('Ctrl Pts',(-0.701236939550792,0.389180807105671,
-1.36084419351007));
#49473=CARTESIAN_POINT('Ctrl Pts',(-0.625699203521556,0.50169258786878,
-1.36613003036871));
#49474=CARTESIAN_POINT('Ctrl Pts',(-0.527871571661909,0.589319762558348,
-1.37141586722736));
#49475=CARTESIAN_POINT('Ctrl Pts',(-0.430043939802261,0.676946937247915,
-1.37670170408601));
#49476=CARTESIAN_POINT('Ctrl Pts',(-0.309926412112203,0.73968950586394,
-1.38198754094466));
#49477=CARTESIAN_POINT('Ctrl Pts',(-0.18211874159782,0.769921387330854,
-1.3872733778033));
#49478=CARTESIAN_POINT('Ctrl Pts',(-0.0543110710834368,0.800153268797768,
-1.39255921466195));
#49479=CARTESIAN_POINT('Ctrl Pts',(0.0811867422552711,0.79787446311557,
-1.3978450515206));
#49480=CARTESIAN_POINT('Ctrl Pts',(0.207905539872897,0.763361949012918,
-1.40313088837925));
#49481=CARTESIAN_POINT('Ctrl Pts',(0.334624337490523,0.728849434910265,
-1.4084167252379));
#49482=CARTESIAN_POINT('Ctrl Pts',(0.452564119387066,0.662103212387157,
-1.41370256209654));
#49483=CARTESIAN_POINT('Ctrl Pts',(0.547389827903631,0.57123598890325,-1.41898839895519));
#49484=CARTESIAN_POINT('Ctrl Pts',(0.642215536420195,0.480368765419343,
-1.42427423581384));
#49485=CARTESIAN_POINT('Ctrl Pts',(0.71392717155678,0.365380540974639,-1.42956007267249));
#49486=CARTESIAN_POINT('Ctrl Pts',(0.753808501962385,0.240247624504105,
-1.43484590953113));
#49487=CARTESIAN_POINT('Ctrl Pts',(0.793689832367991,0.115114708033571,
-1.44013174638978));
#49488=CARTESIAN_POINT('Ctrl Pts',(0.801740858042617,-0.0201629004627912,
-1.44541758324843));
#49489=CARTESIAN_POINT('Ctrl Pts',(0.776983012505953,-0.149142807361987,
-1.45070342010708));
#49490=CARTESIAN_POINT('Ctrl Pts',(0.75222516696929,-0.278122714261184,
-1.45598925696573));
#49491=CARTESIAN_POINT('Ctrl Pts',(0.694658450221336,-0.400804919563214,
-1.46127509382437));
#49492=CARTESIAN_POINT('Ctrl Pts',(0.611279841487808,-0.502277945067551,
-1.46656093068302));
#49493=CARTESIAN_POINT('Ctrl Pts',(0.527901232754279,-0.603750970571887,
-1.47184676754167));
#49494=CARTESIAN_POINT('Ctrl Pts',(0.418710732035175,-0.68401481627853,
-1.47713260440032));
#49495=CARTESIAN_POINT('Ctrl Pts',(0.296979960648103,-0.733313767553898,
-1.48241844125897));
#49496=CARTESIAN_POINT('Ctrl Pts',(0.175249189261031,-0.782612718829265,
-1.48770427811761));
#49497=CARTESIAN_POINT('Ctrl Pts',(0.0409781472059913,-0.800946775673357,
-1.49299011497626));
#49498=CARTESIAN_POINT('Ctrl Pts',(-0.0895131155828244,-0.786087514752204,
-1.49827595183491));
#49499=CARTESIAN_POINT('Ctrl Pts',(-0.22000437837164,-0.771228253831051,
-1.50356178869356));
#49500=CARTESIAN_POINT('Ctrl Pts',(-0.346715861894232,-0.723175675144652,
-1.5088476255522));
#49501=CARTESIAN_POINT('Ctrl Pts',(-0.454246347044275,-0.647770356613803,
-1.51413346241085));
#49502=CARTESIAN_POINT('Ctrl Pts',(-0.561776832194319,-0.572365038082953,
-1.5194192992695));
#49503=CARTESIAN_POINT('Ctrl Pts',(-0.650126318971814,-0.469606979707652,
-1.52470513612815));
#49504=CARTESIAN_POINT('Ctrl Pts',(-0.708556318914909,-0.351985967953831,
-1.5299909729868));
#49505=CARTESIAN_POINT('Ctrl Pts',(-0.762632363248006,-0.243129574794532,
-1.53488293171663));
#49506=CARTESIAN_POINT('Ctrl Pts',(-0.791081736219983,-0.121542748663734,
-1.53977489044646));
#49507=CARTESIAN_POINT('Ctrl Pts',(-0.791157484722713,9.84224722326565E-6,
-1.54466684917629));
#49508=CARTESIAN_POINT('Ctrl Pts',(-0.791145759608552,1.41466495050277E-5,
-1.5731331508237));
#49509=CARTESIAN_POINT('Ctrl Pts',(-0.791049088721019,-0.116326385441727,
-1.56845115576485));
#49510=CARTESIAN_POINT('Ctrl Pts',(-0.765065880610099,-0.232708668117082,
-1.56376916070601));
#49511=CARTESIAN_POINT('Ctrl Pts',(-0.715382449179442,-0.337896623282764,
-1.55908716564716));
#49512=CARTESIAN_POINT('Ctrl Pts',(-0.659291293631521,-0.456650779045952,
-1.55380132878851));
#49513=CARTESIAN_POINT('Ctrl Pts',(-0.572992411191032,-0.561136917854358,
-1.54851549192987));
#49514=CARTESIAN_POINT('Ctrl Pts',(-0.466975048453054,-0.638655212726037,
-1.54322965507122));
#49515=CARTESIAN_POINT('Ctrl Pts',(-0.360957685715075,-0.716173507597717,
-1.53794381821257));
#49516=CARTESIAN_POINT('Ctrl Pts',(-0.235221842679609,-0.766723958532671,
-1.53265798135392));
#49517=CARTESIAN_POINT('Ctrl Pts',(-0.105050153676812,-0.784162382311437,
-1.52737214449528));
#49518=CARTESIAN_POINT('Ctrl Pts',(0.0251215353259854,-0.801600806090204,
-1.52208630763663));
#49519=CARTESIAN_POINT('Ctrl Pts',(0.159729070296112,-0.785927202712783,
-1.51680047077798));
#49520=CARTESIAN_POINT('Ctrl Pts',(0.282411502077233,-0.73904662918814,
-1.51151463391933));
#49521=CARTESIAN_POINT('Ctrl Pts',(0.405093933858354,-0.692166055663498,
-1.50622879706069));
#49522=CARTESIAN_POINT('Ctrl Pts',(0.515851262450468,-0.614078511991633,
-1.50094296020204));
#49523=CARTESIAN_POINT('Ctrl Pts',(0.601221425553798,-0.514275192941416,
-1.49565712334339));
#49524=CARTESIAN_POINT('Ctrl Pts',(0.686591588657128,-0.414471873891198,
-1.49037128648474));
#49525=CARTESIAN_POINT('Ctrl Pts',(0.746574586271674,-0.292952779462627,
-1.48508544962609));
#49526=CARTESIAN_POINT('Ctrl Pts',(0.773879750943835,-0.164488016885666,
-1.47979961276745));
#49527=CARTESIAN_POINT('Ctrl Pts',(0.801184915615994,-0.0360232543087124,
-1.4745137759088));
#49528=CARTESIAN_POINT('Ctrl Pts',(0.795812247345771,0.0993871764166298,
-1.46922793905015));
#49529=CARTESIAN_POINT('Ctrl Pts',(0.758414770144211,0.22528473771424,-1.4639421021915));
#49530=CARTESIAN_POINT('Ctrl Pts',(0.721017292942649,0.351182299011858,
-1.45865626533285));
#49531=CARTESIAN_POINT('Ctrl Pts',(0.651595006809745,0.467566990881743,
-1.45337042847421));
#49532=CARTESIAN_POINT('Ctrl Pts',(0.558585882873856,0.560292769963976,
-1.44808459161556));
#49533=CARTESIAN_POINT('Ctrl Pts',(0.465576758937968,0.65301854904621,-1.44279875475691));
#49534=CARTESIAN_POINT('Ctrl Pts',(0.348980797199094,0.722085415340792,
-1.43751291789827));
#49535=CARTESIAN_POINT('Ctrl Pts',(0.222969719933163,0.759098597425129,
-1.43222708103962));
#49536=CARTESIAN_POINT('Ctrl Pts',(0.0969586426672318,0.796111779509465,
-1.42694124418097));
#49537=CARTESIAN_POINT('Ctrl Pts',(-0.0384675501257566,0.801071277383556,
-1.42165540732232));
#49538=CARTESIAN_POINT('Ctrl Pts',(-0.166848405060231,0.77337428606641,
-1.41636957046367));
#49539=CARTESIAN_POINT('Ctrl Pts',(-0.295229259994706,0.745677294749263,
-1.41108373360502));
#49540=CARTESIAN_POINT('Ctrl Pts',(-0.416564777070667,0.685323814240878,
-1.40579789674638));
#49541=CARTESIAN_POINT('Ctrl Pts',(-0.516107162071556,0.599649542548242,
-1.40051205988773));
#49542=CARTESIAN_POINT('Ctrl Pts',(-0.615649547072444,0.513975270855606,
-1.39522622302908));
#49543=CARTESIAN_POINT('Ctrl Pts',(-0.693398799998261,0.402980207978719,
-1.38994038617043));
#49544=CARTESIAN_POINT('Ctrl Pts',(-0.739904843820666,0.280155311765788,
-1.38465454931178));
#49545=CARTESIAN_POINT('Ctrl Pts',(-0.773694174145641,0.190915921588506,
-1.38081408314909));
#49546=CARTESIAN_POINT('Ctrl Pts',(-0.790990642988861,0.0954317246784125,
-1.37697361698639));
#49547=CARTESIAN_POINT('Ctrl Pts',(-0.791082733992286,-2.00018711214563E-5,
-1.3731331508237));
#49548=CARTESIAN_POINT('Origin',(0.,0.,-2.94));
#49549=CARTESIAN_POINT('',(-0.791073002592696,1.9102929482484E-5,-1.1446668491763));
#49550=CARTESIAN_POINT('',(-0.791059456711661,1.68138715613493E-5,-1.1731331508237));
#49551=CARTESIAN_POINT('',(-0.7911,-9.68818082805471E-17,-2.94));
#49552=CARTESIAN_POINT('Ctrl Pts',(-0.791073002592696,1.9102929482484E-5,
-1.1446668491763));
#49553=CARTESIAN_POINT('Ctrl Pts',(-0.791108504901705,0.0393221944095275,
-1.14624813917225));
#49554=CARTESIAN_POINT('Ctrl Pts',(-0.788231387404301,0.0786201345074876,
-1.1478294291682));
#49555=CARTESIAN_POINT('Ctrl Pts',(-0.782397600201548,0.117474141450363,
-1.14941071916415));
#49556=CARTESIAN_POINT('Ctrl Pts',(-0.762896782830441,0.247352874972065,
-1.1546965560228));
#49557=CARTESIAN_POINT('Ctrl Pts',(-0.710358457961914,0.372271147434174,
-1.15998239288145));
#49558=CARTESIAN_POINT('Ctrl Pts',(-0.631168426079748,0.477045696585406,
-1.1652682297401));
#49559=CARTESIAN_POINT('Ctrl Pts',(-0.551978394197586,0.581820245736633,
-1.17055406659874));
#49560=CARTESIAN_POINT('Ctrl Pts',(-0.446136655301788,0.666451071576987,
-1.17583990345739));
#49561=CARTESIAN_POINT('Ctrl Pts',(-0.326507803555503,0.72065167239659,
-1.18112574031604));
#49562=CARTESIAN_POINT('Ctrl Pts',(-0.206878951809204,0.774852273216199,
-1.18641157717469));
#49563=CARTESIAN_POINT('Ctrl Pts',(-0.0734629872124128,0.798622649015049,
-1.19169741403333));
#49564=CARTESIAN_POINT('Ctrl Pts',(0.0575239711751428,0.789073615989587,
-1.19698325089198));
#49565=CARTESIAN_POINT('Ctrl Pts',(0.188510929562691,0.779524582964126,
-1.20226908775063));
#49566=CARTESIAN_POINT('Ctrl Pts',(0.317068881741004,0.736656141114355,
-1.20755492460928));
#49567=CARTESIAN_POINT('Ctrl Pts',(0.427572178524106,0.665678759510014,
-1.21284076146793));
#49568=CARTESIAN_POINT('Ctrl Pts',(0.538075475307208,0.594701377905672,
-1.21812659832657));
#49569=CARTESIAN_POINT('Ctrl Pts',(0.6305241166951,0.49561505654676,-1.22341243518522));
#49570=CARTESIAN_POINT('Ctrl Pts',(0.693681380154711,0.380463298541787,
-1.22869827204387));
#49571=CARTESIAN_POINT('Ctrl Pts',(0.756838643614322,0.265311540536814,
-1.23398410890252));
#49572=CARTESIAN_POINT('Ctrl Pts',(0.790704529145653,0.13409434588578,-1.23926994576117));
#49573=CARTESIAN_POINT('Ctrl Pts',(0.791162788490867,0.00276058290871739,
-1.24455578261981));
#49574=CARTESIAN_POINT('Ctrl Pts',(0.791621047836082,-0.128573180068345,
-1.24984161947846));
#49575=CARTESIAN_POINT('Ctrl Pts',(0.75867168099518,-0.260023511371435,
-1.25512745633711));
#49576=CARTESIAN_POINT('Ctrl Pts',(0.696319537442132,-0.375613205953966,
-1.26041329319576));
#49577=CARTESIAN_POINT('Ctrl Pts',(0.633967393889087,-0.49120290053649,
-1.26569913005441));
#49578=CARTESIAN_POINT('Ctrl Pts',(0.542212473623899,-0.590931958398456,
-1.27098496691305));
#49579=CARTESIAN_POINT('Ctrl Pts',(0.432207180452458,-0.662678754658679,
-1.2762708037717));
#49580=CARTESIAN_POINT('Ctrl Pts',(0.322201887281011,-0.734425550918906,
-1.28155664063035));
#49581=CARTESIAN_POINT('Ctrl Pts',(0.193946221203308,-0.778190085577387,
-1.286842477489));
#49582=CARTESIAN_POINT('Ctrl Pts',(0.0630290898698403,-0.788652973455892,
-1.29212831434764));
#49583=CARTESIAN_POINT('Ctrl Pts',(-0.0678880414636275,-0.799115861334397,
-1.29741415120629));
#49584=CARTESIAN_POINT('Ctrl Pts',(-0.20146663805286,-0.776277102432927,
-1.30269998806494));
#49585=CARTESIAN_POINT('Ctrl Pts',(-0.321470813640404,-0.722912646651044,
-1.30798582492359));
#49586=CARTESIAN_POINT('Ctrl Pts',(-0.441474989227948,-0.669548190869161,
-1.31327166178223));
#49587=CARTESIAN_POINT('Ctrl Pts',(-0.547904743813803,-0.585658038206865,
-1.31855749864088));
#49588=CARTESIAN_POINT('Ctrl Pts',(-0.627824012534386,-0.48143866483267,
-1.32384333549953));
#49589=CARTESIAN_POINT('Ctrl Pts',(-0.707743281254969,-0.377219291458475,
-1.32912917235818));
#49590=CARTESIAN_POINT('Ctrl Pts',(-0.761152064110279,-0.25267069737238,
-1.33441500921682));
#49591=CARTESIAN_POINT('Ctrl Pts',(-0.781558760307008,-0.122931212057858,
-1.33970084607547));
#49592=CARTESIAN_POINT('Ctrl Pts',(-0.787949405049457,-0.0823014623070763,
-1.34135618044241));
#49593=CARTESIAN_POINT('Ctrl Pts',(-0.791103477187948,-0.041162632736165,
-1.34301151480935));
#49594=CARTESIAN_POINT('Ctrl Pts',(-0.791067994997204,-1.8415035504149E-5,
-1.3446668491763));
#49595=CARTESIAN_POINT('Ctrl Pts',(-0.791082733992286,-2.00018711214563E-5,
-1.3731331508237));
#49596=CARTESIAN_POINT('Ctrl Pts',(-0.791117392711325,-0.0359435389075563,
-1.37168778012775));
#49597=CARTESIAN_POINT('Ctrl Pts',(-0.788715197055925,-0.0718624767924898,
-1.3702424094318));
#49598=CARTESIAN_POINT('Ctrl Pts',(-0.783838218078167,-0.107442191432954,
-1.36879703873584));
#49599=CARTESIAN_POINT('Ctrl Pts',(-0.766002713794266,-0.23756006886979,
-1.36351120187719));
#49600=CARTESIAN_POINT('Ctrl Pts',(-0.715068870507469,-0.363141094194489,
-1.35822536501854));
#49601=CARTESIAN_POINT('Ctrl Pts',(-0.637227471078016,-0.468921450483326,
-1.3529395281599));
#49602=CARTESIAN_POINT('Ctrl Pts',(-0.559386071648563,-0.574701806772162,
-1.34765369130125));
#49603=CARTESIAN_POINT('Ctrl Pts',(-0.454637116076454,-0.660681494025135,
-1.3423678544426));
#49604=CARTESIAN_POINT('Ctrl Pts',(-0.335712375556184,-0.716410062407205,
-1.33708201758396));
#49605=CARTESIAN_POINT('Ctrl Pts',(-0.216787635035913,-0.772138630789275,
-1.33179618072531));
#49606=CARTESIAN_POINT('Ctrl Pts',(-0.0836871095674816,-0.797616080300441,
-1.32651034386666));
#49607=CARTESIAN_POINT('Ctrl Pts',(0.0474114220170869,-0.789745739894928,
-1.32122450700801));
#49608=CARTESIAN_POINT('Ctrl Pts',(0.178509953601655,-0.781875399489416,
-1.31593867014936));
#49609=CARTESIAN_POINT('Ctrl Pts',(0.307606491302361,-0.740657269167225,
-1.31065283329072));
#49610=CARTESIAN_POINT('Ctrl Pts',(0.419009923250545,-0.671101229947795,
-1.30536699643207));
#49611=CARTESIAN_POINT('Ctrl Pts',(0.53041335519873,-0.601545190728366,
-1.30008115957342));
#49612=CARTESIAN_POINT('Ctrl Pts',(0.624123681394395,-0.503651242611697,
-1.29479532271477));
#49613=CARTESIAN_POINT('Ctrl Pts',(0.688750827109173,-0.389317961024534,
-1.28950948585612));
#49614=CARTESIAN_POINT('Ctrl Pts',(0.753377972823951,-0.27498467943737,
-1.28422364899748));
#49615=CARTESIAN_POINT('Ctrl Pts',(0.788921938057842,-0.144212064379711,
-1.27893781213883));
#49616=CARTESIAN_POINT('Ctrl Pts',(0.791062511404142,-0.0128949474928493,
-1.27365197528018));
#49617=CARTESIAN_POINT('Ctrl Pts',(0.793203084750441,0.118422169394013,
-1.26836613842153));
#49618=CARTESIAN_POINT('Ctrl Pts',(0.761940266209149,0.250283788110078,
-1.26308030156288));
#49619=CARTESIAN_POINT('Ctrl Pts',(0.701073912784938,0.366662713446961,
-1.25779446470424));
#49620=CARTESIAN_POINT('Ctrl Pts',(0.640207559360726,0.483041638783844,
-1.25250862784559));
#49621=CARTESIAN_POINT('Ctrl Pts',(0.549737671053596,0.583937870741544,
-1.24722279098694));
#49622=CARTESIAN_POINT('Ctrl Pts',(0.440660461731521,0.657087919601657,
-1.24193695412829));
#49623=CARTESIAN_POINT('Ctrl Pts',(0.331583252409446,0.73023796846177,-1.23665111726965));
#49624=CARTESIAN_POINT('Ctrl Pts',(0.203898722072426,0.775641834224296,
-1.231365280411));
#49625=CARTESIAN_POINT('Ctrl Pts',(0.0731263593535346,0.787780878282514,
-1.22607944355235));
#49626=CARTESIAN_POINT('Ctrl Pts',(-0.0576460033653572,0.799919922340731,
-1.2207936066937));
#49627=CARTESIAN_POINT('Ctrl Pts',(-0.191506198466121,0.778794144694639,
-1.21550776983506));
#49628=CARTESIAN_POINT('Ctrl Pts',(-0.312184112640562,0.726971289965908,
-1.21022193297641));
#49629=CARTESIAN_POINT('Ctrl Pts',(-0.432862026814995,0.67514843523718,
-1.20493609611776));
#49630=CARTESIAN_POINT('Ctrl Pts',(-0.540357660063106,0.592628503425816,
-1.19965025925911));
#49631=CARTESIAN_POINT('Ctrl Pts',(-0.621605394694988,0.489441426430128,
-1.19436442240046));
#49632=CARTESIAN_POINT('Ctrl Pts',(-0.70285312932687,0.386254349434441,
-1.18907858554182));
#49633=CARTESIAN_POINT('Ctrl Pts',(-0.757852965342524,0.262400127254429,
-1.18379274868317));
#49634=CARTESIAN_POINT('Ctrl Pts',(-0.779919916490187,0.132932691546551,
-1.17850691182452));
#49635=CARTESIAN_POINT('Ctrl Pts',(-0.787397920109764,0.0890590296907594,
-1.17671565815758));
#49636=CARTESIAN_POINT('Ctrl Pts',(-0.791093967912682,0.0445407560544645,
-1.17492440449064));
#49637=CARTESIAN_POINT('Ctrl Pts',(-0.791059456711661,1.68138715613493E-5,
-1.1731331508237));
#49638=CARTESIAN_POINT('Origin',(0.,0.,-2.94));
#49639=CARTESIAN_POINT('',(-0.791153738188075,-1.14622333243219E-5,-0.944666849176297));
#49640=CARTESIAN_POINT('',(-0.791163026494784,-6.63049684663537E-6,-0.973133150823701));
#49641=CARTESIAN_POINT('',(-0.7911,-9.68818082805471E-17,-2.94));
#49642=CARTESIAN_POINT('Ctrl Pts',(-0.791153738188075,-1.14622333243219E-5,
-0.944666849176297));
#49643=CARTESIAN_POINT('Ctrl Pts',(-0.791069254281359,0.119702961705676,
-0.949484763535142));
#49644=CARTESIAN_POINT('Ctrl Pts',(-0.763503490006759,0.239454969527334,
-0.954302677893988));
#49645=CARTESIAN_POINT('Ctrl Pts',(-0.71099538606271,0.347032764603257,
-0.959120592252833));
#49646=CARTESIAN_POINT('Ctrl Pts',(-0.653387622509252,0.465058663785214,
-0.96440642911148));
#49647=CARTESIAN_POINT('Ctrl Pts',(-0.565757380114313,0.568430763467434,
-0.969692265970127));
#49648=CARTESIAN_POINT('Ctrl Pts',(-0.458755726373478,0.644584643185194,
-0.974978102828774));
#49649=CARTESIAN_POINT('Ctrl Pts',(-0.351754072632631,0.720738522902962,
-0.980263939687422));
#49650=CARTESIAN_POINT('Ctrl Pts',(-0.225381007545903,0.769674182656259,
-0.98554977654607));
#49651=CARTESIAN_POINT('Ctrl Pts',(-0.0949966169589208,0.785443709935347,
-0.990835613404718));
#49652=CARTESIAN_POINT('Ctrl Pts',(0.0353877736280465,0.801213237214434,
-0.996121450263366));
#49653=CARTESIAN_POINT('Ctrl Pts',(0.16978348971527,0.783816632019305,-1.00140728712201));
#49654=CARTESIAN_POINT('Ctrl Pts',(0.291855327792586,0.735368374591758,
-1.00669312398066));
#49655=CARTESIAN_POINT('Ctrl Pts',(0.413927165869916,0.686920117164204,
-1.01197896083931));
#49656=CARTESIAN_POINT('Ctrl Pts',(0.523675125937363,0.607420207504222,
-1.01726479769796));
#49657=CARTESIAN_POINT('Ctrl Pts',(0.607759829964756,0.506531507205476,
-1.02255063455661));
#49658=CARTESIAN_POINT('Ctrl Pts',(0.691844533992139,0.405642806906743,
-1.02783647141525));
#49659=CARTESIAN_POINT('Ctrl Pts',(0.750265981979478,0.283365315969246,
-1.0331223082739));
#49660=CARTESIAN_POINT('Ctrl Pts',(0.775923305907959,0.15456132135662,-1.03840814513255));
#49661=CARTESIAN_POINT('Ctrl Pts',(0.801580629836442,0.0257573267439869,
-1.0436939819912));
#49662=CARTESIAN_POINT('Ctrl Pts',(0.794473829706067,-0.10957317154376,
-1.04897981884984));
#49663=CARTESIAN_POINT('Ctrl Pts',(0.75546670556802,-0.234981351363983,
-1.05426565570849));
#49664=CARTESIAN_POINT('Ctrl Pts',(0.716459581429971,-0.360389531184213,
-1.05955149256714));
#49665=CARTESIAN_POINT('Ctrl Pts',(0.645552133284242,-0.4758753925369,-1.06483732942579));
#49666=CARTESIAN_POINT('Ctrl Pts',(0.551362847118086,-0.567402140926943,
-1.07012316628444));
#49667=CARTESIAN_POINT('Ctrl Pts',(0.457173560951941,-0.658928889316976,
-1.07540900314308));
#49668=CARTESIAN_POINT('Ctrl Pts',(0.339702436765368,-0.726496524744374,
-1.08069484000173));
#49669=CARTESIAN_POINT('Ctrl Pts',(0.213227568950196,-0.76189250065231,
-1.08598067686038));
#49670=CARTESIAN_POINT('Ctrl Pts',(0.0867527011350093,-0.797288476560251,
-1.09126651371903));
#49671=CARTESIAN_POINT('Ctrl Pts',(-0.0487259103087836,-0.800512792948724,
-1.09655235057767));
#49672=CARTESIAN_POINT('Ctrl Pts',(-0.176741440740974,-0.771173548454202,
-1.10183818743632));
#49673=CARTESIAN_POINT('Ctrl Pts',(-0.304756971173165,-0.741834303959681,
-1.10712402429497));
#49674=CARTESIAN_POINT('Ctrl Pts',(-0.425309420593757,-0.679931498582165,
-1.11240986115362));
#49675=CARTESIAN_POINT('Ctrl Pts',(-0.523746173188335,-0.592989143898281,
-1.11769569801227));
#49676=CARTESIAN_POINT('Ctrl Pts',(-0.622182925782902,-0.506046789214406,
-1.12298153487091));
#49677=CARTESIAN_POINT('Ctrl Pts',(-0.698503981551462,-0.394064885224168,
-1.12826737172956));
#49678=CARTESIAN_POINT('Ctrl Pts',(-0.7434328544989,-0.270654335938406,
-1.13355320858821));
#49679=CARTESIAN_POINT('Ctrl Pts',(-0.774920983961236,-0.184162797246254,
-1.1372577554509));
#49680=CARTESIAN_POINT('Ctrl Pts',(-0.790989830013477,-0.0920577106906312,
-1.1409623023136));
#49681=CARTESIAN_POINT('Ctrl Pts',(-0.791073002592696,1.9102929482484E-5,
-1.1446668491763));
#49682=CARTESIAN_POINT('Ctrl Pts',(-0.791059456711661,1.68138715613493E-5,
-1.1731331508237));
#49683=CARTESIAN_POINT('Ctrl Pts',(-0.790992128300705,-0.0868456014593881,
-1.16963856763199));
#49684=CARTESIAN_POINT('Ctrl Pts',(-0.776726037359125,-0.173729591666139,
-1.16614398444028));
#49685=CARTESIAN_POINT('Ctrl Pts',(-0.748642821403881,-0.255890802062731,
-1.16264940124858));
#49686=CARTESIAN_POINT('Ctrl Pts',(-0.706164708890245,-0.380166210728354,
-1.15736356438993));
#49687=CARTESIAN_POINT('Ctrl Pts',(-0.632074417583308,-0.493636378823848,
-1.15207772753128));
#49688=CARTESIAN_POINT('Ctrl Pts',(-0.53537729394692,-0.582509510433902,
-1.14679189067263));
#49689=CARTESIAN_POINT('Ctrl Pts',(-0.438680170310532,-0.671382642043956,
-1.14150605381399));
#49690=CARTESIAN_POINT('Ctrl Pts',(-0.319376214344695,-0.735658737168568,
-1.13622021695534));
#49691=CARTESIAN_POINT('Ctrl Pts',(-0.191966293019002,-0.76752532138322,
-1.13093438009669));
#49692=CARTESIAN_POINT('Ctrl Pts',(-0.0645563716933151,-0.79939190559787,
-1.12564854323804));
#49693=CARTESIAN_POINT('Ctrl Pts',(0.0709595149922231,-0.798848978902562,
-1.1203627063794));
#49694=CARTESIAN_POINT('Ctrl Pts',(0.198110011757025,-0.765962531630302,
-1.11507686952075));
#49695=CARTESIAN_POINT('Ctrl Pts',(0.325260508521841,-0.733076084358039,
-1.1097910326621));
#49696=CARTESIAN_POINT('Ctrl Pts',(0.444045615365914,-0.667846116508817,
-1.10450519580345));
#49697=CARTESIAN_POINT('Ctrl Pts',(0.540027529130329,-0.578201041508283,
-1.0992193589448));
#49698=CARTESIAN_POINT('Ctrl Pts',(0.636009442894732,-0.488555966507759,
-1.09393352208616));
#49699=CARTESIAN_POINT('Ctrl Pts',(0.709188163579479,-0.374495784355932,
-1.08864768522751));
#49700=CARTESIAN_POINT('Ctrl Pts',(0.750669142088827,-0.249884004561106,
-1.08336184836886));
#49701=CARTESIAN_POINT('Ctrl Pts',(0.792150120598178,-0.125272224766274,
-1.07807601151021));
#49702=CARTESIAN_POINT('Ctrl Pts',(0.801933356932126,0.00989115267157506,
-1.07279017465157));
#49703=CARTESIAN_POINT('Ctrl Pts',(0.778829742083658,0.139177618408181,
-1.06750433779292));
#49704=CARTESIAN_POINT('Ctrl Pts',(0.75572612723519,0.268464084144795,-1.06221850093427));
#49705=CARTESIAN_POINT('Ctrl Pts',(0.699735661204308,0.391873638180182,
-1.05693266407562));
#49706=CARTESIAN_POINT('Ctrl Pts',(0.617663736929631,0.494406396299637,
-1.05164682721697));
#49707=CARTESIAN_POINT('Ctrl Pts',(0.535591812654964,0.596939154419081,
-1.04636099035832));
#49708=CARTESIAN_POINT('Ctrl Pts',(0.427438430136513,0.678595116622594,
-1.04107515349968));
#49709=CARTESIAN_POINT('Ctrl Pts',(0.306349153572166,0.729449362687698,
-1.03578931664103));
#49710=CARTESIAN_POINT('Ctrl Pts',(0.185259877007812,0.780303608752805,
-1.03050347978238));
#49711=CARTESIAN_POINT('Ctrl Pts',(0.0512347063975671,0.800356138679497,
-1.02521764292373));
#49712=CARTESIAN_POINT('Ctrl Pts',(-0.0794361929085426,0.78716965634866,
-1.01993180606509));
#49713=CARTESIAN_POINT('Ctrl Pts',(-0.210107092214652,0.773983174017823,
-1.01464596920644));
#49714=CARTESIAN_POINT('Ctrl Pts',(-0.337423720216622,0.727557679429456,
-1.00936013234779));
#49715=CARTESIAN_POINT('Ctrl Pts',(-0.445911305179286,0.653535985645149,
-1.00407429548914));
#49716=CARTESIAN_POINT('Ctrl Pts',(-0.55439889014195,0.579514291860843,
-0.998788458630495));
#49717=CARTESIAN_POINT('Ctrl Pts',(-0.644057432065305,0.477896398880599,
-0.993502621771847));
#49718=CARTESIAN_POINT('Ctrl Pts',(-0.703989332637604,0.361033511120964,
-0.988216784913199));
#49719=CARTESIAN_POINT('Ctrl Pts',(-0.760996443192033,0.249873753152225,
-0.983188906883366));
#49720=CARTESIAN_POINT('Ctrl Pts',(-0.791107547260317,0.124920661667419,
-0.978161028853534));
#49721=CARTESIAN_POINT('Ctrl Pts',(-0.791163026494784,-6.63049684663537E-6,
-0.973133150823701));
#49722=CARTESIAN_POINT('Origin',(0.,0.,-2.94));
#49723=CARTESIAN_POINT('',(-0.79103327968755,-2.89210560314168E-6,-0.744666849176298));
#49724=CARTESIAN_POINT('',(-0.791037024154788,-7.56658461008487E-6,-0.7731331508237));
#49725=CARTESIAN_POINT('',(-0.7911,-9.68818082805471E-17,-2.94));
#49726=CARTESIAN_POINT('Ctrl Pts',(-0.79103327968755,-2.89210560314168E-6,
-0.744666849176298));
#49727=CARTESIAN_POINT('Ctrl Pts',(-0.791024492119856,0.0688233200155534,
-0.747435551039388));
#49728=CARTESIAN_POINT('Ctrl Pts',(-0.782132078258211,0.137651760409329,
-0.750204252902477));
#49729=CARTESIAN_POINT('Ctrl Pts',(-0.764384099192582,0.204115476170194,
-0.752972954765567));
#49730=CARTESIAN_POINT('Ctrl Pts',(-0.730500739209966,0.331003951673808,
-0.758258791624215));
#49731=CARTESIAN_POINT('Ctrl Pts',(-0.664340509511136,0.449273450620519,
-0.763544628482863));
#49732=CARTESIAN_POINT('Ctrl Pts',(-0.573944892725679,0.544548839705632,
-0.76883046534151));
#49733=CARTESIAN_POINT('Ctrl Pts',(-0.483549275940222,0.639824228790745,
-0.774116302200158));
#49734=CARTESIAN_POINT('Ctrl Pts',(-0.368918272068141,0.712105508014256,
-0.779402139058806));
#49735=CARTESIAN_POINT('Ctrl Pts',(-0.24398477146737,0.752607208311651,
-0.784687975917454));
#49736=CARTESIAN_POINT('Ctrl Pts',(-0.119051270866599,0.793108908609046,
-0.789973812776101));
#49737=CARTESIAN_POINT('Ctrl Pts',(0.0161847264628582,0.801831029980324,
-0.79525964963475));
#49738=CARTESIAN_POINT('Ctrl Pts',(0.145285884550884,0.777713437238234,
-0.800545486493398));
#49739=CARTESIAN_POINT('Ctrl Pts',(0.274387042638903,0.753595844496146,
-0.805831323352045));
#49740=CARTESIAN_POINT('Ctrl Pts',(0.397353361485488,0.696638537640694,
-0.811117160210692));
#49741=CARTESIAN_POINT('Ctrl Pts',(0.49923883014826,0.61376442482669,-0.816402997069339));
#49742=CARTESIAN_POINT('Ctrl Pts',(0.601124298811043,0.530890312012677,
-0.821688833927988));
#49743=CARTESIAN_POINT('Ctrl Pts',(0.681928917290005,0.422099393240108,
-0.826974670786636));
#49744=CARTESIAN_POINT('Ctrl Pts',(0.731831242418353,0.300614722412347,
-0.832260507645284));
#49745=CARTESIAN_POINT('Ctrl Pts',(0.781733567546697,0.179130051584592,
-0.837546344503932));
#49746=CARTESIAN_POINT('Ctrl Pts',(0.800733599324429,0.0449516287016287,
-0.84283218136258));
#49747=CARTESIAN_POINT('Ctrl Pts',(0.786521968116677,-0.0856117537520969,
-0.848118018221228));
#49748=CARTESIAN_POINT('Ctrl Pts',(0.772310336908926,-0.216175136205815,
-0.853403855079876));
#49749=CARTESIAN_POINT('Ctrl Pts',(0.724887042715701,-0.343123478230312,
-0.858689691938524));
#49750=CARTESIAN_POINT('Ctrl Pts',(0.650016176717285,-0.451026771618364,
-0.863975528797172));
#49751=CARTESIAN_POINT('Ctrl Pts',(0.575145310718861,-0.558930065006429,
-0.86926136565582));
#49752=CARTESIAN_POINT('Ctrl Pts',(0.472826872915242,-0.647788309758041,
-0.874547202514467));
#49753=CARTESIAN_POINT('Ctrl Pts',(0.355497215840721,-0.706801180134935,
-0.879833039373115));
#49754=CARTESIAN_POINT('Ctrl Pts',(0.238167558766213,-0.765814050511822,
-0.885118876231763));
#49755=CARTESIAN_POINT('Ctrl Pts',(0.105826682420811,-0.794981546513998,
-0.89040471309041));
#49756=CARTESIAN_POINT('Ctrl Pts',(-0.0254399663468239,-0.79075848830279,
-0.895690549949058));
#49757=CARTESIAN_POINT('Ctrl Pts',(-0.156706615114466,-0.786535430091583,
-0.900976386807706));
#49758=CARTESIAN_POINT('Ctrl Pts',(-0.286899036304337,-0.748921817666989,
-0.906262223666354));
#49759=CARTESIAN_POINT('Ctrl Pts',(-0.40019291826776,-0.682489418876934,
-0.911548060525002));
#49760=CARTESIAN_POINT('Ctrl Pts',(-0.513486800231182,-0.616057020086879,
-0.916833897383649));
#49761=CARTESIAN_POINT('Ctrl Pts',(-0.609882142968154,-0.520805834931365,
-0.922119734242297));
#49762=CARTESIAN_POINT('Ctrl Pts',(-0.677662519892473,-0.408313222714652,
-0.927405571100945));
#49763=CARTESIAN_POINT('Ctrl Pts',(-0.745442896816793,-0.295820610497938,
-0.932691407959593));
#49764=CARTESIAN_POINT('Ctrl Pts',(-0.784608307928459,-0.166086571220027,
-0.93797724481824));
#49765=CARTESIAN_POINT('Ctrl Pts',(-0.790398371128303,-0.0348797022402185,
-0.943263081676888));
#49766=CARTESIAN_POINT('Ctrl Pts',(-0.790910929672757,-0.0232647682636074,
-0.943731004176691));
#49767=CARTESIAN_POINT('Ctrl Pts',(-0.791161943381833,-0.0116382925046326,
-0.944198926676494));
#49768=CARTESIAN_POINT('Ctrl Pts',(-0.791153738188075,-1.14622333243219E-5,
-0.944666849176297));
#49769=CARTESIAN_POINT('Ctrl Pts',(-0.791163026494784,-6.63049684663537E-6,
-0.973133150823701));
#49770=CARTESIAN_POINT('Ctrl Pts',(-0.791165872896041,-0.0064161133407936,
-0.972875191994886));
#49771=CARTESIAN_POINT('Ctrl Pts',(-0.791089604615324,-0.0128255282738238,
-0.972617233166071));
#49772=CARTESIAN_POINT('Ctrl Pts',(-0.790933794943816,-0.0192330090117345,
-0.972359274337257));
#49773=CARTESIAN_POINT('Ctrl Pts',(-0.787741097456487,-0.150528758845775,
-0.967073437478609));
#49774=CARTESIAN_POINT('Ctrl Pts',(-0.751150443260588,-0.281012375974835,
-0.96178760061996));
#49775=CARTESIAN_POINT('Ctrl Pts',(-0.685609264166152,-0.394824155174704,
-0.956501763761312));
#49776=CARTESIAN_POINT('Ctrl Pts',(-0.620068085071716,-0.508635934374572,
-0.951215926902664));
#49777=CARTESIAN_POINT('Ctrl Pts',(-0.525576381078742,-0.605775875645253,
-0.945930090044017));
#49778=CARTESIAN_POINT('Ctrl Pts',(-0.41361919992299,-0.674437049749595,
-0.94064425318537));
#49779=CARTESIAN_POINT('Ctrl Pts',(-0.301662018767232,-0.74309822385394,
-0.935358416326722));
#49780=CARTESIAN_POINT('Ctrl Pts',(-0.17223936044869,-0.783280630791945,
-0.930072579468073));
#49781=CARTESIAN_POINT('Ctrl Pts',(-0.0410819753514236,-0.790100277130122,
-0.924786742609425));
#49782=CARTESIAN_POINT('Ctrl Pts',(0.090075409745828,-0.796919923468298,
-0.919500905750777));
#49783=CARTESIAN_POINT('Ctrl Pts',(0.222967521621809,-0.770376809206654,
-0.914215068892129));
#49784=CARTESIAN_POINT('Ctrl Pts',(0.341441913192751,-0.713697132217263,
-0.908929232033482));
#49785=CARTESIAN_POINT('Ctrl Pts',(0.459916304763692,-0.657017455227872,
-0.903643395174834));
#49786=CARTESIAN_POINT('Ctrl Pts',(0.563972976029599,-0.570201215510731,
-0.898357558316188));
#49787=CARTESIAN_POINT('Ctrl Pts',(0.640964299884474,-0.46380054214444,
-0.89307172145754));
#49788=CARTESIAN_POINT('Ctrl Pts',(0.717955623739359,-0.357399868778137,
-0.887785884598892));
#49789=CARTESIAN_POINT('Ctrl Pts',(0.767881600183203,-0.231414761762697,
-0.882500047740244));
#49790=CARTESIAN_POINT('Ctrl Pts',(0.784673948102637,-0.101158152360013,
-0.877214210881596));
#49791=CARTESIAN_POINT('Ctrl Pts',(0.80146629602207,0.0290984570426636,
-0.871928374022948));
#49792=CARTESIAN_POINT('Ctrl Pts',(0.785125015417087,0.163626568832565,
-0.8666425371643));
#49793=CARTESIAN_POINT('Ctrl Pts',(0.737636316503833,0.286074887388823,
-0.861356700305653));
#49794=CARTESIAN_POINT('Ctrl Pts',(0.690147617590579,0.408523205945081,
-0.856070863447005));
#49795=CARTESIAN_POINT('Ctrl Pts',(0.611511500369052,0.518891731267699,
-0.850785026588357));
#49796=CARTESIAN_POINT('Ctrl Pts',(0.511285836291241,0.603765658370727,
-0.845499189729709));
#49797=CARTESIAN_POINT('Ctrl Pts',(0.411060172213435,0.68863958547375,-0.840213352871062));
#49798=CARTESIAN_POINT('Ctrl Pts',(0.289244961279322,0.748018914357198,
-0.834927516012414));
#49799=CARTESIAN_POINT('Ctrl Pts',(0.160646302367462,0.774686350825631,
-0.829641679153766));
#49800=CARTESIAN_POINT('Ctrl Pts',(0.0320476434555805,0.801353787294069,
-0.824355842295117));
#49801=CARTESIAN_POINT('Ctrl Pts',(-0.103334463434049,0.795309331347496,
-0.819070005436469));
#49802=CARTESIAN_POINT('Ctrl Pts',(-0.229044923362013,0.75728765981096,
-0.813784168577821));
#49803=CARTESIAN_POINT('Ctrl Pts',(-0.354755383289956,0.719265988274431,
-0.808498331719173));
#49804=CARTESIAN_POINT('Ctrl Pts',(-0.470794196256217,0.649267101147948,
-0.803212494860526));
#49805=CARTESIAN_POINT('Ctrl Pts',(-0.56305735894832,0.555799052854549,
-0.797926658001879));
#49806=CARTESIAN_POINT('Ctrl Pts',(-0.655320521640422,0.46233100456115,
-0.792640821143232));
#49807=CARTESIAN_POINT('Ctrl Pts',(-0.723808034058369,0.345393795100832,
-0.787354984284584));
#49808=CARTESIAN_POINT('Ctrl Pts',(-0.760195542674977,0.219200623897304,
-0.782069147425936));
#49809=CARTESIAN_POINT('Ctrl Pts',(-0.78070056783669,0.148088468953461,
-0.779090481891858));
#49810=CARTESIAN_POINT('Ctrl Pts',(-0.791012146346498,0.074037057278515,
-0.776111816357779));
#49811=CARTESIAN_POINT('Ctrl Pts',(-0.791037024154788,-7.56658461008487E-6,
-0.7731331508237));
#49812=CARTESIAN_POINT('Origin',(0.,0.,-2.94));
#49813=CARTESIAN_POINT('',(-0.791138066768001,1.60959521169762E-5,-0.544666849176297));
#49814=CARTESIAN_POINT('',(-0.791122640286116,1.87499586476574E-5,-0.573133150823702));
#49815=CARTESIAN_POINT('',(-0.7911,-9.68818082805471E-17,-2.94));
#49816=CARTESIAN_POINT('Ctrl Pts',(-0.791138066768001,1.60959521169762E-5,
-0.544666849176297));
#49817=CARTESIAN_POINT('Ctrl Pts',(-0.791154370742701,0.0178948272985896,
-0.545386338543632));
#49818=CARTESIAN_POINT('Ctrl Pts',(-0.790560616501651,0.03577247744017,
-0.546105827910967));
#49819=CARTESIAN_POINT('Ctrl Pts',(-0.789349314925486,0.0536081872233632,
-0.546825317278302));
#49820=CARTESIAN_POINT('Ctrl Pts',(-0.780450305699053,0.184640911892175,
-0.55211115413695));
#49821=CARTESIAN_POINT('Ctrl Pts',(-0.738220245989705,0.313409978176958,
-0.557396990995598));
#49822=CARTESIAN_POINT('Ctrl Pts',(-0.667792012348153,0.424264076908017,
-0.562682827854246));
#49823=CARTESIAN_POINT('Ctrl Pts',(-0.597363778706602,0.535118175639075,
-0.567968664712894));
#49824=CARTESIAN_POINT('Ctrl Pts',(-0.498737371132847,0.628057306816409,
-0.573254501571542));
#49825=CARTESIAN_POINT('Ctrl Pts',(-0.383900392253534,0.691785131047376,
-0.578540338430189));
#49826=CARTESIAN_POINT('Ctrl Pts',(-0.269063413374222,0.755512955278343,
-0.583826175288837));
#49827=CARTESIAN_POINT('Ctrl Pts',(-0.138015863189353,0.790029472562943,
-0.589112012147485));
#49828=CARTESIAN_POINT('Ctrl Pts',(-0.00668599048618175,0.791139353238011,
-0.594397849006133));
#49829=CARTESIAN_POINT('Ctrl Pts',(0.124643882216989,0.792249233913078,
-0.599683685864781));
#49830=CARTESIAN_POINT('Ctrl Pts',(0.256256077438462,0.759952477978614,
-0.604969522723429));
#49831=CARTESIAN_POINT('Ctrl Pts',(0.372153716289941,0.698174612945949,
-0.610255359582077));
#49832=CARTESIAN_POINT('Ctrl Pts',(0.488051355141419,0.636396747913284,
-0.615541196440724));
#49833=CARTESIAN_POINT('Ctrl Pts',(0.588234437622903,0.545137773782418,
-0.620827033299372));
#49834=CARTESIAN_POINT('Ctrl Pts',(0.660526154173397,0.435489814305162,
-0.62611287015802));
#49835=CARTESIAN_POINT('Ctrl Pts',(0.732817870723891,0.325841854827906,
-0.631398707016668));
#49836=CARTESIAN_POINT('Ctrl Pts',(0.777218221343395,0.19780491000426,-0.636684543875315));
#49837=CARTESIAN_POINT('Ctrl Pts',(0.788330540242214,0.066941302885881,
-0.641970380733963));
#49838=CARTESIAN_POINT('Ctrl Pts',(0.799442859141033,-0.0639223042324982,
-0.647256217592611));
#49839=CARTESIAN_POINT('Ctrl Pts',(0.777267146319167,-0.197612573645611,
-0.652542054451259));
#49840=CARTESIAN_POINT('Ctrl Pts',(0.724498761364504,-0.31788004575931,
-0.657827891309907));
#49841=CARTESIAN_POINT('Ctrl Pts',(0.671730376409841,-0.438147517873008,
-0.663113728168555));
#49842=CARTESIAN_POINT('Ctrl Pts',(0.588369319322382,-0.544992192687291,
-0.668399565027202));
#49843=CARTESIAN_POINT('Ctrl Pts',(0.484547757049015,-0.625427573624165,
-0.67368540188585));
#49844=CARTESIAN_POINT('Ctrl Pts',(0.380726194775648,-0.705862954561039,
-0.678971238744498));
#49845=CARTESIAN_POINT('Ctrl Pts',(0.256444127316373,-0.759889041620504,
-0.684257075603146));
#49846=CARTESIAN_POINT('Ctrl Pts',(0.126807489024694,-0.780939203419763,
-0.689542912461794));
#49847=CARTESIAN_POINT('Ctrl Pts',(-0.00282914926697755,-0.801989365219021,
-0.694828749320442));
#49848=CARTESIAN_POINT('Ctrl Pts',(-0.137820358391053,-0.790063601758076,
-0.700114586179089));
#49849=CARTESIAN_POINT('Ctrl Pts',(-0.261758555298625,-0.746611436718336,
-0.705400423037737));
#49850=CARTESIAN_POINT('Ctrl Pts',(-0.38569675220621,-0.703159271678591,
-0.710686259896385));
#49851=CARTESIAN_POINT('Ctrl Pts',(-0.498581936897288,-0.628180705060044,
-0.715972096755033));
#49852=CARTESIAN_POINT('Ctrl Pts',(-0.586693415596102,-0.530789049252922,
-0.721257933613681));
#49853=CARTESIAN_POINT('Ctrl Pts',(-0.674804894294906,-0.43339739344581,
-0.726543770472328));
#49854=CARTESIAN_POINT('Ctrl Pts',(-0.738142667001452,-0.313592648450128,
-0.731829607330976));
#49855=CARTESIAN_POINT('Ctrl Pts',(-0.769008308221525,-0.185936549922035,
-0.737115444189623));
#49856=CARTESIAN_POINT('Ctrl Pts',(-0.78370664034055,-0.125146245265584,
-0.739632579185181));
#49857=CARTESIAN_POINT('Ctrl Pts',(-0.791041268808539,-0.0625754895569357,
-0.742149714180739));
#49858=CARTESIAN_POINT('Ctrl Pts',(-0.79103327968755,-2.89210560314168E-6,
-0.744666849176298));
#49859=CARTESIAN_POINT('Ctrl Pts',(-0.791037024154788,-7.56658461008487E-6,
-0.7731331508237));
#49860=CARTESIAN_POINT('Ctrl Pts',(-0.79105629364485,-0.0573599718684727,
-0.770825979499131));
#49861=CARTESIAN_POINT('Ctrl Pts',(-0.784904040672549,-0.114708304793828,
-0.768518808174561));
#49862=CARTESIAN_POINT('Ctrl Pts',(-0.772536929917119,-0.170683533283396,
-0.766211636849992));
#49863=CARTESIAN_POINT('Ctrl Pts',(-0.744203303727385,-0.298925386313782,
-0.760925799991344));
#49864=CARTESIAN_POINT('Ctrl Pts',(-0.683248546532655,-0.419959959427814,
-0.755639963132697));
#49865=CARTESIAN_POINT('Ctrl Pts',(-0.597081438855663,-0.519076036813415,
-0.750354126274049));
#49866=CARTESIAN_POINT('Ctrl Pts',(-0.510914331178661,-0.618192114199027,
-0.745068289415401));
#49867=CARTESIAN_POINT('Ctrl Pts',(-0.39953487301939,-0.695389695856203,
-0.739782452556753));
#49868=CARTESIAN_POINT('Ctrl Pts',(-0.276480743768598,-0.741285757953729,
-0.734496615698105));
#49869=CARTESIAN_POINT('Ctrl Pts',(-0.15342661451782,-0.78718182005125,
-0.729210778839458));
#49870=CARTESIAN_POINT('Ctrl Pts',(-0.0186978141755228,-0.801776362589129,
-0.72392494198081));
#49871=CARTESIAN_POINT('Ctrl Pts',(0.111329968833544,-0.783295483619938,
-0.718639105122162));
#49872=CARTESIAN_POINT('Ctrl Pts',(0.241357751842625,-0.764814604650745,
-0.713353268263514));
#49873=CARTESIAN_POINT('Ctrl Pts',(0.366684517518475,-0.713258304174474,
-0.708067431404866));
#49874=CARTESIAN_POINT('Ctrl Pts',(0.472077353070542,-0.634893021963372,
-0.702781594546217));
#49875=CARTESIAN_POINT('Ctrl Pts',(0.577470188622603,-0.556527739752275,
-0.69749575768757));
#49876=CARTESIAN_POINT('Ctrl Pts',(0.662929094050884,-0.451353475806351,
-0.692209920828922));
#49877=CARTESIAN_POINT('Ctrl Pts',(0.718066918242495,-0.332153695667528,
-0.686924083970274));
#49878=CARTESIAN_POINT('Ctrl Pts',(0.773204742434107,-0.212953915528704,
-0.681638247111627));
#49879=CARTESIAN_POINT('Ctrl Pts',(0.798021485389048,-0.0797286191969827,
-0.676352410252979));
#49880=CARTESIAN_POINT('Ctrl Pts',(0.78950078201452,0.0513292491502936,
-0.671066573394331));
#49881=CARTESIAN_POINT('Ctrl Pts',(0.780980078639991,0.182387117497577,
-0.665780736535683));
#49882=CARTESIAN_POINT('Ctrl Pts',(0.739121928935989,0.311277557860415,
-0.660494899677034));
#49883=CARTESIAN_POINT('Ctrl Pts',(0.66901400544059,0.422334508587931,-0.655209062818386));
#49884=CARTESIAN_POINT('Ctrl Pts',(0.598906081945198,0.533391459315435,
-0.649923225959738));
#49885=CARTESIAN_POINT('Ctrl Pts',(0.500548384658416,0.62661492040762,-0.644637389101092));
#49886=CARTESIAN_POINT('Ctrl Pts',(0.385895855662796,0.690673993431162,
-0.639351552242444));
#49887=CARTESIAN_POINT('Ctrl Pts',(0.271243326667177,0.754733066454704,
-0.634065715383797));
#49888=CARTESIAN_POINT('Ctrl Pts',(0.140295965962721,0.789627751409603,
-0.628779878525149));
#49889=CARTESIAN_POINT('Ctrl Pts',(0.00896984474943487,0.791116754028786,
-0.623494041666501));
#49890=CARTESIAN_POINT('Ctrl Pts',(-0.122356276463859,0.792605756647969,
-0.618208204807853));
#49891=CARTESIAN_POINT('Ctrl Pts',(-0.254061158185983,0.760689076931433,
-0.612922367949206));
#49892=CARTESIAN_POINT('Ctrl Pts',(-0.370136655895347,0.699246045811115,
-0.607636531090558));
#49893=CARTESIAN_POINT('Ctrl Pts',(-0.486212153604717,0.637803014690794,
-0.60235069423191));
#49894=CARTESIAN_POINT('Ctrl Pts',(-0.586658267301324,0.546833632166687,
-0.597064857373262));
#49895=CARTESIAN_POINT('Ctrl Pts',(-0.659266217146009,0.43739482341457,
-0.591779020514613));
#49896=CARTESIAN_POINT('Ctrl Pts',(-0.731874166990686,0.327956014662466,
-0.586493183655966));
#49897=CARTESIAN_POINT('Ctrl Pts',(-0.776643952983447,0.200047779682357,
-0.581207346797319));
#49898=CARTESIAN_POINT('Ctrl Pts',(-0.788134006102694,0.0692167974149916,
-0.575921509938671));
#49899=CARTESIAN_POINT('Ctrl Pts',(-0.790154398533972,0.046211688247417,
-0.574992056900348));
#49900=CARTESIAN_POINT('Ctrl Pts',(-0.791145810275827,0.0231162102499581,
-0.574062603862025));
#49901=CARTESIAN_POINT('Ctrl Pts',(-0.791122640286116,1.87499586476574E-5,
-0.573133150823702));
#49902=CARTESIAN_POINT('Origin',(0.,0.,-2.94));
#49903=CARTESIAN_POINT('',(-0.791091445179114,-2.03764682111252E-5,-0.3446668491763));
#49904=CARTESIAN_POINT('',(-0.791107814146002,-2.00951009365201E-5,-0.373133150823702));
#49905=CARTESIAN_POINT('',(-0.7911,-9.68818082805471E-17,-2.94));
#49906=CARTESIAN_POINT('Ctrl Pts',(-0.791091445179114,-2.03764682111252E-5,
-0.3446668491763));
#49907=CARTESIAN_POINT('Ctrl Pts',(-0.790992936328914,0.0983025670368676,
-0.348622962906527));
#49908=CARTESIAN_POINT('Ctrl Pts',(-0.772614090163263,0.196661307733409,
-0.352579076636755));
#49909=CARTESIAN_POINT('Ctrl Pts',(-0.736807395616188,0.288203124009163,
-0.356535190366982));
#49910=CARTESIAN_POINT('Ctrl Pts',(-0.688965407561815,0.410513840933409,
-0.36182102722563));
#49911=CARTESIAN_POINT('Ctrl Pts',(-0.610011002822924,0.52065489764232,
-0.367106864084277));
#49912=CARTESIAN_POINT('Ctrl Pts',(-0.509540739832612,0.605239137095278,
-0.372392700942925));
#49913=CARTESIAN_POINT('Ctrl Pts',(-0.409070476842299,0.689823376548237,
-0.377678537801572));
#49914=CARTESIAN_POINT('Ctrl Pts',(-0.287084355600562,0.748850798745245,
-0.38296437466022));
#49915=CARTESIAN_POINT('Ctrl Pts',(-0.158409248097563,0.775146882115055,
-0.388250211518869));
#49916=CARTESIAN_POINT('Ctrl Pts',(-0.0297341405945646,0.801442965484864,
-0.393536048377516));
#49917=CARTESIAN_POINT('Ctrl Pts',(0.1056299531697,0.795007710027475,-0.398821885236164));
#49918=CARTESIAN_POINT('Ctrl Pts',(0.231230127528721,0.756623292553696,
-0.404107722094812));
#49919=CARTESIAN_POINT('Ctrl Pts',(0.356830301887734,0.718238875079919,
-0.40939355895346));
#49920=CARTESIAN_POINT('Ctrl Pts',(0.47266655684151,0.647905295589755,-0.414679395812107));
#49921=CARTESIAN_POINT('Ctrl Pts',(0.564659509179019,0.554171288860078,
-0.419965232670754));
#49922=CARTESIAN_POINT('Ctrl Pts',(0.656652461516538,0.460437282130389,
-0.425251069529402));
#49923=CARTESIAN_POINT('Ctrl Pts',(0.72480211123779,0.343302848161179,-0.430536906388051));
#49924=CARTESIAN_POINT('Ctrl Pts',(0.760825170491265,0.217005158150775,
-0.435822743246699));
#49925=CARTESIAN_POINT('Ctrl Pts',(0.796848229744735,0.0907074681403859,
-0.441108580105346));
#49926=CARTESIAN_POINT('Ctrl Pts',(0.80074469853044,-0.0447534779111776,
-0.446394416963993));
#49927=CARTESIAN_POINT('Ctrl Pts',(0.772040978359756,-0.172913002518913,
-0.451680253822641));
#49928=CARTESIAN_POINT('Ctrl Pts',(0.743337258189069,-0.301072527126663,
-0.456966090681289));
#49929=CARTESIAN_POINT('Ctrl Pts',(0.682033349061983,-0.421930630290567,
-0.462251927539937));
#49930=CARTESIAN_POINT('Ctrl Pts',(0.595580469361028,-0.520797545336097,
-0.467537764398585));
#49931=CARTESIAN_POINT('Ctrl Pts',(0.509127589660082,-0.619664460381615,
-0.472823601257233));
#49932=CARTESIAN_POINT('Ctrl Pts',(0.397525739385269,-0.696540187308768,
-0.47810943811588));
#49933=CARTESIAN_POINT('Ctrl Pts',(0.274339628708118,-0.742080822303308,
-0.483395274974527));
#49934=CARTESIAN_POINT('Ctrl Pts',(0.151153518030953,-0.787621457297853,
-0.488681111833175));
#49935=CARTESIAN_POINT('Ctrl Pts',(0.0163831469514432,-0.80182700035978,
-0.493966948691824));
#49936=CARTESIAN_POINT('Ctrl Pts',(-0.113590743369394,-0.782970830702836,
-0.499252785550472));
#49937=CARTESIAN_POINT('Ctrl Pts',(-0.243564633690224,-0.764114661045893,
-0.50453862240912));
#49938=CARTESIAN_POINT('Ctrl Pts',(-0.368742043252385,-0.712196778670083,
-0.509824459267768));
#49939=CARTESIAN_POINT('Ctrl Pts',(-0.473908212837532,-0.633527572024988,
-0.515110296126416));
#49940=CARTESIAN_POINT('Ctrl Pts',(-0.57907438242268,-0.554858365379893,
-0.520396132985063));
#49941=CARTESIAN_POINT('Ctrl Pts',(-0.664229312030816,-0.44943783446551,
-0.525681969843711));
#49942=CARTESIAN_POINT('Ctrl Pts',(-0.719022797463125,-0.330079377481899,
-0.530967806702359));
#49943=CARTESIAN_POINT('Ctrl Pts',(-0.766357987979791,-0.226967570366176,
-0.535534154193671));
#49944=CARTESIAN_POINT('Ctrl Pts',(-0.791034591140219,-0.113453961755914,
-0.540100501684984));
#49945=CARTESIAN_POINT('Ctrl Pts',(-0.791138066768001,1.60959521169762E-5,
-0.544666849176297));
#49946=CARTESIAN_POINT('Ctrl Pts',(-0.791122640286116,1.87499586476574E-5,
-0.573133150823702));
#49947=CARTESIAN_POINT('Ctrl Pts',(-0.791014041611268,-0.108239976577143,
-0.568776767003377));
#49948=CARTESIAN_POINT('Ctrl Pts',(-0.768616759905835,-0.216542250831125,
-0.564420383183053));
#49949=CARTESIAN_POINT('Ctrl Pts',(-0.7254134058197,-0.315787218355868,
-0.560063999362727));
#49950=CARTESIAN_POINT('Ctrl Pts',(-0.672992432171727,-0.436206522304726,
-0.554778162504079));
#49951=CARTESIAN_POINT('Ctrl Pts',(-0.589940164630051,-0.543291400647814,
-0.549492325645431));
#49952=CARTESIAN_POINT('Ctrl Pts',(-0.486351238141156,-0.624026161133036,
-0.544206488786784));
#49953=CARTESIAN_POINT('Ctrl Pts',(-0.38276231165226,-0.704760921618259,
-0.538920651928136));
#49954=CARTESIAN_POINT('Ctrl Pts',(-0.258636726216144,-0.759145564245615,
-0.533634815069489));
#49955=CARTESIAN_POINT('Ctrl Pts',(-0.129061396490065,-0.780569876792528,
-0.528348978210841));
#49956=CARTESIAN_POINT('Ctrl Pts',(0.000513933236015063,-0.801994189339442,
-0.523063141352193));
#49957=CARTESIAN_POINT('Ctrl Pts',(0.135539007252059,-0.790458171805913,
-0.517777304493544));
#49958=CARTESIAN_POINT('Ctrl Pts',(0.259602126381619,-0.747363975983607,
-0.512491467634897));
#49959=CARTESIAN_POINT('Ctrl Pts',(0.383665245511179,-0.704269780161301,
-0.507205630776248));
#49960=CARTESIAN_POINT('Ctrl Pts',(0.496766409754256,-0.629617406050217,
-0.501919793917601));
#49961=CARTESIAN_POINT('Ctrl Pts',(0.585158673978075,-0.532480518787361,
-0.496633957058954));
#49962=CARTESIAN_POINT('Ctrl Pts',(0.67355093820189,-0.435343631524511,
-0.491348120200306));
#49963=CARTESIAN_POINT('Ctrl Pts',(0.737234302406452,-0.31572223110989,
-0.486062283341658));
#49964=CARTESIAN_POINT('Ctrl Pts',(0.768468335982814,-0.188155768478525,
-0.480776446483011));
#49965=CARTESIAN_POINT('Ctrl Pts',(0.799702369559179,-0.0605893058471451,
-0.475490609624363));
#49966=CARTESIAN_POINT('Ctrl Pts',(0.798487072507338,0.0749222190009814,
-0.470204772765715));
#49967=CARTESIAN_POINT('Ctrl Pts',(0.764970158796818,0.201907980947109,
-0.464918935907067));
#49968=CARTESIAN_POINT('Ctrl Pts',(0.731453245086298,0.32889374289323,-0.459633099048419));
#49969=CARTESIAN_POINT('Ctrl Pts',(0.665634714717104,0.447353741937353,
-0.45434726218977));
#49970=CARTESIAN_POINT('Ctrl Pts',(0.575514518279434,0.542889690332724,
-0.449061425331122));
#49971=CARTESIAN_POINT('Ctrl Pts',(0.485394321841764,0.638425638728095,
-0.443775588472475));
#49972=CARTESIAN_POINT('Ctrl Pts',(0.370972459335619,0.711037536474715,
-0.438489751613827));
#49973=CARTESIAN_POINT('Ctrl Pts',(0.246156400914278,0.751899729291653,
-0.43320391475518));
#49974=CARTESIAN_POINT('Ctrl Pts',(0.121340342492937,0.79276192210859,-0.427918077896532));
#49975=CARTESIAN_POINT('Ctrl Pts',(-0.0138699118435993,0.801874409995844,
-0.422632241037884));
#49976=CARTESIAN_POINT('Ctrl Pts',(-0.143040155074307,0.778129610447774,
-0.417346404179236));
#49977=CARTESIAN_POINT('Ctrl Pts',(-0.272210398305008,0.754384810899704,
-0.412060567320588));
#49978=CARTESIAN_POINT('Ctrl Pts',(-0.395340630429881,0.697782723916312,
-0.406774730461941));
#49979=CARTESIAN_POINT('Ctrl Pts',(-0.497464917569459,0.615203082249481,
-0.401488893603293));
#49980=CARTESIAN_POINT('Ctrl Pts',(-0.599589204709056,0.532623440582635,
-0.396203056744645));
#49981=CARTESIAN_POINT('Ctrl Pts',(-0.68070754686335,0.424066244232339,
-0.390917219885996));
#49982=CARTESIAN_POINT('Ctrl Pts',(-0.730960369152815,0.302726139181895,
-0.385631383027348));
#49983=CARTESIAN_POINT('Ctrl Pts',(-0.770567559629172,0.207090900518661,
-0.381465305626133));
#49984=CARTESIAN_POINT('Ctrl Pts',(-0.791001278485662,0.103514997377555,
-0.377299228224918));
#49985=CARTESIAN_POINT('Ctrl Pts',(-0.791107814146002,-2.00951009365201E-5,
-0.373133150823702));
#49986=CARTESIAN_POINT('Origin',(0.,0.,-2.94));
#49987=CARTESIAN_POINT('',(-0.791053554504038,1.52922707510328E-5,-0.144666849176299));
#49988=CARTESIAN_POINT('',(-0.79104322765544,1.14479096649424E-5,-0.173133150823705));
#49989=CARTESIAN_POINT('',(-0.7911,-9.68818082805471E-17,-2.94));
#49990=CARTESIAN_POINT('Ctrl Pts',(-0.791053554504038,1.52922707510328E-5,
-0.144666849176299));
#49991=CARTESIAN_POINT('Ctrl Pts',(-0.791085703591015,0.0474147764528999,
-0.146573750410772));
#49992=CARTESIAN_POINT('Ctrl Pts',(-0.786893588218416,0.094808539727534,
-0.148480651645245));
#49993=CARTESIAN_POINT('Ctrl Pts',(-0.778423925444021,0.141425176396593,
-0.150387552879717));
#49994=CARTESIAN_POINT('Ctrl Pts',(-0.754946434914425,0.270644210857813,
-0.155673389738365));
#49995=CARTESIAN_POINT('Ctrl Pts',(-0.698601499670502,0.393892027855944,
-0.160959226597013));
#49996=CARTESIAN_POINT('Ctrl Pts',(-0.616234303656779,0.496187532009763,
-0.16624506345566));
#49997=CARTESIAN_POINT('Ctrl Pts',(-0.533867107643055,0.598483036163582,
-0.171530900314307));
#49998=CARTESIAN_POINT('Ctrl Pts',(-0.425477650859533,0.679826227473085,
-0.176816737172955));
#49999=CARTESIAN_POINT('Ctrl Pts',(-0.304241876441027,0.730330646536183,
-0.182102574031602));
#50000=CARTESIAN_POINT('Ctrl Pts',(-0.183006102022508,0.780835065599286,
-0.18738841089025));
#50001=CARTESIAN_POINT('Ctrl Pts',(-0.0489240099689825,0.800500712415977,
-0.1926742477489));
#50002=CARTESIAN_POINT('Ctrl Pts',(0.0817081782642248,0.786937087104024,
-0.197960084607548));
#50003=CARTESIAN_POINT('Ctrl Pts',(0.212340366497417,0.773373461792073,
-0.203245921466195));
#50004=CARTESIAN_POINT('Ctrl Pts',(0.339522650910292,0.726580564351502,
-0.208531758324842));
#50005=CARTESIAN_POINT('Ctrl Pts',(0.44779614723485,0.652245980563451,-0.213817595183489));
#50006=CARTESIAN_POINT('Ctrl Pts',(0.55606964355942,0.577911396775392,-0.219103432042137));
#50007=CARTESIAN_POINT('Ctrl Pts',(0.645434351795641,0.476035126639855,
-0.224389268900785));
#50008=CARTESIAN_POINT('Ctrl Pts',(0.705028613724712,0.358999719529879,
-0.229675105759433));
#50009=CARTESIAN_POINT('Ctrl Pts',(0.764622875653779,0.24196431241991,-0.234960942618081));
#50010=CARTESIAN_POINT('Ctrl Pts',(0.7944466912757,0.109769768335487,-0.24024677947673));
#50011=CARTESIAN_POINT('Ctrl Pts',(0.790874992389185,-0.0215162213875797,
-0.245532616335378));
#50012=CARTESIAN_POINT('Ctrl Pts',(0.78730329350267,-0.152802211110639,
-0.250818453194026));
#50013=CARTESIAN_POINT('Ctrl Pts',(0.750336080107733,-0.283179646472356,
-0.256104290052673));
#50014=CARTESIAN_POINT('Ctrl Pts',(0.68446661229184,-0.396801743794359,
-0.261390126911321));
#50015=CARTESIAN_POINT('Ctrl Pts',(0.618597144475944,-0.510423841116369,
-0.266675963769968));
#50016=CARTESIAN_POINT('Ctrl Pts',(0.523825422239093,-0.607290600398658,
-0.271961800628616));
#50017=CARTESIAN_POINT('Ctrl Pts',(0.411670498006626,-0.675628288467962,
-0.277247637487264));
#50018=CARTESIAN_POINT('Ctrl Pts',(0.299515573774159,-0.743965976537265,
-0.282533474345911));
#50019=CARTESIAN_POINT('Ctrl Pts',(0.16997744754608,-0.783774593393581,
-0.28781931120456));
#50020=CARTESIAN_POINT('Ctrl Pts',(0.0388009198198214,-0.790215582223114,
-0.293105148063208));
#50021=CARTESIAN_POINT('Ctrl Pts',(-0.0923756079064444,-0.796656571052647,
-0.298390984921856));
#50022=CARTESIAN_POINT('Ctrl Pts',(-0.225190537130885,-0.769729931855394,
-0.303676821780504));
#50023=CARTESIAN_POINT('Ctrl Pts',(-0.343500809912295,-0.71270847616472,
-0.308962658639152));
#50024=CARTESIAN_POINT('Ctrl Pts',(-0.461811082693692,-0.655687020474052,
-0.3142484954978));
#50025=CARTESIAN_POINT('Ctrl Pts',(-0.565616699032059,-0.568570748289972,
-0.319534332356447));
#50026=CARTESIAN_POINT('Ctrl Pts',(-0.642300542374549,-0.461948257379328,
-0.324820169215095));
#50027=CARTESIAN_POINT('Ctrl Pts',(-0.71898438571704,-0.355325766468685,
-0.330106006073742));
#50028=CARTESIAN_POINT('Ctrl Pts',(-0.768546456063654,-0.229197056831479,
-0.335391842932389));
#50029=CARTESIAN_POINT('Ctrl Pts',(-0.784962705552036,-0.0988925134430879,
-0.340677679791037));
#50030=CARTESIAN_POINT('Ctrl Pts',(-0.789092433201673,-0.0661126585751875,
-0.342007402919458));
#50031=CARTESIAN_POINT('Ctrl Pts',(-0.791124555828957,-0.033068539627467,
-0.343337126047879));
#50032=CARTESIAN_POINT('Ctrl Pts',(-0.791091445179114,-2.03764682111252E-5,
-0.3446668491763));
#50033=CARTESIAN_POINT('Ctrl Pts',(-0.791107814146002,-2.00951009365201E-5,
-0.373133150823702));
#50034=CARTESIAN_POINT('Ctrl Pts',(-0.791136448830798,-0.0278482864218827,
-0.37201339136627));
#50035=CARTESIAN_POINT('Ctrl Pts',(-0.789696590075878,-0.055673529464667,
-0.370893631908838));
#50036=CARTESIAN_POINT('Ctrl Pts',(-0.786765835743427,-0.0833408443281345,
-0.369773872451406));
#50037=CARTESIAN_POINT('Ctrl Pts',(-0.772931177619944,-0.21394470903718,
-0.364488035592758));
#50038=CARTESIAN_POINT('Ctrl Pts',(-0.725874558948336,-0.341029424704697,
-0.35920219873411));
#50039=CARTESIAN_POINT('Ctrl Pts',(-0.651315503160049,-0.449148407495439,
-0.353916361875462));
#50040=CARTESIAN_POINT('Ctrl Pts',(-0.576756447371763,-0.557267390286181,
-0.348630525016814));
#50041=CARTESIAN_POINT('Ctrl Pts',(-0.474694954466797,-0.646420640200151,
-0.343344688158166));
#50042=CARTESIAN_POINT('Ctrl Pts',(-0.357536146397053,-0.70577197496111,
-0.338058851299519));
#50043=CARTESIAN_POINT('Ctrl Pts',(-0.240377338327316,-0.765123309722065,
-0.332773014440872));
#50044=CARTESIAN_POINT('Ctrl Pts',(-0.1081212150928,-0.794672729330014,
-0.327487177582224));
#50045=CARTESIAN_POINT('Ctrl Pts',(0.0231570776879453,-0.79082863276307,
-0.322201340723576));
#50046=CARTESIAN_POINT('Ctrl Pts',(0.154435370468698,-0.786984536196125,
-0.316915503864928));
#50047=CARTESIAN_POINT('Ctrl Pts',(0.284735832795685,-0.749746923454283,
-0.31162966700628));
#50048=CARTESIAN_POINT('Ctrl Pts',(0.398221021362254,-0.683641861411983,
-0.306343830147633));
#50049=CARTESIAN_POINT('Ctrl Pts',(0.511706209928824,-0.617536799369684,
-0.301057993288985));
#50050=CARTESIAN_POINT('Ctrl Pts',(0.608376124734981,-0.522564288026924,
-0.295772156430336));
#50051=CARTESIAN_POINT('Ctrl Pts',(0.676480965662377,-0.410267814884783,
-0.290486319571689));
#50052=CARTESIAN_POINT('Ctrl Pts',(0.744585806589778,-0.297971341742634,
-0.285200482713041));
#50053=CARTESIAN_POINT('Ctrl Pts',(0.784125573638418,-0.168350906801097,
-0.279914645854393));
#50054=CARTESIAN_POINT('Ctrl Pts',(0.79029438440916,-0.0371612997782024,
-0.274628808995745));
#50055=CARTESIAN_POINT('Ctrl Pts',(0.796463195179903,0.0940283072446845,
-0.269342972137097));
#50056=CARTESIAN_POINT('Ctrl Pts',(0.769261049672759,0.226787086348913,
-0.26405713527845));
#50057=CARTESIAN_POINT('Ctrl Pts',(0.71199424612376,0.344978797360926,-0.258771298419802));
#50058=CARTESIAN_POINT('Ctrl Pts',(0.65472744257476,0.463170508372939,-0.253485461561154));
#50059=CARTESIAN_POINT('Ctrl Pts',(0.567395980983906,0.566795151292719,
-0.248199624702506));
#50060=CARTESIAN_POINT('Ctrl Pts',(0.460614617197846,0.643257608380992,
-0.242913787843858));
#50061=CARTESIAN_POINT('Ctrl Pts',(0.353833253411787,0.719720065469265,
-0.237627950985211));
#50062=CARTESIAN_POINT('Ctrl Pts',(0.227601987430519,0.769020336726032,
-0.232342114126563));
#50063=CARTESIAN_POINT('Ctrl Pts',(0.0972636625592692,0.785166196174475,
-0.227056277267915));
#50064=CARTESIAN_POINT('Ctrl Pts',(-0.0330746623119731,0.801312055622916,
-0.221770440409268));
#50065=CARTESIAN_POINT('Ctrl Pts',(-0.167520046073201,0.784303503263036,
-0.21648460355062));
#50066=CARTESIAN_POINT('Ctrl Pts',(-0.289731233702443,0.736207846505756,
-0.211198766691972));
#50067=CARTESIAN_POINT('Ctrl Pts',(-0.411942421331698,0.688112189748469,
-0.205912929833324));
#50068=CARTESIAN_POINT('Ctrl Pts',(-0.521919412828967,0.608929428593772,
-0.200627092974676));
#50069=CARTESIAN_POINT('Ctrl Pts',(-0.606295020979308,0.508283889784541,
-0.195341256116028));
#50070=CARTESIAN_POINT('Ctrl Pts',(-0.690670629129644,0.407638350975315,
-0.190055419257381));
#50071=CARTESIAN_POINT('Ctrl Pts',(-0.749444853933058,0.285530034511553,
-0.184769582398733));
#50072=CARTESIAN_POINT('Ctrl Pts',(-0.775473893104923,0.156800639274513,
-0.179483745540085));
#50073=CARTESIAN_POINT('Ctrl Pts',(-0.78589796804693,0.105247262512122,
-0.177366880634625));
#50074=CARTESIAN_POINT('Ctrl Pts',(-0.791070266522022,0.0526319761890897,
-0.175250015729165));
#50075=CARTESIAN_POINT('Ctrl Pts',(-0.79104322765544,1.14479096649424E-5,
-0.173133150823705));
#50076=CARTESIAN_POINT('Origin',(0.,0.,-6.17861797838101));
#50077=CARTESIAN_POINT('',(-0.676660270930202,1.30808743349972E-5,-0.0786179783810092));
#50078=CARTESIAN_POINT('',(-0.6767,7.27977111083166E-14,-0.0710999999999995));
#50079=CARTESIAN_POINT('',(-0.6767,7.27977111083166E-14,-6.17861797838101));
#50080=CARTESIAN_POINT('',(-0.657933807534675,-0.158364149874814,-0.0711000000000017));
#50081=CARTESIAN_POINT('Ctrl Pts',(-0.676660270930202,1.30808743350301E-5,
-0.0786179783810092));
#50082=CARTESIAN_POINT('Ctrl Pts',(-0.676624131187738,-0.053270085543402,
-0.0761119855873401));
#50083=CARTESIAN_POINT('Ctrl Pts',(-0.670347495187715,-0.106561703444771,
-0.0736059927936709));
#50084=CARTESIAN_POINT('Ctrl Pts',(-0.657933807534675,-0.158364149874814,
-0.0711000000000017));
#50085=CARTESIAN_POINT('Origin',(0.,0.,-0.0711000000000004));
#50086=CARTESIAN_POINT('Origin',(0.,0.,-6.17861797838101));
#50087=CARTESIAN_POINT('',(-0.676692682281262,-1.74298521427489E-5,-0.278617978381007));
#50088=CARTESIAN_POINT('',(-0.676651437434504,9.79244154855619E-6,-0.239182021618999));
#50089=CARTESIAN_POINT('',(-0.6767,7.27977111083166E-14,-6.17861797838101));
#50090=CARTESIAN_POINT('Ctrl Pts',(-0.676692682281262,-1.7429852142755E-5,
-0.278617978381007));
#50091=CARTESIAN_POINT('Ctrl Pts',(-0.676721004840672,-0.0282865387004088,
-0.277288255252586));
#50092=CARTESIAN_POINT('Ctrl Pts',(-0.668072916989408,-0.168912128805448,
-0.270672695265517));
#50093=CARTESIAN_POINT('Ctrl Pts',(-0.572617975996934,-0.411831935255785,
-0.258771298419802));
#50094=CARTESIAN_POINT('Ctrl Pts',(-0.306234735283331,-0.635387420227233,
-0.242913787843858));
#50095=CARTESIAN_POINT('Ctrl Pts',(0.0345914406976117,-0.704485853085711,
-0.227056277267915));
#50096=CARTESIAN_POINT('Ctrl Pts',(0.367008771067512,-0.602330028183672,
-0.21119876669197));
#50097=CARTESIAN_POINT('Ctrl Pts',(0.610209470489882,-0.353753099832041,
-0.195341256116028));
#50098=CARTESIAN_POINT('Ctrl Pts',(0.705073760608792,-0.0191819564521373,
-0.179483745540084));
#50099=CARTESIAN_POINT('Ctrl Pts',(0.62854066985661,0.320052203509621,-0.16362623496414));
#50100=CARTESIAN_POINT('Ctrl Pts',(0.399215307462047,0.58148440677362,-0.147768724388197));
#50101=CARTESIAN_POINT('Ctrl Pts',(0.0728434763577143,0.701563108700217,
-0.131911213812254));
#50102=CARTESIAN_POINT('Ctrl Pts',(-0.271234459526246,0.651097643395513,
-0.11605370323631));
#50103=CARTESIAN_POINT('Ctrl Pts',(-0.549380630953683,0.442356886629713,
-0.100196192660368));
#50104=CARTESIAN_POINT('Ctrl Pts',(-0.663161936596271,0.193473868574276,
-0.0877176177086003));
#50105=CARTESIAN_POINT('Ctrl Pts',(-0.676687770977166,0.0405581838272357,
-0.0805248796154809));
#50106=CARTESIAN_POINT('Ctrl Pts',(-0.676660270930202,1.30808743350301E-5,
-0.0786179783810092));
#50107=CARTESIAN_POINT('',(-0.364065050236216,0.570420484551968,-0.0711000000000004));
#50108=CARTESIAN_POINT('Origin',(0.,0.,-0.0711000000000004));
#50109=CARTESIAN_POINT('Ctrl Pts',(-0.676651437434504,9.79244154853884E-6,
-0.239182021618999));
#50110=CARTESIAN_POINT('Ctrl Pts',(-0.676616813331805,-0.0673724171628328,
-0.236013049665811));
#50111=CARTESIAN_POINT('Ctrl Pts',(-0.649932577953111,-0.247174784475467,
-0.227558240853975));
#50112=CARTESIAN_POINT('Ctrl Pts',(-0.493004432164587,-0.504424033259022,
-0.21381759518349));
#50113=CARTESIAN_POINT('Ctrl Pts',(-0.192054423564975,-0.67868406853937,
-0.197960084607548));
#50114=CARTESIAN_POINT('Ctrl Pts',(0.155580900692857,-0.687961374427907,
-0.182102574031604));
#50115=CARTESIAN_POINT('Ctrl Pts',(0.465398645427725,-0.530002638582951,
-0.16624506345566));
#50116=CARTESIAN_POINT('Ctrl Pts',(0.662076718045427,-0.243202481582967,
-0.150387552879718));
#50117=CARTESIAN_POINT('Ctrl Pts',(0.697820336995596,0.102713198692547,
-0.134530042303775));
#50118=CARTESIAN_POINT('Ctrl Pts',(0.563909430812559,0.423669692494884,
-0.11867253172783));
#50119=CARTESIAN_POINT('Ctrl Pts',(0.292957635797326,0.641617108208754,
-0.102815021151888));
#50120=CARTESIAN_POINT('Ctrl Pts',(-0.0492916150247689,0.703631926771629,
-0.0869575105759442));
#50121=CARTESIAN_POINT('Ctrl Pts',(-0.269341331211303,0.630876931084481,
-0.0763858368586482));
#50122=CARTESIAN_POINT('Ctrl Pts',(-0.364065050236216,0.570420484551968,
-0.0711000000000004));
#50123=CARTESIAN_POINT('Origin',(0.,0.,-6.17861797838101));
#50124=CARTESIAN_POINT('',(-0.676732561979404,1.37683363057702E-5,-0.478617978381007));
#50125=CARTESIAN_POINT('',(-0.67670668415194,-1.71891729481843E-5,-0.439182021619));
#50126=CARTESIAN_POINT('',(-0.6767,7.27977111083166E-14,-6.17861797838101));
#50127=CARTESIAN_POINT('Ctrl Pts',(-0.676732561979403,1.3768336305774E-5,
-0.478617978381007));
#50128=CARTESIAN_POINT('Ctrl Pts',(-0.676644049835158,-0.0970475236002888,
-0.474051630889693));
#50129=CARTESIAN_POINT('Ctrl Pts',(-0.631101877637816,-0.306543793263608,
-0.464199446539731));
#50130=CARTESIAN_POINT('Ctrl Pts',(-0.422494366982188,-0.564796775530692,
-0.449061425331123));
#50131=CARTESIAN_POINT('Ctrl Pts',(-0.101267392955972,-0.698027078919814,
-0.433203914755179));
#50132=CARTESIAN_POINT('Ctrl Pts',(0.244576786450544,-0.661573188172743,
-0.417346404179235));
#50133=CARTESIAN_POINT('Ctrl Pts',(0.530966517512247,-0.464296720931165,
-0.401488893603292));
#50134=CARTESIAN_POINT('Ctrl Pts',(0.68828299573105,-0.1541538373096,-0.385631383027349));
#50135=CARTESIAN_POINT('Ctrl Pts',(0.678283980079609,0.193462477415893,
-0.369773872451405));
#50136=CARTESIAN_POINT('Ctrl Pts',(0.503400142512799,0.494049779148767,
-0.353916361875461));
#50137=CARTESIAN_POINT('Ctrl Pts',(0.206144193604109,0.674537959812384,
-0.338058851299519));
#50138=CARTESIAN_POINT('Ctrl Pts',(-0.141223581330571,0.691051943005463,
-0.322201340723575));
#50139=CARTESIAN_POINT('Ctrl Pts',(-0.454261155256553,0.539577325634538,
-0.306343830147631));
#50140=CARTESIAN_POINT('Ctrl Pts',(-0.639882056834951,0.280636962336042,
-0.29181604270011));
#50141=CARTESIAN_POINT('Ctrl Pts',(-0.676608418674978,0.0840871534747274,
-0.282574092111234));
#50142=CARTESIAN_POINT('Ctrl Pts',(-0.676692682281262,-1.7429852142755E-5,
-0.278617978381007));
#50143=CARTESIAN_POINT('Ctrl Pts',(-0.67670668415194,-1.71891729482017E-5,
-0.439182021619));
#50144=CARTESIAN_POINT('Ctrl Pts',(-0.676731178010118,-0.0238211799034624,
-0.438062262161566));
#50145=CARTESIAN_POINT('Ctrl Pts',(-0.669685553243432,-0.159977744463465,
-0.431656665845485));
#50146=CARTESIAN_POINT('Ctrl Pts',(-0.580654911117769,-0.400420729098558,
-0.419965232670754));
#50147=CARTESIAN_POINT('Ctrl Pts',(-0.318747394057519,-0.629203452711689,
-0.404107722094813));
#50148=CARTESIAN_POINT('Ctrl Pts',(0.0206447886986398,-0.705032395634334,
-0.388250211518869));
#50149=CARTESIAN_POINT('Ctrl Pts',(0.355018405902544,-0.609474213827725,
-0.372392700942925));
#50150=CARTESIAN_POINT('Ctrl Pts',(0.603090197140036,-0.365758254686112,
-0.356535190366982));
#50151=CARTESIAN_POINT('Ctrl Pts',(0.704556106741155,-0.0331297058619517,
-0.340677679791039));
#50152=CARTESIAN_POINT('Ctrl Pts',(0.634750676840949,0.307552379158318,
-0.324820169215095));
#50153=CARTESIAN_POINT('Ctrl Pts',(0.410642978477166,0.573471210647949,
-0.308962658639151));
#50154=CARTESIAN_POINT('Ctrl Pts',(0.0867116258434061,0.699984269273112,
-0.293105148063209));
#50155=CARTESIAN_POINT('Ctrl Pts',(-0.258298579659923,0.656337369834618,
-0.277247637487264));
#50156=CARTESIAN_POINT('Ctrl Pts',(-0.540518640889337,0.453140652074363,
-0.261390126911321));
#50157=CARTESIAN_POINT('Ctrl Pts',(-0.661202601018511,0.2024097365269,-0.248701588288566));
#50158=CARTESIAN_POINT('Ctrl Pts',(-0.676674566243774,0.0450209307131661,
-0.241298886524459));
#50159=CARTESIAN_POINT('Ctrl Pts',(-0.676651437434504,9.79244154853884E-6,
-0.239182021618999));
#50160=CARTESIAN_POINT('Origin',(0.,0.,-6.17861797838101));
#50161=CARTESIAN_POINT('',(-0.676642928030041,-2.47388173200321E-6,-0.678617978381005));
#50162=CARTESIAN_POINT('',(-0.676719366302129,1.60385502095753E-5,-0.639182021618998));
#50163=CARTESIAN_POINT('',(-0.6767,7.27977111083166E-14,-6.17861797838101));
#50164=CARTESIAN_POINT('Ctrl Pts',(-0.676642928030041,-2.47388173194724E-6,
-0.678617978381005));
#50165=CARTESIAN_POINT('Ctrl Pts',(-0.676649761854052,-0.0535265248175451,
-0.676100843385447));
#50166=CARTESIAN_POINT('Ctrl Pts',(-0.657200799107262,-0.219443081072225,
-0.66829787153124));
#50167=CARTESIAN_POINT('Ctrl Pts',(-0.523043611653193,-0.47320425620448,
-0.655209062818387));
#50168=CARTESIAN_POINT('Ctrl Pts',(-0.233360621587032,-0.66561228059116,
-0.639351552242444));
#50169=CARTESIAN_POINT('Ctrl Pts',(0.113050266597516,-0.696215860924957,
-0.6234940416665));
#50170=CARTESIAN_POINT('Ctrl Pts',(0.431979637282727,-0.55757553815993,
-0.607636531090557));
#50171=CARTESIAN_POINT('Ctrl Pts',(0.645898588102162,-0.283393545566738,
-0.591779020514614));
#50172=CARTESIAN_POINT('Ctrl Pts',(0.702805318729989,0.0596789053693757,
-0.57592150993867));
#50173=CARTESIAN_POINT('Ctrl Pts',(0.588866307489121,0.388243943526985,
-0.560063999362727));
#50174=CARTESIAN_POINT('Ctrl Pts',(0.331779117822002,0.622430321207524,
-0.544206488786783));
#50175=CARTESIAN_POINT('Ctrl Pts',(-0.00596063381383579,0.705309406307461,
-0.52834897821084));
#50176=CARTESIAN_POINT('Ctrl Pts',(-0.34225140821695,0.616734028050019,
-0.512491467634896));
#50177=CARTESIAN_POINT('Ctrl Pts',(-0.595343899704099,0.378236075574855,
-0.496633957058954));
#50178=CARTESIAN_POINT('Ctrl Pts',(-0.672507309873267,0.142947270699369,
-0.485342793974323));
#50179=CARTESIAN_POINT('Ctrl Pts',(-0.676746508256332,0.0153070782871879,
-0.479337467748341));
#50180=CARTESIAN_POINT('Ctrl Pts',(-0.676732561979403,1.3768336305774E-5,
-0.478617978381007));
#50181=CARTESIAN_POINT('Ctrl Pts',(-0.676719366302129,1.60385502095822E-5,
-0.639182021618998));
#50182=CARTESIAN_POINT('Ctrl Pts',(-0.676626471948366,-0.0925875264185486,
-0.634825637798672));
#50183=CARTESIAN_POINT('Ctrl Pts',(-0.634222060982391,-0.297634469454627,
-0.625183417119698));
#50184=CARTESIAN_POINT('Ctrl Pts',(-0.433587460447112,-0.556326163561039,
-0.610255359582076));
#50185=CARTESIAN_POINT('Ctrl Pts',(-0.11505964981147,-0.695886602188015,
-0.594397849006135));
#50186=CARTESIAN_POINT('Ctrl Pts',(0.231438141567586,-0.66628317759591,
-0.578540338430189));
#50187=CARTESIAN_POINT('Ctrl Pts',(0.521675372676006,-0.474712219837212,
-0.562682827854247));
#50188=CARTESIAN_POINT('Ctrl Pts',(0.685097945892652,-0.167742930263535,
-0.546825317278303));
#50189=CARTESIAN_POINT('Ctrl Pts',(0.681979282582143,0.180003178438481,
-0.53096780670236));
#50190=CARTESIAN_POINT('Ctrl Pts',(0.513077502146677,0.483992110380683,
-0.515110296126415));
#50191=CARTESIAN_POINT('Ctrl Pts',(0.219451129913428,0.670326851393724,
-0.499252785550473));
#50192=CARTESIAN_POINT('Ctrl Pts',(-0.127521866330539,0.693711077989502,
-0.483395274974529));
#50193=CARTESIAN_POINT('Ctrl Pts',(-0.443495427494386,0.54846029201429,
-0.467537764398586));
#50194=CARTESIAN_POINT('Ctrl Pts',(-0.636959943577643,0.28955503210012,
-0.452800013280076));
#50195=CARTESIAN_POINT('Ctrl Pts',(-0.676615554482665,0.088545820661681,
-0.443348099020214));
#50196=CARTESIAN_POINT('Ctrl Pts',(-0.67670668415194,-1.71891729482017E-5,
-0.439182021619));
#50197=CARTESIAN_POINT('Origin',(0.,0.,-6.17861797838101));
#50198=CARTESIAN_POINT('',(-0.676745967174656,-9.80469378314186E-6,-0.878617978381005));
#50199=CARTESIAN_POINT('',(-0.676646131014468,-6.47238999015864E-6,-0.839182021618998));
#50200=CARTESIAN_POINT('',(-0.6767,7.27977111083166E-14,-6.17861797838101));
#50201=CARTESIAN_POINT('Ctrl Pts',(-0.676745967174656,-9.80469378311123E-6,
-0.878617978381005));
#50202=CARTESIAN_POINT('Ctrl Pts',(-0.676752985825416,-0.00995529331039852,
-0.878150055881202));
#50203=CARTESIAN_POINT('Ctrl Pts',(-0.674112766541405,-0.132245209733512,
-0.87239629652275));
#50204=CARTESIAN_POINT('Ctrl Pts',(-0.604143565385745,-0.364015714199608,
-0.861356700305653));
#50205=CARTESIAN_POINT('Ctrl Pts',(-0.356776373766072,-0.608446798745448,
-0.845499189729708));
#50206=CARTESIAN_POINT('Ctrl Pts',(-0.0226800088848199,-0.704969861042468,
-0.829641679153765));
#50207=CARTESIAN_POINT('Ctrl Pts',(0.316929665073997,-0.630121000425581,
-0.813784168577821));
#50208=CARTESIAN_POINT('Ctrl Pts',(0.579496547370947,-0.40209531129622,
-0.797926658001879));
#50209=CARTESIAN_POINT('Ctrl Pts',(0.701192956853533,-0.0763238169921492,
-0.782069147425935));
#50210=CARTESIAN_POINT('Ctrl Pts',(0.652435575344282,0.268001320531126,
-0.76621163684999));
#50211=CARTESIAN_POINT('Ctrl Pts',(0.445076890002194,0.547177713149235,
-0.750354126274048));
#50212=CARTESIAN_POINT('Ctrl Pts',(0.129523958779256,0.693340055011537,
-0.734496615698105));
#50213=CARTESIAN_POINT('Ctrl Pts',(-0.217515098455649,0.670957576695487,
-0.718639105122159));
#50214=CARTESIAN_POINT('Ctrl Pts',(-0.511678163758033,0.485471260235309,
-0.702781594546218));
#50215=CARTESIAN_POINT('Ctrl Pts',(-0.654507065922775,0.230147136195413,
-0.689441218965832));
#50216=CARTESIAN_POINT('Ctrl Pts',(-0.676635411221723,0.0588708641822061,
-0.681386680244095));
#50217=CARTESIAN_POINT('Ctrl Pts',(-0.676642928030041,-2.47388173194724E-6,
-0.678617978381005));
#50218=CARTESIAN_POINT('Ctrl Pts',(-0.676646131014468,-6.47238999016905E-6,
-0.839182021618998));
#50219=CARTESIAN_POINT('Ctrl Pts',(-0.676662613967231,-0.0490652167404076,
-0.836874850294427));
#50220=CARTESIAN_POINT('Ctrl Pts',(-0.659343207714862,-0.210508362902118,
-0.829281842111208));
#50221=CARTESIAN_POINT('Ctrl Pts',(-0.532304648268198,-0.462761977210308,
-0.816402997069341));
#50222=CARTESIAN_POINT('Ctrl Pts',(-0.246485614000569,-0.660864379589555,
-0.800545486493398));
#50223=CARTESIAN_POINT('Ctrl Pts',(0.0992518876742048,-0.698316510554226,
-0.784687975917454));
#50224=CARTESIAN_POINT('Ctrl Pts',(0.420862135428632,-0.566014089119677,
-0.76883046534151));
#50225=CARTESIAN_POINT('Ctrl Pts',(0.64016452944956,-0.296118660935354,
-0.752972954765568));
#50226=CARTESIAN_POINT('Ctrl Pts',(0.703848602098822,0.0457605883163558,
-0.737115444189624));
#50227=CARTESIAN_POINT('Ctrl Pts',(0.596433319942227,0.37651584426451,-0.721257933613681));
#50228=CARTESIAN_POINT('Ctrl Pts',(0.34403038572165,0.615743436684253,-0.705400423037737));
#50229=CARTESIAN_POINT('Ctrl Pts',(0.0079967149263957,0.705289258864694,
-0.689542912461795));
#50230=CARTESIAN_POINT('Ctrl Pts',(-0.329980886368106,0.623385515352452,
-0.67368540188585));
#50231=CARTESIAN_POINT('Ctrl Pts',(-0.58774305981707,0.389942280031795,
-0.657827891309908));
#50232=CARTESIAN_POINT('Ctrl Pts',(-0.671068275265414,0.151880359453098,
-0.64632676455429));
#50233=CARTESIAN_POINT('Ctrl Pts',(-0.676739185708065,0.0197734034587098,
-0.64011147465732));
#50234=CARTESIAN_POINT('Ctrl Pts',(-0.676719366302129,1.60385502095822E-5,
-0.639182021618998));
#50235=CARTESIAN_POINT('Origin',(0.,0.,-6.17861797838101));
#50236=CARTESIAN_POINT('',(-0.676676906654629,1.63404783267962E-5,-1.078617978381));
#50237=CARTESIAN_POINT('',(-0.676753912310732,-5.67166874843039E-6,-1.039182021619));
#50238=CARTESIAN_POINT('',(-0.6767,7.27977111083166E-14,-6.17861797838101));
#50239=CARTESIAN_POINT('Ctrl Pts',(-0.676676906654629,1.63404783268123E-5,
-1.078617978381));
#50240=CARTESIAN_POINT('Ctrl Pts',(-0.676605761560008,-0.0787453581397193,
-1.07491343151831));
#50241=CARTESIAN_POINT('Ctrl Pts',(-0.643248328946388,-0.269946967027055,
-1.06592304779696));
#50242=CARTESIAN_POINT('Ctrl Pts',(-0.466925454985086,-0.528656322451762,
-1.05164682721697));
#50243=CARTESIAN_POINT('Ctrl Pts',(-0.157566931955473,-0.687509672466789,
-1.03578931664103));
#50244=CARTESIAN_POINT('Ctrl Pts',(0.190094715234546,-0.679235516607566,
-1.01993180606508));
#50245=CARTESIAN_POINT('Ctrl Pts',(0.491546022542315,-0.505845228804307,
-1.00407429548914));
#50246=CARTESIAN_POINT('Ctrl Pts',(0.673506849846877,-0.209488450733178,
-0.988216784913199));
#50247=CARTESIAN_POINT('Ctrl Pts',(0.691744133306218,0.137793112373883,
-0.972359274337254));
#50248=CARTESIAN_POINT('Ctrl Pts',(0.541824551004231,0.45157839154494,-0.956501763761313));
#50249=CARTESIAN_POINT('Ctrl Pts',(0.260192224202427,0.655588967452813,
-0.940644253185368));
#50250=CARTESIAN_POINT('Ctrl Pts',(-0.0846905254229573,0.700231677864431,
-0.924786742609425));
#50251=CARTESIAN_POINT('Ctrl Pts',(-0.408985759189344,0.574654275683705,
-0.908929232033481));
#50252=CARTESIAN_POINT('Ctrl Pts',(-0.627224599629542,0.317211108211441,
-0.893539643957343));
#50253=CARTESIAN_POINT('Ctrl Pts',(-0.676673700381987,0.102392863337454,
-0.88343589273985));
#50254=CARTESIAN_POINT('Ctrl Pts',(-0.676745967174656,-9.80469378311123E-6,
-0.878617978381005));
#50255=CARTESIAN_POINT('Ctrl Pts',(-0.676753912310732,-5.67166874834366E-6,
-1.039182021619));
#50256=CARTESIAN_POINT('Ctrl Pts',(-0.676756347097398,-0.00548828706568831,
-1.03892406279018));
#50257=CARTESIAN_POINT('Ctrl Pts',(-0.675354290426282,-0.123313979218898,
-1.03338026710272));
#50258=CARTESIAN_POINT('Ctrl Pts',(-0.61122817502222,-0.35199006261332,
-1.0225506345566));
#50259=CARTESIAN_POINT('Ctrl Pts',(-0.368746051047842,-0.601268023394017,
-1.00669312398066));
#50260=CARTESIAN_POINT('Ctrl Pts',(-0.0366250313885693,-0.704383058566367,
-0.990835613404718));
#50261=CARTESIAN_POINT('Ctrl Pts',(0.304399208681507,-0.636268817304129,
-0.974978102828775));
#50262=CARTESIAN_POINT('Ctrl Pts',(0.571426699942949,-0.413483267753163,
-0.959120592252834));
#50263=CARTESIAN_POINT('Ctrl Pts',(0.699545426752022,-0.0901836017791227,
-0.943263081676888));
#50264=CARTESIAN_POINT('Ctrl Pts',(0.657610862529838,0.25503889821415,-0.927405571100947));
#50265=CARTESIAN_POINT('Ctrl Pts',(0.455816928044417,0.538263703241892,
-0.911548060525));
#50266=CARTESIAN_POINT('Ctrl Pts',(0.14321793965191,0.690641374290149,-0.89569054994906));
#50267=CARTESIAN_POINT('Ctrl Pts',(-0.204196060091041,0.675130250516757,
-0.879833039373114));
#50268=CARTESIAN_POINT('Ctrl Pts',(-0.501971808040508,0.495500948588465,
-0.863975528797173));
#50269=CARTESIAN_POINT('Ctrl Pts',(-0.652151980137971,0.239079746805326,
-0.850425189545799));
#50270=CARTESIAN_POINT('Ctrl Pts',(-0.676624850755489,0.0633306492989827,
-0.842160687153075));
#50271=CARTESIAN_POINT('Ctrl Pts',(-0.676646131014468,-6.47238999016905E-6,
-0.839182021618998));
#50272=CARTESIAN_POINT('Origin',(0.,0.,-6.17861797838101));
#50273=CARTESIAN_POINT('',(-0.676672623201375,-1.57520597928919E-5,-1.278617978381));
#50274=CARTESIAN_POINT('',(-0.676665319626825,1.43824383198043E-5,-1.239182021619));
#50275=CARTESIAN_POINT('',(-0.6767,7.27977111083166E-14,-6.17861797838101));
#50276=CARTESIAN_POINT('Ctrl Pts',(-0.676672623201375,-1.57520597928451E-5,
-1.278617978381));
#50277=CARTESIAN_POINT('Ctrl Pts',(-0.676702974356069,-0.0352101549393811,
-1.27696264401406));
#50278=CARTESIAN_POINT('Ctrl Pts',(-0.665389827098819,-0.182768491112835,
-1.27002147278847));
#50279=CARTESIAN_POINT('Ctrl Pts',(-0.559711989719446,-0.429207847488311,
-1.25779446470423));
#50280=CARTESIAN_POINT('Ctrl Pts',(-0.286594754496667,-0.644484549447267,
-1.2419369541283));
#50281=CARTESIAN_POINT('Ctrl Pts',(0.0561911245777891,-0.703092771474672,
-1.22607944355235));
#50282=CARTESIAN_POINT('Ctrl Pts',(0.385317439461293,-0.590785374419714,
-1.21022193297641));
#50283=CARTESIAN_POINT('Ctrl Pts',(0.620776501059534,-0.33486329078227,
-1.19436442240046));
#50284=CARTESIAN_POINT('Ctrl Pts',(0.705330299092296,0.00246108992610756,
-1.17850691182452));
#50285=CARTESIAN_POINT('Ctrl Pts',(0.618424554916906,0.339187201493628,
-1.16264940124858));
#50286=CARTESIAN_POINT('Ctrl Pts',(0.381185284430804,0.593459911632335,
-1.14679189067263));
#50287=CARTESIAN_POINT('Ctrl Pts',(0.0512832509114107,0.703467778904769,
-1.13093438009669));
#50288=CARTESIAN_POINT('Ctrl Pts',(-0.291085286224135,0.642468866113421,
-1.11507686952075));
#50289=CARTESIAN_POINT('Ctrl Pts',(-0.562693571058386,0.425291468137809,
-1.0992193589448));
#50290=CARTESIAN_POINT('Ctrl Pts',(-0.66601953362321,0.179617462040716,
-1.08706639523156));
#50291=CARTESIAN_POINT('Ctrl Pts',(-0.676707275018306,0.0336358601402424,
-1.08019926837696));
#50292=CARTESIAN_POINT('Ctrl Pts',(-0.676676906654629,1.63404783268123E-5,
-1.078617978381));
#50293=CARTESIAN_POINT('Ctrl Pts',(-0.676665319626825,1.43824383197974E-5,
-1.239182021619));
#50294=CARTESIAN_POINT('Ctrl Pts',(-0.676607727494747,-0.0742869656269988,
-1.23568743842729));
#50295=CARTESIAN_POINT('Ctrl Pts',(-0.645946489283497,-0.261021420873604,
-1.22690701837693));
#50296=CARTESIAN_POINT('Ctrl Pts',(-0.477294726647991,-0.519313614334867,
-1.21284076146793));
#50297=CARTESIAN_POINT('Ctrl Pts',(-0.171140054664367,-0.684257238039178,
-1.19698325089199));
#50298=CARTESIAN_POINT('Ctrl Pts',(0.176617247270067,-0.682863993842307,
-1.18112574031604));
#50299=CARTESIAN_POINT('Ctrl Pts',(0.481440462292368,-0.515472567055936,
-1.1652682297401));
#50300=CARTESIAN_POINT('Ctrl Pts',(0.669229769411713,-0.222774329429288,
-1.14941071916415));
#50301=CARTESIAN_POINT('Ctrl Pts',(0.694335253018772,0.124078372550911,
-1.13355320858821));
#50302=CARTESIAN_POINT('Ctrl Pts',(0.550653992635405,0.440768722250355,
-1.11769569801226));
#50303=CARTESIAN_POINT('Ctrl Pts',(0.273113628774048,0.650312103452947,
-1.10183818743633));
#50304=CARTESIAN_POINT('Ctrl Pts',(-0.0708182368002938,0.701770378012652,
-1.08598067686038));
#50305=CARTESIAN_POINT('Ctrl Pts',(-0.397534816887265,0.582634495616192,
-1.07012316628444));
#50306=CARTESIAN_POINT('Ctrl Pts',(-0.623871437853526,0.326107342335911,
-1.05452361453731));
#50307=CARTESIAN_POINT('Ctrl Pts',(-0.676706455860252,0.106856038111985,
-1.04420989964883));
#50308=CARTESIAN_POINT('Ctrl Pts',(-0.676753912310732,-5.67166874834366E-6,
-1.039182021619));
#50309=CARTESIAN_POINT('Origin',(0.,0.,-6.17861797838101));
#50310=CARTESIAN_POINT('',(-0.676749171927519,8.41897198169495E-6,-1.478617978381));
#50311=CARTESIAN_POINT('',(-0.676685230808469,-1.71094250207282E-5,-1.439182021619));
#50312=CARTESIAN_POINT('',(-0.6767,7.27977111083166E-14,-6.17861797838101));
#50313=CARTESIAN_POINT('Ctrl Pts',(-0.676749171927519,8.41897198166925E-6,
-1.478617978381));
#50314=CARTESIAN_POINT('Ctrl Pts',(-0.676684377322802,-0.103966600961598,
-1.47372601965117));
#50315=CARTESIAN_POINT('Ctrl Pts',(-0.626054318658875,-0.320349160458701,
-1.46354822406269));
#50316=CARTESIAN_POINT('Ctrl Pts',(-0.404965598083139,-0.577494374128802,
-1.44808459161556));
#50317=CARTESIAN_POINT('Ctrl Pts',(-0.0798019238330923,-0.700805636916392,
-1.43222708103962));
#50318=CARTESIAN_POINT('Ctrl Pts',(0.264760890572085,-0.65375726275486,
-1.41636957046367));
#50319=CARTESIAN_POINT('Ctrl Pts',(0.544962679865294,-0.447786294269141,
-1.40051205988773));
#50320=CARTESIAN_POINT('Ctrl Pts',(0.692688873355398,-0.13296244774702,
-1.38465454931178));
#50321=CARTESIAN_POINT('Ctrl Pts',(0.672028543154347,0.21418339096928,-1.36879703873584));
#50322=CARTESIAN_POINT('Ctrl Pts',(0.488004032358267,0.509263146303875,
-1.3529395281599));
#50323=CARTESIAN_POINT('Ctrl Pts',(0.185350067969226,0.680545545929922,
-1.33708201758396));
#50324=CARTESIAN_POINT('Ctrl Pts',(-0.162360854618199,0.686393357098464,
-1.32122450700801));
#50325=CARTESIAN_POINT('Ctrl Pts',(-0.470603292949117,0.525385028761478,
-1.30536699643207));
#50326=CARTESIAN_POINT('Ctrl Pts',(-0.644211358515505,0.266799669463018,
-1.29116482022306));
#50327=CARTESIAN_POINT('Ctrl Pts',(-0.676606056624289,0.0771731047055059,
-1.28224848087271));
#50328=CARTESIAN_POINT('Ctrl Pts',(-0.676672623201375,-1.57520597928451E-5,
-1.278617978381));
#50329=CARTESIAN_POINT('Ctrl Pts',(-0.676685230808469,-1.71094250207143E-5,
-1.439182021619));
#50330=CARTESIAN_POINT('Ctrl Pts',(-0.676714877572692,-0.0307457878633605,
-1.43773665092304));
#50331=CARTESIAN_POINT('Ctrl Pts',(-0.667145429154239,-0.173833392972892,
-1.43100544336844));
#50332=CARTESIAN_POINT('Ctrl Pts',(-0.568095276096871,-0.418048613675424,
-1.41898839895519));
#50333=CARTESIAN_POINT('Ctrl Pts',(-0.299291263068257,-0.638687424309053,
-1.40313088837925));
#50334=CARTESIAN_POINT('Ctrl Pts',(0.0422678024777705,-0.704066984734566,
-1.3872733778033));
#50335=CARTESIAN_POINT('Ctrl Pts',(0.373551939990352,-0.598294103471671,
-1.37141586722736));
#50336=CARTESIAN_POINT('Ctrl Pts',(0.614028912825419,-0.347081230166595,
-1.35555835665142));
#50337=CARTESIAN_POINT('Ctrl Pts',(0.705240900970187,-0.0114959870512474,
-1.33970084607548));
#50338=CARTESIAN_POINT('Ctrl Pts',(0.625015078797678,0.326883828592142,
-1.32384333549953));
#50339=CARTESIAN_POINT('Ctrl Pts',(0.392853632391026,0.585801083676619,
-1.30798582492359));
#50340=CARTESIAN_POINT('Ctrl Pts',(0.0651929510142312,0.702315289067225,
-1.29212831434764));
#50341=CARTESIAN_POINT('Ctrl Pts',(-0.27831555874946,0.648102874455513,
-1.2762708037717));
#50342=CARTESIAN_POINT('Ctrl Pts',(-0.554168023743774,0.43634239718304,
-1.26041329319576));
#50343=CARTESIAN_POINT('Ctrl Pts',(-0.664203759053046,0.188552741867401,
-1.24805036581152));
#50344=CARTESIAN_POINT('Ctrl Pts',(-0.676694840205421,0.0380997719910252,
-1.24097327528594));
#50345=CARTESIAN_POINT('Ctrl Pts',(-0.676665319626825,1.43824383197974E-5,
-1.239182021619));
#50346=CARTESIAN_POINT('Origin',(0.,0.,-6.17861797838101));
#50347=CARTESIAN_POINT('',(-0.676643729523802,3.91070869351799E-6,-1.678617978381));
#50348=CARTESIAN_POINT('',(-0.676739142367725,1.21009199712183E-5,-1.639182021619));
#50349=CARTESIAN_POINT('',(-0.6767,7.27977111083166E-14,-6.17861797838101));
#50350=CARTESIAN_POINT('Ctrl Pts',(-0.676643729523802,3.91070869351987E-6,
-1.678617978381));
#50351=CARTESIAN_POINT('Ctrl Pts',(-0.676631511654014,-0.060443692974697,
-1.67577523214692));
#50352=CARTESIAN_POINT('Ctrl Pts',(-0.653687683271354,-0.233297400810955,
-1.6676466490542));
#50353=CARTESIAN_POINT('Ctrl Pts',(-0.508277862304651,-0.489030165196652,
-1.65423222910282));
#50354=CARTESIAN_POINT('Ctrl Pts',(-0.212827550790863,-0.672459159656269,
-1.63837471852688));
#50355=CARTESIAN_POINT('Ctrl Pts',(0.134359251378219,-0.692419294467113,
-1.62251720795094));
#50356=CARTESIAN_POINT('Ctrl Pts',(0.448884510774523,-0.54405843782444,
-1.60665969737499));
#50357=CARTESIAN_POINT('Ctrl Pts',(0.65428992543882,-0.263441798601729,
-1.59080218679905));
#50358=CARTESIAN_POINT('Ctrl Pts',(0.700643260203079,0.0812152061701052,
-1.57494467622311));
#50359=CARTESIAN_POINT('Ctrl Pts',(0.576676430357581,0.406129514380929,
-1.55908716564716));
#50360=CARTESIAN_POINT('Ctrl Pts',(0.312524673140342,0.63231733841464,-1.54322965507122));
#50361=CARTESIAN_POINT('Ctrl Pts',(-0.0275990612546199,0.704794423643601,
-1.52737214449527));
#50362=CARTESIAN_POINT('Ctrl Pts',(-0.361013708553533,0.605942233234882,
-1.51151463391933));
#50363=CARTESIAN_POINT('Ctrl Pts',(-0.606669124072505,0.359790858247332,
-1.49565712334339));
#50364=CARTESIAN_POINT('Ctrl Pts',(-0.674560784855072,0.129095479649908,
-1.48469157149728));
#50365=CARTESIAN_POINT('Ctrl Pts',(-0.676754388892557,0.00838001173401543,
-1.47901185650982));
#50366=CARTESIAN_POINT('Ctrl Pts',(-0.676749171927519,8.41897198166925E-6,
-1.478617978381));
#50367=CARTESIAN_POINT('Ctrl Pts',(-0.676739142367725,1.210091997122E-5,
-1.63918202161899));
#50368=CARTESIAN_POINT('Ctrl Pts',(-0.676656450938597,-0.0995045696225097,
-1.63450002656015));
#50369=CARTESIAN_POINT('Ctrl Pts',(-0.629338348642414,-0.311448711915821,
-1.62453219464265));
#50370=CARTESIAN_POINT('Ctrl Pts',(-0.416313374927947,-0.569368123427741,
-1.60927852586652));
#50371=CARTESIAN_POINT('Ctrl Pts',(-0.0936533636192634,-0.699089360241109,
-1.59342101529057));
#50372=CARTESIAN_POINT('Ctrl Pts',(0.251772950048864,-0.658868171748504,
-1.57756350471463));
#50373=CARTESIAN_POINT('Ctrl Pts',(0.535995491794349,-0.458481972268986,
-1.56170599413868));
#50374=CARTESIAN_POINT('Ctrl Pts',(0.689922281653143,-0.146642870259839,
-1.54584848356274));
#50375=CARTESIAN_POINT('Ctrl Pts',(0.676135081734832,0.200843813364896,
-1.5299909729868));
#50376=CARTESIAN_POINT('Ctrl Pts',(0.49798543810141,0.49950714665405,-1.51413346241085));
#50377=CARTESIAN_POINT('Ctrl Pts',(0.198779949634609,0.676744721252252,
-1.49827595183491));
#50378=CARTESIAN_POINT('Ctrl Pts',(-0.148747182193283,0.689471654173747,
-1.48241844125896));
#50379=CARTESIAN_POINT('Ctrl Pts',(-0.460115192831522,0.534594140863082,
-1.46656093068302));
#50380=CARTESIAN_POINT('Ctrl Pts',(-0.641447726706004,0.275723280480322,
-1.45214879080303));
#50381=CARTESIAN_POINT('Ctrl Pts',(-0.676606456972008,0.0816314601060807,
-1.44302248778169));
#50382=CARTESIAN_POINT('Ctrl Pts',(-0.676685230808469,-1.71094250207143E-5,
-1.439182021619));
#50383=CARTESIAN_POINT('Origin',(0.,0.,-6.17861797838101));
#50384=CARTESIAN_POINT('',(-0.676728058604507,-1.46844370246448E-5,-1.878617978381));
#50385=CARTESIAN_POINT('',(-0.676642402811546,-1.99994779626067E-7,-1.839182021619));
#50386=CARTESIAN_POINT('',(-0.6767,7.27977111083166E-14,-6.17861797838101));
#50387=CARTESIAN_POINT('Ctrl Pts',(-0.676728058604507,-1.46844370245737E-5,
-1.878617978381));
#50388=CARTESIAN_POINT('Ctrl Pts',(-0.676744117284434,-0.0168821899574054,
-1.87782444464268));
#50389=CARTESIAN_POINT('Ctrl Pts',(-0.672010154326253,-0.14609746486122,
-1.87174507404571));
#50390=CARTESIAN_POINT('Ctrl Pts',(-0.592689897555636,-0.382381449755007,
-1.86037986659008));
#50391=CARTESIAN_POINT('Ctrl Pts',(-0.337939220168536,-0.619107398803415,
-1.84452235601415));
#50392=CARTESIAN_POINT('Ctrl Pts',(-0.00103851454807973,-0.705333828246443,
-1.8286648454382));
#50393=CARTESIAN_POINT('Ctrl Pts',(0.336114644751484,-0.620099857575242,
-1.81280733486226));
#50394=CARTESIAN_POINT('Ctrl Pts',(0.591561313924781,-0.384125109370422,
-1.79694982428632));
#50395=CARTESIAN_POINT('Ctrl Pts',(0.70320467250143,-0.0547729527541542,
-1.78109231371037));
#50396=CARTESIAN_POINT('Ctrl Pts',(0.64390520984823,0.287894023056329,-1.76523480313443));
#50397=CARTESIAN_POINT('Ctrl Pts',(0.428078099583546,0.560576514347677,
-1.74937729255848));
#50398=CARTESIAN_POINT('Ctrl Pts',(0.10818899867648,0.69698782510646,-1.73351978198254));
#50399=CARTESIAN_POINT('Ctrl Pts',(-0.237999888598618,0.663967575118165,
-1.7176622714066));
#50400=CARTESIAN_POINT('Ctrl Pts',(-0.526333113076832,0.469542694395412,
-1.70180476083065));
#50401=CARTESIAN_POINT('Ctrl Pts',(-0.657967270519695,0.216292294824611,
-1.68878999648879));
#50402=CARTESIAN_POINT('Ctrl Pts',(-0.676654229709424,0.051953315149448,
-1.68106106900557));
#50403=CARTESIAN_POINT('Ctrl Pts',(-0.676643729523802,3.91070869351987E-6,
-1.678617978381));
#50404=CARTESIAN_POINT('Ctrl Pts',(-0.676642402811546,-1.99994779622598E-7,
-1.839182021619));
#50405=CARTESIAN_POINT('Ctrl Pts',(-0.676642980117375,-0.0559834906210994,
-1.8365492390559));
#50406=CARTESIAN_POINT('Ctrl Pts',(-0.655979709932234,-0.224364000430775,
-1.82863061963417));
#50407=CARTESIAN_POINT('Ctrl Pts',(-0.51785494220135,-0.478876962232637,
-1.81542616335378));
#50408=CARTESIAN_POINT('Ctrl Pts',(-0.226092044745908,-0.668116212512566,
-1.79956865277784));
#50409=CARTESIAN_POINT('Ctrl Pts',(0.120631824241489,-0.694942335089534,
-1.78371114220189));
#50410=CARTESIAN_POINT('Ctrl Pts',(0.438031166284854,-0.552834137407103,
-1.76785363162595));
#50411=CARTESIAN_POINT('Ctrl Pts',(0.648949015415239,-0.276336862381976,
-1.75199612105));
#50412=CARTESIAN_POINT('Ctrl Pts',(0.702113112519488,0.0673354538688382,
-1.73613861047406));
#50413=CARTESIAN_POINT('Ctrl Pts',(0.584599736947659,0.394639118284352,
-1.72028109989812));
#50414=CARTESIAN_POINT('Ctrl Pts',(0.324975348420559,0.626009511939285,
-1.70442358932217));
#50415=CARTESIAN_POINT('Ctrl Pts',(-0.0136476660564434,0.705202543480052,
-1.68856607874623));
#50416=CARTESIAN_POINT('Ctrl Pts',(-0.348953053916159,0.612967089069317,
-1.67270856817029));
#50417=CARTESIAN_POINT('Ctrl Pts',(-0.599431048207782,0.371724769909193,
-1.65685105759434));
#50418=CARTESIAN_POINT('Ctrl Pts',(-0.673261370829587,0.138027284702877,
-1.64567554207725));
#50419=CARTESIAN_POINT('Ctrl Pts',(-0.67674980716783,0.0128468700077985,
-1.6397858634188));
#50420=CARTESIAN_POINT('Ctrl Pts',(-0.676739142367725,1.210091997122E-5,
-1.63918202161899));
#50421=CARTESIAN_POINT('Origin',(0.,0.,-6.17861797838101));
#50422=CARTESIAN_POINT('',(-0.6766975754333,1.74675394711349E-5,-2.078617978381));
#50423=CARTESIAN_POINT('',(-0.676740228638047,-1.17804846946346E-5,-2.03918202161899));
#50424=CARTESIAN_POINT('',(-0.6767,7.27977111083166E-14,-6.17861797838101));
#50425=CARTESIAN_POINT('Ctrl Pts',(-0.6766975754333,1.74675394711173E-5,
-2.078617978381));
#50426=CARTESIAN_POINT('Ctrl Pts',(-0.676610386945761,-0.085659472551938,
-2.07458782027978));
#50427=CARTESIAN_POINT('Ctrl Pts',(-0.638863309880312,-0.28378240291994,
-2.06527182531992));
#50428=CARTESIAN_POINT('Ctrl Pts',(-0.450484675054114,-0.542734230837378,
-2.05066999350141));
#50429=CARTESIAN_POINT('Ctrl Pts',(-0.13639766348118,-0.692020639271782,
-2.03481248292547));
#50430=CARTESIAN_POINT('Ctrl Pts',(0.210846410774077,-0.67308296579615,
-2.01895497234952));
#50431=CARTESIAN_POINT('Ctrl Pts',(0.506835591947215,-0.490524790929845,
-2.00309746177358));
#50432=CARTESIAN_POINT('Ctrl Pts',(0.679617534353063,-0.188724388411024,
-1.98723995119763));
#50433=CARTESIAN_POINT('Ctrl Pts',(0.687190479687935,0.158953239688651,
-1.97138244062169));
#50434=CARTESIAN_POINT('Ctrl Pts',(0.527713512083115,0.467990744509071,
-1.95552493004575));
#50435=CARTESIAN_POINT('Ctrl Pts',(0.239954068430876,0.663263848573645,
-1.93966741946981));
#50436=CARTESIAN_POINT('Ctrl Pts',(-0.106136081809596,0.697303391587448,
-1.92380990889386));
#50437=CARTESIAN_POINT('Ctrl Pts',(-0.426425491571088,0.561834662440479,
-1.90795239831792));
#50438=CARTESIAN_POINT('Ctrl Pts',(-0.632214195584207,0.303402487836874,
-1.8928884214803));
#50439=CARTESIAN_POINT('Ctrl Pts',(-0.67663714821915,0.0954745733244865,
-1.88311028150133));
#50440=CARTESIAN_POINT('Ctrl Pts',(-0.676728058604507,-1.46844370245737E-5,
-1.878617978381));
#50441=CARTESIAN_POINT('Ctrl Pts',(-0.676740228638047,-1.17804846946623E-5,
-2.03918202161899));
#50442=CARTESIAN_POINT('Ctrl Pts',(-0.676750329773678,-0.012415612487542,
-2.03859845155166));
#50443=CARTESIAN_POINT('Ctrl Pts',(-0.67339073835084,-0.137164892122005,
-2.03272904462567));
#50444=CARTESIAN_POINT('Ctrl Pts',(-0.600140158358559,-0.370578839715501,
-2.02157380084104));
#50445=CARTESIAN_POINT('Ctrl Pts',(-0.350123530259618,-0.612299272968753,
-2.0057162902651));
#50446=CARTESIAN_POINT('Ctrl Pts',(-0.0149949761710098,-0.705175181645777,
-1.98985877968915));
#50447=CARTESIAN_POINT('Ctrl Pts',(0.323778723678411,-0.626629255790618,
-1.97400126911321));
#50448=CARTESIAN_POINT('Ctrl Pts',(0.583844686443398,-0.395755313585723,
-1.95814375853727));
#50449=CARTESIAN_POINT('Ctrl Pts',(0.701983182336375,-0.0686767634387369,
-1.94228624796132));
#50450=CARTESIAN_POINT('Ctrl Pts',(0.649475790428822,0.275096499007858,
-1.92642873738538));
#50451=CARTESIAN_POINT('Ctrl Pts',(0.439086592159748,0.551996241567879,
-1.91057122680944));
#50452=CARTESIAN_POINT('Ctrl Pts',(0.121959336304979,0.694710591834882,
-1.89471371623349));
#50453=CARTESIAN_POINT('Ctrl Pts',(-0.224815152906662,0.668546956573044,
-1.87885620565755));
#50454=CARTESIAN_POINT('Ctrl Pts',(-0.516939071671466,0.479865483546136,
-1.86299869508161));
#50455=CARTESIAN_POINT('Ctrl Pts',(-0.655762648669376,0.225226555268029,
-1.84977396706875));
#50456=CARTESIAN_POINT('Ctrl Pts',(-0.676641821060614,0.0564141472276884,
-1.84183507591455));
#50457=CARTESIAN_POINT('Ctrl Pts',(-0.676642402811546,-1.99994779622598E-7,
-1.839182021619));
#50458=CARTESIAN_POINT('Origin',(0.,0.,-6.17861797838101));
#50459=CARTESIAN_POINT('',(-0.676656556320913,-1.19096857998774E-5,-2.278617978381));
#50460=CARTESIAN_POINT('',(-0.676683955905987,1.70211467142023E-5,-2.23918202161899));
#50461=CARTESIAN_POINT('',(-0.6767,7.27977111083166E-14,-6.17861797838101));
#50462=CARTESIAN_POINT('Ctrl Pts',(-0.676656556320913,-1.19096857998831E-5,
-2.278617978381));
#50463=CARTESIAN_POINT('Ctrl Pts',(-0.676683115505212,-0.0421320665452035,
-2.27663703277554));
#50464=CARTESIAN_POINT('Ctrl Pts',(-0.662482884559255,-0.196625443856858,
-2.26937025031143));
#50465=CARTESIAN_POINT('Ctrl Pts',(-0.546278931161056,-0.446179579486538,
-2.25681763098868));
#50466=CARTESIAN_POINT('Ctrl Pts',(-0.266684887662029,-0.652974776292271,
-2.24096012041273));
#50467=CARTESIAN_POINT('Ctrl Pts',(0.0777378875832581,-0.701037594295302,
-2.22510260983679));
#50468=CARTESIAN_POINT('Ctrl Pts',(0.403263271585882,-0.578684388566949,
-2.20924509926084));
#50469=CARTESIAN_POINT('Ctrl Pts',(0.630758929622586,-0.315658138628835,
-2.1933875886849));
#50470=CARTESIAN_POINT('Ctrl Pts',(0.704922684214943,0.0241018061657587,
-2.17753007810895));
#50471=CARTESIAN_POINT('Ctrl Pts',(0.607725984161892,0.358002815569531,
-2.16167256753301));
#50472=CARTESIAN_POINT('Ctrl Pts',(0.362796485494498,0.604876514583012,
-2.14581505695707));
#50473=CARTESIAN_POINT('Ctrl Pts',(0.0296743777790237,0.704710095773204,
-2.12995754638113));
#50474=CARTESIAN_POINT('Ctrl Pts',(-0.310661308079694,0.633234900683358,
-2.11410003580518));
#50475=CARTESIAN_POINT('Ctrl Pts',(-0.575477984286229,0.407825915536408,
-2.09824252522924));
#50476=CARTESIAN_POINT('Ctrl Pts',(-0.668652086086511,0.165761324663879,
-2.08641517275451));
#50477=CARTESIAN_POINT('Ctrl Pts',(-0.676724740802238,0.026711882739232,
-2.07987365713843));
#50478=CARTESIAN_POINT('Ctrl Pts',(-0.6766975754333,1.74675394711173E-5,
-2.078617978381));
#50479=CARTESIAN_POINT('Ctrl Pts',(-0.676683955905987,1.70211467142092E-5,
-2.23918202161899));
#50480=CARTESIAN_POINT('Ctrl Pts',(-0.676606246433108,-0.0812010095403874,
-2.23536182718876));
#50481=CARTESIAN_POINT('Ctrl Pts',(-0.641718981747392,-0.274861857426088,
-2.22625579589989));
#50482=CARTESIAN_POINT('Ctrl Pts',(-0.461135729708285,-0.533714085354632,
-2.21186392775236));
#50483=CARTESIAN_POINT('Ctrl Pts',(-0.150064190853226,-0.689186204695865,
-2.19600641717642));
#50484=CARTESIAN_POINT('Ctrl Pts',(0.197486622320041,-0.677123268042198,
-2.18014890660047));
#50485=CARTESIAN_POINT('Ctrl Pts',(0.497030188535669,-0.500457668343409,
-2.16429139602453));
#50486=CARTESIAN_POINT('Ctrl Pts',(0.675750122618055,-0.20213524655836,
-2.14843388544859));
#50487=CARTESIAN_POINT('Ctrl Pts',(0.690201193133537,0.145324461521679,
-2.13257637487265));
#50488=CARTESIAN_POINT('Ctrl Pts',(0.536870472963871,0.457457081461282,
-2.1167188642967));
#50489=CARTESIAN_POINT('Ctrl Pts',(0.253031300742842,0.65838594073986,-2.10086135372076));
#50490=CARTESIAN_POINT('Ctrl Pts',(-0.0923175372979227,0.699267015114235,
-2.08500384314482));
#50491=CARTESIAN_POINT('Ctrl Pts',(-0.415224800514443,0.57016247785808,
-2.06914633256887));
#50492=CARTESIAN_POINT('Ctrl Pts',(-0.629025916191861,0.3123083083271,-2.05387239206027));
#50493=CARTESIAN_POINT('Ctrl Pts',(-0.676658836124467,0.0999353048383027,
-2.0438842884103));
#50494=CARTESIAN_POINT('Ctrl Pts',(-0.676740228638047,-1.17804846946623E-5,
-2.03918202161899));
#50495=CARTESIAN_POINT('Origin',(0.,0.,-6.17861797838101));
#50496=CARTESIAN_POINT('',(-0.676757533991425,1.53215262135908E-6,-2.478617978381));
#50497=CARTESIAN_POINT('',(-0.676666358633788,-1.46093892624266E-5,-2.43918202161899));
#50498=CARTESIAN_POINT('',(-0.6767,7.27977111083166E-14,-6.17861797838101));
#50499=CARTESIAN_POINT('Ctrl Pts',(-0.676757533991425,1.53215262137176E-6,
-2.478617978381));
#50500=CARTESIAN_POINT('Ctrl Pts',(-0.676742969913277,-0.110890132171142,
-2.47340040841265));
#50501=CARTESIAN_POINT('Ctrl Pts',(-0.620749487720945,-0.334138543334539,
-2.46289700158564));
#50502=CARTESIAN_POINT('Ctrl Pts',(-0.387055478021894,-0.589648153320687,
-2.4471077579));
#50503=CARTESIAN_POINT('Ctrl Pts',(-0.0582613062111292,-0.70292425479551,
-2.43125024732405));
#50504=CARTESIAN_POINT('Ctrl Pts',(0.284695672591286,-0.645325702098597,
-2.41539273674811));
#50505=CARTESIAN_POINT('Ctrl Pts',(0.558445657515852,-0.430854192718303,
-2.39953522617216));
#50506=CARTESIAN_POINT('Ctrl Pts',(0.696442454311359,-0.111645849067578,
-2.38367771559622));
#50507=CARTESIAN_POINT('Ctrl Pts',(0.665140265164793,0.234702610632607,
-2.36782020502028));
#50508=CARTESIAN_POINT('Ctrl Pts',(0.472148374730573,0.523996946575577,
-2.35196269444434));
#50509=CARTESIAN_POINT('Ctrl Pts',(0.164381400495464,0.685912270594717,
-2.33610518386839));
#50510=CARTESIAN_POINT('Ctrl Pts',(-0.183345234784635,0.681088402972051,
-2.32024767329245));
#50511=CARTESIAN_POINT('Ctrl Pts',(-0.486502269038555,0.510697983157941,
-2.3043901627165));
#50512=CARTESIAN_POINT('Ctrl Pts',(-0.648297829736711,0.252955391533677,
-2.29051359774602));
#50513=CARTESIAN_POINT('Ctrl Pts',(-0.676612246565188,0.0702588426274883,
-2.28192286963419));
#50514=CARTESIAN_POINT('Ctrl Pts',(-0.676656556320913,-1.19096857998831E-5,
-2.278617978381));
#50515=CARTESIAN_POINT('Ctrl Pts',(-0.676666358633788,-1.4609389262385E-5,
-2.43918202161899));
#50516=CARTESIAN_POINT('Ctrl Pts',(-0.676696070333537,-0.0376688183928807,
-2.43741103968452));
#50517=CARTESIAN_POINT('Ctrl Pts',(-0.664383137857744,-0.187690043031484,
-2.43035422089139));
#50518=CARTESIAN_POINT('Ctrl Pts',(-0.555000672657401,-0.435282826986497,
-2.41801156523963));
#50519=CARTESIAN_POINT('Ctrl Pts',(-0.27955329320369,-0.647569951726063,
-2.40215405466368));
#50520=CARTESIAN_POINT('Ctrl Pts',(0.0638510132913964,-0.702438562595467,
-2.38629654408774));
#50521=CARTESIAN_POINT('Ctrl Pts',(0.391733704562298,-0.586550586760786,
-2.3704390335118));
#50522=CARTESIAN_POINT('Ctrl Pts',(0.624389405388874,-0.328077363677613,
-2.35458152293585));
#50523=CARTESIAN_POINT('Ctrl Pts',(0.70526157763973,0.0101485577617963,
-2.33872401235991));
#50524=CARTESIAN_POINT('Ctrl Pts',(0.614690913258262,0.345907454787038,
-2.32286650178397));
#50525=CARTESIAN_POINT('Ctrl Pts',(0.374694337750614,0.59757931639001,-2.30700899120802));
#50526=CARTESIAN_POINT('Ctrl Pts',(0.0436128907985044,0.703984944353017,
-2.29115148063208));
#50527=CARTESIAN_POINT('Ctrl Pts',(-0.298070463232192,0.639258073916999,
-2.27529397005614));
#50528=CARTESIAN_POINT('Ctrl Pts',(-0.567295530361938,0.419133233412588,
-2.25943645948019));
#50529=CARTESIAN_POINT('Ctrl Pts',(-0.666979967577887,0.174696049819589,
-2.24739914333448));
#50530=CARTESIAN_POINT('Ctrl Pts',(-0.67671376965045,0.0311768466220108,
-2.24064766404741));
#50531=CARTESIAN_POINT('Ctrl Pts',(-0.676683955905987,1.70211467142092E-5,
-2.23918202161899));
#50532=CARTESIAN_POINT('Origin',(0.,0.,-6.17861797838101));
#50533=CARTESIAN_POINT('',(-0.676651429080103,9.78749391371E-6,-2.678617978381));
#50534=CARTESIAN_POINT('',(-0.676753308202105,6.0958899819781E-6,-2.63918202161899));
#50535=CARTESIAN_POINT('',(-0.6767,7.27977111083166E-14,-6.17861797838101));
#50536=CARTESIAN_POINT('Ctrl Pts',(-0.676651429080103,9.78749391371964E-6,
-2.678617978381));
#50537=CARTESIAN_POINT('Ctrl Pts',(-0.676616861736543,-0.0673593563639852,
-2.6754496209084));
#50538=CARTESIAN_POINT('Ctrl Pts',(-0.649939928618552,-0.247148624797767,
-2.66699542657715));
#50539=CARTESIAN_POINT('Ctrl Pts',(-0.493033473894675,-0.504395560448939,
-2.65325539538726));
#50540=CARTESIAN_POINT('Ctrl Pts',(-0.19209406288682,-0.678672792135419,
-2.63739788481132));
#50541=CARTESIAN_POINT('Ctrl Pts',(0.155541711691216,-0.687970685207893,
-2.62154037423537));
#50542=CARTESIAN_POINT('Ctrl Pts',(0.465366675199364,-0.530029004296125,
-2.60568286365943));
#50543=CARTESIAN_POINT('Ctrl Pts',(0.662065125935696,-0.243241971709246,
-2.58982535308348));
#50544=CARTESIAN_POINT('Ctrl Pts',(0.697821414466598,0.102675027602084,
-2.57396784250754));
#50545=CARTESIAN_POINT('Ctrl Pts',(0.563943504067627,0.423632638026367,
-2.5581103319316));
#50546=CARTESIAN_POINT('Ctrl Pts',(0.292975927787107,0.641608910099083,
-2.54225282135566));
#50547=CARTESIAN_POINT('Ctrl Pts',(-0.0492114989961208,0.703615744670204,
-2.52639531077971));
#50548=CARTESIAN_POINT('Ctrl Pts',(-0.379436046685527,0.594579830011842,
-2.51053780020377));
#50549=CARTESIAN_POINT('Ctrl Pts',(-0.617423055528672,0.341006830258411,
-2.49468028962782));
#50550=CARTESIAN_POINT('Ctrl Pts',(-0.676399412320139,0.115245834625529,
-2.48404034902024));
#50551=CARTESIAN_POINT('Ctrl Pts',(-0.676757724548395,0.0014524430419314,
-2.47868624527129));
#50552=CARTESIAN_POINT('Ctrl Pts',(-0.676757533991425,1.53215262137176E-6,
-2.478617978381));
#50553=CARTESIAN_POINT('Ctrl Pts',(-0.676753308202105,6.0958899819755E-6,
-2.63918202161899));
#50554=CARTESIAN_POINT('Ctrl Pts',(-0.676702953103352,-0.106425038065699,
-2.63417441532163));
#50555=CARTESIAN_POINT('Ctrl Pts',(-0.624199859688166,-0.325248720721236,
-2.62388097216561));
#50556=CARTESIAN_POINT('Ctrl Pts',(-0.398647252183052,-0.581873916279484,
-2.60830169215095));
#50557=CARTESIAN_POINT('Ctrl Pts',(-0.072158885197231,-0.701633794373258,
-2.59244418157501));
#50558=CARTESIAN_POINT('Ctrl Pts',(0.271870667014987,-0.650832717782648,
-2.57658667099906));
#50559=CARTESIAN_POINT('Ctrl Pts',(0.549810870497681,-0.441819977821406,
-2.56072916042312));
#50560=CARTESIAN_POINT('Ctrl Pts',(0.694096926018893,-0.125404718454481,
-2.54487164984717));
#50561=CARTESIAN_POINT('Ctrl Pts',(0.669654172730331,0.221495316122894,
-2.52901413927123));
#50562=CARTESIAN_POINT('Ctrl Pts',(0.48242442724551,0.514551803141691,-2.51315662869529));
#50563=CARTESIAN_POINT('Ctrl Pts',(0.17792158070152,0.682525308864219,-2.49729911811934));
#50564=CARTESIAN_POINT('Ctrl Pts',(-0.169832424647492,0.684582963312612,
-2.4814416075434));
#50565=CARTESIAN_POINT('Ctrl Pts',(-0.476301673309269,0.520224568933759,
-2.46558409696745));
#50566=CARTESIAN_POINT('Ctrl Pts',(-0.645690377045496,0.261883291547497,
-2.45149756832599));
#50567=CARTESIAN_POINT('Ctrl Pts',(-0.676607390040075,0.0747174244931122,
-2.44269687654317));
#50568=CARTESIAN_POINT('Ctrl Pts',(-0.676666358633788,-1.4609389262385E-5,
-2.43918202161899));
#50569=CARTESIAN_POINT('Origin',(0.,0.,-6.17861797838101));
#50570=CARTESIAN_POINT('',(-0.676706726596661,-1.7186887101997E-5,-2.878617978381));
#50571=CARTESIAN_POINT('',(-0.676645697232346,6.098308949265E-6,-2.83918202161899));
#50572=CARTESIAN_POINT('',(-0.6767,7.27977111083166E-14,-6.17861797838101));
#50573=CARTESIAN_POINT('Ctrl Pts',(-0.676706726596661,-1.71868871020019E-5,
-2.878617978381));
#50574=CARTESIAN_POINT('Ctrl Pts',(-0.67673120694042,-0.0238081107658035,
-2.87749883340416));
#50575=CARTESIAN_POINT('Ctrl Pts',(-0.669690139537909,-0.159951598195322,
-2.87109385156866));
#50576=CARTESIAN_POINT('Ctrl Pts',(-0.580678100880426,-0.400387101364609,
-2.85940303287452));
#50577=CARTESIAN_POINT('Ctrl Pts',(-0.318783833330571,-0.629184992977676,
-2.84354552229858));
#50578=CARTESIAN_POINT('Ctrl Pts',(0.0206039577451542,-0.705033591190155,
-2.82768801172263));
#50579=CARTESIAN_POINT('Ctrl Pts',(0.35498310936897,-0.609494774254864,
-2.81183050114669));
#50580=CARTESIAN_POINT('Ctrl Pts',(0.603069014406956,-0.365793181515832,
-2.79597299057075));
#50581=CARTESIAN_POINT('Ctrl Pts',(0.704554188889049,-0.0331705094948168,
-2.78011547999481));
#50582=CARTESIAN_POINT('Ctrl Pts',(0.634768486672358,0.307515619292639,
-2.76425796941886));
#50583=CARTESIAN_POINT('Ctrl Pts',(0.410676193241495,0.573447427482177,
-2.74840045884292));
#50584=CARTESIAN_POINT('Ctrl Pts',(0.0867521583136464,0.699979250270445,
-2.73254294826698));
#50585=CARTESIAN_POINT('Ctrl Pts',(-0.258260557150356,0.656352323376431,
-2.71668543769103));
#50586=CARTESIAN_POINT('Ctrl Pts',(-0.54049242092486,0.453171965929088,
-2.70082792711509));
#50587=CARTESIAN_POINT('Ctrl Pts',(-0.661196692645007,0.202435872569431,
-2.68813877401175));
#50588=CARTESIAN_POINT('Ctrl Pts',(-0.676674531156826,0.045033991551841,
-2.68073545776705));
#50589=CARTESIAN_POINT('Ctrl Pts',(-0.676651429080103,9.78749391371964E-6,
-2.678617978381));
#50590=CARTESIAN_POINT('Ctrl Pts',(-0.676645697232345,6.09830894927194E-6,
-2.83918202161899));
#50591=CARTESIAN_POINT('Ctrl Pts',(-0.676625799079458,-0.0629000889752367,
-2.83622362781738));
#50592=CARTESIAN_POINT('Ctrl Pts',(-0.652383626261716,-0.238217374673108,
-2.82797939715712));
#50593=CARTESIAN_POINT('Ctrl Pts',(-0.502917578453797,-0.494540994662418,
-2.81444932963821));
#50594=CARTESIAN_POINT('Ctrl Pts',(-0.205485567371259,-0.674738888549961,
-2.79859181906227));
#50595=CARTESIAN_POINT('Ctrl Pts',(0.141898163291737,-0.690913740906892,
-2.78273430848633));
#50596=CARTESIAN_POINT('Ctrl Pts',(0.454787708536229,-0.539133588532463,
-2.76687679791038));
#50597=CARTESIAN_POINT('Ctrl Pts',(0.657122394010951,-0.256294840776867,
-2.75101928733444));
#50598=CARTESIAN_POINT('Ctrl Pts',(0.69971645158859,0.0888469104459926,
-2.7351617767585));
#50599=CARTESIAN_POINT('Ctrl Pts',(0.572215643513511,0.412390765461524,
-2.71930426618255));
#50600=CARTESIAN_POINT('Ctrl Pts',(0.305614285798879,0.635686081674883,
-2.70344675560661));
#50601=CARTESIAN_POINT('Ctrl Pts',(-0.0352791951986797,0.704451747464407,
-2.68758924503067));
#50602=CARTESIAN_POINT('Ctrl Pts',(-0.367596616630921,0.601971439157228,
-2.67173173445472));
#50603=CARTESIAN_POINT('Ctrl Pts',(-0.610554559694072,0.353157211106192,
-2.65587422387878));
#50604=CARTESIAN_POINT('Ctrl Pts',(-0.675238312251887,0.124176238940119,
-2.6450243196002));
#50605=CARTESIAN_POINT('Ctrl Pts',(-0.676756106011389,0.00591957877575619,
-2.63946025218027));
#50606=CARTESIAN_POINT('Ctrl Pts',(-0.676753308202105,6.0958899819755E-6,
-2.63918202161899));
#50607=CARTESIAN_POINT('Origin',(0.,0.,-6.17861797838101));
#50608=CARTESIAN_POINT('',(-0.676719327190981,1.60436807500843E-5,-3.078617978381));
#50609=CARTESIAN_POINT('',(-0.676720689883097,-1.58642249737939E-5,-3.03918202161899));
#50610=CARTESIAN_POINT('',(-0.6767,7.27977111083166E-14,-6.17861797838101));
#50611=CARTESIAN_POINT('Ctrl Pts',(-0.676719327190981,1.60436807501024E-5,
-3.078617978381));
#50612=CARTESIAN_POINT('Ctrl Pts',(-0.676626430457751,-0.0925744753283335,
-3.07426220904126));
#50613=CARTESIAN_POINT('Ctrl Pts',(-0.634231039946861,-0.297608388428762,
-3.06462060284287));
#50614=CARTESIAN_POINT('Ctrl Pts',(-0.433619679201001,-0.556301053019741,
-3.04969315978585));
#50615=CARTESIAN_POINT('Ctrl Pts',(-0.115099950991358,-0.695879938684137,
-3.0338356492099));
#50616=CARTESIAN_POINT('Ctrl Pts',(0.231399554821144,-0.666296580968136,
-3.01797813863396));
#50617=CARTESIAN_POINT('Ctrl Pts',(0.521647880459103,-0.474742431844655,
-3.00212062805801));
#50618=CARTESIAN_POINT('Ctrl Pts',(0.685088231319183,-0.167782606634913,
-2.98626311748207));
#50619=CARTESIAN_POINT('Ctrl Pts',(0.681989707179352,0.179963682677014,
-2.97040560690613));
#50620=CARTESIAN_POINT('Ctrl Pts',(0.513105531786303,0.48396239629908,-2.95454809633019));
#50621=CARTESIAN_POINT('Ctrl Pts',(0.219489950840751,0.670314142220776,
-2.93869058575424));
#50622=CARTESIAN_POINT('Ctrl Pts',(-0.127481691142976,0.693718463214421,
-2.92283307517829));
#50623=CARTESIAN_POINT('Ctrl Pts',(-0.443463664270248,0.548485976350586,
-2.90697556460236));
#50624=CARTESIAN_POINT('Ctrl Pts',(-0.636951241452163,0.289581126223947,
-2.89223719900325));
#50625=CARTESIAN_POINT('Ctrl Pts',(-0.676615583758409,0.0885588702252283,
-2.8827846702628));
#50626=CARTESIAN_POINT('Ctrl Pts',(-0.676706726596661,-1.71868871020019E-5,
-2.878617978381));
#50627=CARTESIAN_POINT('Ctrl Pts',(-0.676720689883097,-1.58642249737904E-5,
-3.03918202161899));
#50628=CARTESIAN_POINT('Ctrl Pts',(-0.676739964302642,-0.0193422042320756,
-3.03827284031314));
#50629=CARTESIAN_POINT('Ctrl Pts',(-0.671211161756148,-0.151017847550784,
-3.03207782214863));
#50630=CARTESIAN_POINT('Ctrl Pts',(-0.588486997030099,-0.388818647245757,
-3.02059696712548));
#50631=CARTESIAN_POINT('Ctrl Pts',(-0.331171302414811,-0.62275392778882,
-3.00473945654953));
#50632=CARTESIAN_POINT('Ctrl Pts',(0.00664919963267667,-0.70530324986049,
-2.98888194597359));
#50633=CARTESIAN_POINT('Ctrl Pts',(0.342853340201669,-0.61639960515244,
-2.97302443539765));
#50634=CARTESIAN_POINT('Ctrl Pts',(0.595712873526129,-0.377654681468092,
-2.9571669248217));
#50635=CARTESIAN_POINT('Ctrl Pts',(0.703759888922834,-0.0471052530281482,
-2.94130941424576));
#50636=CARTESIAN_POINT('Ctrl Pts',(0.640729114900228,0.29489504478491,-2.92545190366982));
#50637=CARTESIAN_POINT('Ctrl Pts',(0.421942773788548,0.565208971768099,
-2.90959439309387));
#50638=CARTESIAN_POINT('Ctrl Pts',(0.100585885339081,0.698125608891462,
-2.89373688251793));
#50639=CARTESIAN_POINT('Ctrl Pts',(-0.245222540035754,0.661334100117283,
-2.87787937194199));
#50640=CARTESIAN_POINT('Ctrl Pts',(-0.531419540085806,0.463778135032813,
-2.86202186136604));
#50641=CARTESIAN_POINT('Ctrl Pts',(-0.659140535672339,0.211371023644656,
-2.84912274459171));
#50642=CARTESIAN_POINT('Ctrl Pts',(-0.67666135161134,0.0494959832456144,
-2.84150946467603));
#50643=CARTESIAN_POINT('Ctrl Pts',(-0.676645697232345,6.09830894927194E-6,
-2.83918202161899));
#50644=CARTESIAN_POINT('Origin',(0.,0.,-6.17861797838101));
#50645=CARTESIAN_POINT('',(-0.676646145701304,-6.48367876880208E-6,-3.278617978381));
#50646=CARTESIAN_POINT('',(-0.676705321009977,1.72594551696437E-5,-3.239182021619));
#50647=CARTESIAN_POINT('',(-0.6767,7.27977111083166E-14,-6.17861797838101));
#50648=CARTESIAN_POINT('Ctrl Pts',(-0.676646145701304,-6.48367876878927E-6,
-3.278617978381));
#50649=CARTESIAN_POINT('Ctrl Pts',(-0.67666265341308,-0.0490521592361608,
-3.27631142153702));
#50650=CARTESIAN_POINT('Ctrl Pts',(-0.659349338354501,-0.210482214049339,
-3.26871902783439));
#50651=CARTESIAN_POINT('Ctrl Pts',(-0.532331448398351,-0.462731149618616,
-3.25584079727311));
#50652=CARTESIAN_POINT('Ctrl Pts',(-0.246523886922497,-0.660850104757407,
-3.23998328669717));
#50653=CARTESIAN_POINT('Ctrl Pts',(0.0992114457684886,-0.698322258566757,
-3.22412577612122));
#50654=CARTESIAN_POINT('Ctrl Pts',(0.420829355607847,-0.566038462686005,
-3.20826826554528));
#50655=CARTESIAN_POINT('Ctrl Pts',(0.640147380197513,-0.296155735057606,
-3.19241075496933));
#50656=CARTESIAN_POINT('Ctrl Pts',(0.703851252246643,0.0457198260286,-3.17655324439339));
#50657=CARTESIAN_POINT('Ctrl Pts',(0.596455125262476,0.376481302762003,
-3.16069573381745));
#50658=CARTESIAN_POINT('Ctrl Pts',(0.344066045534297,0.615723512700013,
-3.14483822324151));
#50659=CARTESIAN_POINT('Ctrl Pts',(0.00803756064714361,0.705288795742634,
-3.12898071266556));
#50660=CARTESIAN_POINT('Ctrl Pts',(-0.32994478397183,0.623404625673433,
-3.11312320208962));
#50661=CARTESIAN_POINT('Ctrl Pts',(-0.587720476917705,0.38997631824622,
-3.09726569151367));
#50662=CARTESIAN_POINT('Ctrl Pts',(-0.671063931972615,0.151906504437187,
-3.08576395027747));
#50663=CARTESIAN_POINT('Ctrl Pts',(-0.67673916300584,0.0197864740163767,
-3.07954804589991));
#50664=CARTESIAN_POINT('Ctrl Pts',(-0.676719327190981,1.60436807501024E-5,
-3.078617978381));
#50665=CARTESIAN_POINT('Ctrl Pts',(-0.676705321009976,1.72594551696367E-5,
-3.23918202161899));
#50666=CARTESIAN_POINT('Ctrl Pts',(-0.676614650526792,-0.0881153225781286,
-3.23503621595024));
#50667=CARTESIAN_POINT('Ctrl Pts',(-0.637246565667583,-0.28869418167919,
-3.22560457342284));
#50668=CARTESIAN_POINT('Ctrl Pts',(-0.44454248687824,-0.547611964332075,
-3.2108870940368));
#50669=CARTESIAN_POINT('Ctrl Pts',(-0.128847013424495,-0.693466173112368,
-3.19502958346085));
#50670=CARTESIAN_POINT('Ctrl Pts',(0.218170026627314,-0.670744903522167,
-3.17917207288491));
#50671=CARTESIAN_POINT('Ctrl Pts',(0.512151867514703,-0.484971494750699,
-3.16331456230897));
#50672=CARTESIAN_POINT('Ctrl Pts',(0.681634130178766,-0.181305815392006,
-3.14745705173302));
#50673=CARTESIAN_POINT('Ctrl Pts',(0.68541717920589,0.166433700220129,-3.13159954115708));
#50674=CARTESIAN_POINT('Ctrl Pts',(0.522581388918324,0.473714658920027,
-3.11574203058114));
#50675=CARTESIAN_POINT('Ctrl Pts',(0.232710696222986,0.665839784019352,
-3.0998845200052));
#50676=CARTESIAN_POINT('Ctrl Pts',(-0.113729903497026,0.696105160999459,
-3.08402700942925));
#50677=CARTESIAN_POINT('Ctrl Pts',(-0.432523772013128,0.557153545051146,
-3.0681694988533));
#50678=CARTESIAN_POINT('Ctrl Pts',(-0.633925378362749,0.298494876192099,
-3.05322116958322));
#50679=CARTESIAN_POINT('Ctrl Pts',(-0.676627905864348,0.0930180914472541,
-3.04355867717178));
#50680=CARTESIAN_POINT('Ctrl Pts',(-0.676720689883097,-1.58642249737904E-5,
-3.03918202161899));
#50681=CARTESIAN_POINT('Origin',(0.,0.,-6.17861797838101));
#50682=CARTESIAN_POINT('',(-0.676753931151198,-5.65874007816422E-6,-3.478617978381));
#50683=CARTESIAN_POINT('',(-0.676652143573121,-1.0128264255671E-5,-3.43918202161899));
#50684=CARTESIAN_POINT('',(-0.6767,7.27977111083166E-14,-6.17861797838101));
#50685=CARTESIAN_POINT('Ctrl Pts',(-0.676753931151198,-5.65874007810076E-6,
-3.478617978381));
#50686=CARTESIAN_POINT('Ctrl Pts',(-0.676756355253784,-0.00547521365838144,
-3.47836063403277));
#50687=CARTESIAN_POINT('Ctrl Pts',(-0.675357794150052,-0.12328784257846,
-3.4728174528259));
#50688=CARTESIAN_POINT('Ctrl Pts',(-0.611248559970205,-0.351954664290164,
-3.46198843476037));
#50689=CARTESIAN_POINT('Ctrl Pts',(-0.368780872539474,-0.601246668040893,
-3.44613092418443));
#50690=CARTESIAN_POINT('Ctrl Pts',(-0.0366658246279656,-0.704380937480284,
-3.43027341360848));
#50691=CARTESIAN_POINT('Ctrl Pts',(0.304362360169178,-0.636286446102303,
-3.41441590303255));
#50692=CARTESIAN_POINT('Ctrl Pts',(0.571402753704327,-0.413516361031052,
-3.3985583924566));
#50693=CARTESIAN_POINT('Ctrl Pts',(0.699540203905405,-0.0902241148542729,
-3.38270088188066));
#50694=CARTESIAN_POINT('Ctrl Pts',(0.657625632702926,0.255000813711106,
-3.36684337130472));
#50695=CARTESIAN_POINT('Ctrl Pts',(0.455848100739092,0.538237305315985,
-3.35098586072876));
#50696=CARTESIAN_POINT('Ctrl Pts',(0.143257937062477,0.690633080043126,
-3.33512835015283));
#50697=CARTESIAN_POINT('Ctrl Pts',(-0.204156960980475,0.675142076206533,
-3.31927083957688));
#50698=CARTESIAN_POINT('Ctrl Pts',(-0.501943111877064,0.495530019494702,
-3.30341332900094));
#50699=CARTESIAN_POINT('Ctrl Pts',(-0.652144945246755,0.239105887371835,
-3.28986237526898));
#50700=CARTESIAN_POINT('Ctrl Pts',(-0.67662482340183,0.0633437005471308,
-3.28159725839567));
#50701=CARTESIAN_POINT('Ctrl Pts',(-0.676646145701304,-6.48367876878927E-6,
-3.278617978381));
#50702=CARTESIAN_POINT('Ctrl Pts',(-0.676652143573121,-1.01282642557092E-5,
-3.43918202161899));
#50703=CARTESIAN_POINT('Ctrl Pts',(-0.676675846286291,-0.044590091349477,
-3.437085428446));
#50704=CARTESIAN_POINT('Ctrl Pts',(-0.661396035876845,-0.201547028199607,
-3.42970299841435));
#50705=CARTESIAN_POINT('Ctrl Pts',(-0.541383431856071,-0.452107139770282,
-3.41703473152406));
#50706=CARTESIAN_POINT('Ctrl Pts',(-0.259552071413764,-0.655842670420542,
-3.40117722094812));
#50707=CARTESIAN_POINT('Ctrl Pts',(0.0853740963848333,-0.700148662632442,
-3.38531971037218));
#50708=CARTESIAN_POINT('Ctrl Pts',(0.409546578284193,-0.574254722518878,
-3.36946219979623));
#50709=CARTESIAN_POINT('Ctrl Pts',(0.634161918067455,-0.308764550738151,
-3.35360468922029));
#50710=CARTESIAN_POINT('Ctrl Pts',(0.70461811808652,0.0317835458017981,
-3.33774717864434));
#50711=CARTESIAN_POINT('Ctrl Pts',(0.603787900785698,0.364605344152174,
-3.32188966806841));
#50712=CARTESIAN_POINT('Ctrl Pts',(0.356182198023997,0.608794815952237,
-3.30603215749246));
#50713=CARTESIAN_POINT('Ctrl Pts',(0.021991760855621,0.704991665606051,
-3.29017464691652));
#50714=CARTESIAN_POINT('Ctrl Pts',(-0.317544678396473,0.629811291849872,
-3.27431713634057));
#50715=CARTESIAN_POINT('Ctrl Pts',(-0.579888821700749,0.401529376990078,
-3.25845962576463));
#50716=CARTESIAN_POINT('Ctrl Pts',(-0.669533849297346,0.160840322501936,
-3.24674792085744));
#50717=CARTESIAN_POINT('Ctrl Pts',(-0.676730253963205,0.0242523298834378,
-3.24032205280889));
#50718=CARTESIAN_POINT('Ctrl Pts',(-0.676705321009976,1.72594551696367E-5,
-3.23918202161899));
#50719=CARTESIAN_POINT('Origin',(0.,0.,-6.17861797838101));
#50720=CARTESIAN_POINT('',(-0.676665289551903,1.43754394393928E-5,-3.678617978381));
#50721=CARTESIAN_POINT('',(-0.676757684388521,-1.06428210661091E-6,-3.639182021619));
#50722=CARTESIAN_POINT('',(-0.6767,7.27977111083166E-14,-6.17861797838101));
#50723=CARTESIAN_POINT('Ctrl Pts',(-0.676665289551903,1.43754394393916E-5,
-3.678617978381));
#50724=CARTESIAN_POINT('Ctrl Pts',(-0.676607739317337,-0.0742739175691506,
-3.67512400966988));
#50725=CARTESIAN_POINT('Ctrl Pts',(-0.645954239072405,-0.260995295744918,
-3.66634420410011));
#50726=CARTESIAN_POINT('Ctrl Pts',(-0.47732480187785,-0.519285972556088,
-3.65227856167169));
#50727=CARTESIAN_POINT('Ctrl Pts',(-0.171179682347504,-0.684247326726716,
-3.63642105109576));
#50728=CARTESIAN_POINT('Ctrl Pts',(0.176577700272081,-0.682874222348358,
-3.6205635405198));
#50729=CARTESIAN_POINT('Ctrl Pts',(0.48141060950412,-0.51550044892136,-3.60470602994387));
#50730=CARTESIAN_POINT('Ctrl Pts',(0.66921686778135,-0.222813086819806,
-3.58884851936792));
#50731=CARTESIAN_POINT('Ctrl Pts',(0.694342438818249,0.12403816121331,-3.57299100879198));
#50732=CARTESIAN_POINT('Ctrl Pts',(0.550679519060578,0.440736831985327,
-3.55713349821603));
#50733=CARTESIAN_POINT('Ctrl Pts',(0.273151290577277,0.650296286501176,
-3.54127598764009));
#50734=CARTESIAN_POINT('Ctrl Pts',(-0.0707775948694625,0.701774479334883,
-3.52541847706415));
#50735=CARTESIAN_POINT('Ctrl Pts',(-0.397501074521878,0.582657518217351,
-3.5095609664882));
#50736=CARTESIAN_POINT('Ctrl Pts',(-0.623861468045536,0.326133368546649,
-3.49396080026049));
#50737=CARTESIAN_POINT('Ctrl Pts',(-0.676706564337889,0.106869103155189,
-3.48364647089142));
#50738=CARTESIAN_POINT('Ctrl Pts',(-0.676753931151198,-5.65874007810076E-6,
-3.478617978381));
#50739=CARTESIAN_POINT('Ctrl Pts',(-0.676757684388521,-1.06428210658034E-6,
-3.639182021619));
#50740=CARTESIAN_POINT('Ctrl Pts',(-0.676757777269629,-0.00100806921878618,
-3.63913464094175));
#50741=CARTESIAN_POINT('Ctrl Pts',(-0.676510061530498,-0.114357529906071,
-3.63380142340587));
#50742=CARTESIAN_POINT('Ctrl Pts',(-0.618093122687726,-0.339790785345425,
-3.62318236901133));
#50743=CARTESIAN_POINT('Ctrl Pts',(-0.380605728184695,-0.593831765563718,
-3.60732485843538));
#50744=CARTESIAN_POINT('Ctrl Pts',(-0.0505964556334205,-0.703517508521898,
-3.59146734785944));
#50745=CARTESIAN_POINT('Ctrl Pts',(0.291712366691096,-0.642184382587279,
-3.5756098372835));
#50746=CARTESIAN_POINT('Ctrl Pts',(0.563108499012531,-0.424741926891352,
-3.55975232670755));
#50747=CARTESIAN_POINT('Ctrl Pts',(0.697617947778104,-0.104048474555806,
-3.54389481613161));
#50748=CARTESIAN_POINT('Ctrl Pts',(0.66254265856183,0.241938239444174,-3.52803730555567));
#50749=CARTESIAN_POINT('Ctrl Pts',(0.466409123192545,0.529111912474371,
-3.51217979497972));
#50750=CARTESIAN_POINT('Ctrl Pts',(0.156895665186708,0.687663170720335,
-3.49632228440378));
#50751=CARTESIAN_POINT('Ctrl Pts',(-0.19075773797954,0.679049609027539,
-3.48046477382783));
#50752=CARTESIAN_POINT('Ctrl Pts',(-0.492039626312628,0.505365107875141,
-3.4646072632519));
#50753=CARTESIAN_POINT('Ctrl Pts',(-0.649691444389947,0.248036967307317,
-3.45084634584895));
#50754=CARTESIAN_POINT('Ctrl Pts',(-0.676616088066844,0.067802916062758,
-3.44237126530465));
#50755=CARTESIAN_POINT('Ctrl Pts',(-0.676652143573121,-1.01282642557092E-5,
-3.43918202161899));
#50756=CARTESIAN_POINT('Origin',(0.,0.,-6.17861797838101));
#50757=CARTESIAN_POINT('',(-0.676685270745956,-1.71119534365975E-5,-3.878617978381));
#50758=CARTESIAN_POINT('',(-0.676655703468725,1.16019570828296E-5,-3.83918202161899));
#50759=CARTESIAN_POINT('',(-0.6767,7.27977111083166E-14,-6.17861797838101));
#50760=CARTESIAN_POINT('Ctrl Pts',(-0.676685270745956,-1.71119534366597E-5,
-3.878617978381));
#50761=CARTESIAN_POINT('Ctrl Pts',(-0.676714912134811,-0.0307327214839186,
-3.87717322216564));
#50762=CARTESIAN_POINT('Ctrl Pts',(-0.66715043232197,-0.173807244306441,
-3.87044262909162));
#50763=CARTESIAN_POINT('Ctrl Pts',(-0.568119486722484,-0.418015713325986,
-3.85842619915896));
#50764=CARTESIAN_POINT('Ctrl Pts',(-0.299328251646252,-0.638670091320746,
-3.84256868858302));
#50765=CARTESIAN_POINT('Ctrl Pts',(0.0422270275427583,-0.704069432603173,
-3.82671117800707));
#50766=CARTESIAN_POINT('Ctrl Pts',(0.373517290723508,-0.598315737142038,
-3.81085366743113));
#50767=CARTESIAN_POINT('Ctrl Pts',(0.614008812156318,-0.347116790685268,
-3.79499615685518));
#50768=CARTESIAN_POINT('Ctrl Pts',(0.705240235193272,-0.0115368299714127,
-3.77913864627925));
#50769=CARTESIAN_POINT('Ctrl Pts',(0.625034009757416,0.326847631822259,
-3.76328113570329));
#50770=CARTESIAN_POINT('Ctrl Pts',(0.392887558138946,0.585778332170854,
-3.74742362512736));
#50771=CARTESIAN_POINT('Ctrl Pts',(0.065233624501804,0.702311513514914,
-3.73156611455141));
#50772=CARTESIAN_POINT('Ctrl Pts',(-0.278278024886458,0.648118992659946,
-3.71570860397547));
#50773=CARTESIAN_POINT('Ctrl Pts',(-0.554142753654658,0.436374490951619,
-3.69985109339953));
#50774=CARTESIAN_POINT('Ctrl Pts',(-0.664198309185149,0.188578892491741,
-3.6874875515347));
#50775=CARTESIAN_POINT('Ctrl Pts',(-0.676694803963945,0.0381128350943536,
-3.68040984652853));
#50776=CARTESIAN_POINT('Ctrl Pts',(-0.676665289551903,1.43754394393916E-5,
-3.678617978381));
#50777=CARTESIAN_POINT('Ctrl Pts',(-0.676655703468725,1.16019570828574E-5,
-3.839182021619));
#50778=CARTESIAN_POINT('Ctrl Pts',(-0.676612882638414,-0.069815305702025,
-3.83589801657886));
#50779=CARTESIAN_POINT('Ctrl Pts',(-0.648551748397102,-0.252067159102267,
-3.82732817468008));
#50780=CARTESIAN_POINT('Ctrl Pts',(-0.487506623358711,-0.50973932387144,
-3.81347249592265));
#50781=CARTESIAN_POINT('Ctrl Pts',(-0.184685586744943,-0.680726171208512,
-3.79761498534671));
#50782=CARTESIAN_POINT('Ctrl Pts',(0.163030878572916,-0.686234521684292,
-3.78175747477076));
#50783=CARTESIAN_POINT('Ctrl Pts',(0.471115982751349,-0.524925344135482,
-3.76589996419482));
#50784=CARTESIAN_POINT('Ctrl Pts',(0.664676968465788,-0.236011469447257,
-3.75004245361887));
#50785=CARTESIAN_POINT('Ctrl Pts',(0.696660876212486,0.110274700971604,
-3.73418494304293));
#50786=CARTESIAN_POINT('Ctrl Pts',(0.559292701589483,0.429754069286446,
-3.71832743246699));
#50787=CARTESIAN_POINT('Ctrl Pts',(0.285965429933078,0.644764033583383,
-3.70246992189105));
#50788=CARTESIAN_POINT('Ctrl Pts',(-0.0568775023532221,0.703037577833207,
-3.6866124113151));
#50789=CARTESIAN_POINT('Ctrl Pts',(-0.385894018096841,0.590408920085563,
-3.67075490073916));
#50790=CARTESIAN_POINT('Ctrl Pts',(-0.620400337809798,0.335022444869625,
-3.65494477084045));
#50791=CARTESIAN_POINT('Ctrl Pts',(-0.67674741535816,0.111334432431026,
-3.6444204778004));
#50792=CARTESIAN_POINT('Ctrl Pts',(-0.676757684388521,-1.06428210658034E-6,
-3.639182021619));
#50793=CARTESIAN_POINT('Origin',(0.,0.,-6.17861797838101));
#50794=CARTESIAN_POINT('',(-0.676739110229135,1.21105064106007E-5,-4.078617978381));
#50795=CARTESIAN_POINT('',(-0.676698966456529,-1.74541653144567E-5,-4.039182021619));
#50796=CARTESIAN_POINT('',(-0.6767,7.27977111083166E-14,-6.17861797838101));
#50797=CARTESIAN_POINT('Ctrl Pts',(-0.676739110229135,1.21105064106054E-5,
-4.078617978381));
#50798=CARTESIAN_POINT('Ctrl Pts',(-0.676656380771256,-0.099491513469243,
-4.07393659780274));
#50799=CARTESIAN_POINT('Ctrl Pts',(-0.629347804780193,-0.31142265532354,
-4.06396938036584));
#50800=CARTESIAN_POINT('Ctrl Pts',(-0.416346348986597,-0.569344013287909,
-4.04871632607028));
#50801=CARTESIAN_POINT('Ctrl Pts',(-0.0936938502820333,-0.699083936448678,
-4.03285881549434));
#50802=CARTESIAN_POINT('Ctrl Pts',(0.251734792730736,-0.658882752779327,
-4.01700130491839));
#50803=CARTESIAN_POINT('Ctrl Pts',(0.535968939526595,-0.458513013603747,
-4.00114379434245));
#50804=CARTESIAN_POINT('Ctrl Pts',(0.689913789056643,-0.146682826025263,
-3.98528628376651));
#50805=CARTESIAN_POINT('Ctrl Pts',(0.676146713284492,0.200804656061129,
-3.96942877319056));
#50806=CARTESIAN_POINT('Ctrl Pts',(0.49801436627063,0.499478306605316,-3.95357126261462));
#50807=CARTESIAN_POINT('Ctrl Pts',(0.198819142241936,0.676733209218694,
-3.93771375203867));
#50808=CARTESIAN_POINT('Ctrl Pts',(-0.148707252523208,0.689480268628661,
-3.92185624146274));
#50809=CARTESIAN_POINT('Ctrl Pts',(-0.460084232647476,0.534620787708854,
-3.90599873088679));
#50810=CARTESIAN_POINT('Ctrl Pts',(-0.641439490611294,0.275749392064349,
-3.89158597652621));
#50811=CARTESIAN_POINT('Ctrl Pts',(-0.676606465087421,0.0816445081588362,
-3.88245905902428));
#50812=CARTESIAN_POINT('Ctrl Pts',(-0.676685270745956,-1.71119534366597E-5,
-3.878617978381));
#50813=CARTESIAN_POINT('Ctrl Pts',(-0.676698966456529,-1.74541653144393E-5,
-4.039182021619));
#50814=CARTESIAN_POINT('Ctrl Pts',(-0.676725765237266,-0.0262676949275742,
-4.03794722907462));
#50815=CARTESIAN_POINT('Ctrl Pts',(-0.668813390334722,-0.164872567242388,
-4.03142659967159));
#50816=CARTESIAN_POINT('Ctrl Pts',(-0.576279664676672,-0.406692308999895,
-4.01962013340991));
#50817=CARTESIAN_POINT('Ctrl Pts',(-0.311907214595146,-0.632622142833319,
-4.00376262283397));
#50818=CARTESIAN_POINT('Ctrl Pts',(0.0282871139661857,-0.70476714261023,
-3.98790511225803));
#50819=CARTESIAN_POINT('Ctrl Pts',(0.361605095917608,-0.6055894985268,-3.97204760168208));
#50820=CARTESIAN_POINT('Ctrl Pts',(0.607020085064156,-0.35919841654471,
-3.95619009110614));
#50821=CARTESIAN_POINT('Ctrl Pts',(0.704873873408482,-0.0254893841755349,
-3.9403325805302));
#50822=CARTESIAN_POINT('Ctrl Pts',(0.631379072581692,0.31441589149629,-3.92447506995425));
#50823=CARTESIAN_POINT('Ctrl Pts',(0.40440161705542,0.57788945157572,-3.90861755937831));
#50824=CARTESIAN_POINT('Ctrl Pts',(0.0791177138722245,0.700883209579997,
-3.89276004880237));
#50825=CARTESIAN_POINT('Ctrl Pts',(-0.265399004090862,0.653498473408395,
-3.87690253822642));
#50826=CARTESIAN_POINT('Ctrl Pts',(-0.545399577203117,0.447254052308289,
-3.86104502765048));
#50827=CARTESIAN_POINT('Ctrl Pts',(-0.662288714997138,0.197514295592761,
-3.84847152211467));
#50828=CARTESIAN_POINT('Ctrl Pts',(-0.676681805773553,0.0425760084765945,
-3.84118385343751));
#50829=CARTESIAN_POINT('Ctrl Pts',(-0.676655703468725,1.16019570828574E-5,
-3.839182021619));
#50830=CARTESIAN_POINT('Origin',(0.,0.,-6.17861797838101));
#50831=CARTESIAN_POINT('',(-0.676642404370006,-2.12118767964631E-7,-4.278617978381));
#50832=CARTESIAN_POINT('',(-0.676726753762749,1.49205000514463E-5,-4.239182021619));
#50833=CARTESIAN_POINT('',(-0.6767,7.27977111083166E-14,-6.17861797838101));
#50834=CARTESIAN_POINT('Ctrl Pts',(-0.676642404370006,-2.12118767984465E-7,
-4.27861797838101));
#50835=CARTESIAN_POINT('Ctrl Pts',(-0.676643016530589,-0.0559704364681642,
-4.2759858102985));
#50836=CARTESIAN_POINT('Ctrl Pts',(-0.655986276549325,-0.22433785474264,
-4.26806780535735));
#50837=CARTESIAN_POINT('Ctrl Pts',(-0.517882675605679,-0.478846971472886,
-4.25486396355754));
#50838=CARTESIAN_POINT('Ctrl Pts',(-0.226130737646503,-0.668103118741933,
-4.23900645298161));
#50839=CARTESIAN_POINT('Ctrl Pts',(0.120591577745708,-0.694949321287569,
-4.22314894240565));
#50840=CARTESIAN_POINT('Ctrl Pts',(0.437999149760179,-0.552859505291001,
-4.20729143182972));
#50841=CARTESIAN_POINT('Ctrl Pts',(0.648933011794961,-0.276374445244078,
-4.19143392125377));
#50842=CARTESIAN_POINT('Ctrl Pts',(0.702117012141806,0.0672947920890993,
-4.17557641067783));
#50843=CARTESIAN_POINT('Ctrl Pts',(0.584622591848963,0.394605262105121,
-4.15971890010188));
#50844=CARTESIAN_POINT('Ctrl Pts',(0.325011602776974,0.625990691497561,
-4.14386138952594));
#50845=CARTESIAN_POINT('Ctrl Pts',(-0.0136068253575281,0.705203333858357,
-4.12800387895));
#50846=CARTESIAN_POINT('Ctrl Pts',(-0.348917554886554,0.612987298133689,
-4.11214636837405));
#50847=CARTESIAN_POINT('Ctrl Pts',(-0.599409520346848,0.371759485015262,
-4.09628885779812));
#50848=CARTESIAN_POINT('Ctrl Pts',(-0.673257437461863,0.138053426064092,
-4.08511272780042));
#50849=CARTESIAN_POINT('Ctrl Pts',(-0.676749792193473,0.0128599423431918,
-4.07922243466139));
#50850=CARTESIAN_POINT('Ctrl Pts',(-0.676739110229135,1.21105064106054E-5,
-4.078617978381));
#50851=CARTESIAN_POINT('Ctrl Pts',(-0.676726753762749,1.49205000514446E-5,
-4.239182021619));
#50852=CARTESIAN_POINT('Ctrl Pts',(-0.676635341683233,-0.0950309047916752,
-4.23471060471172));
#50853=CARTESIAN_POINT('Ctrl Pts',(-0.632525590471087,-0.302516277141406,
-4.2249533509458));
#50854=CARTESIAN_POINT('Ctrl Pts',(-0.427530623812185,-0.560994163804123,
-4.20991026032124));
#50855=CARTESIAN_POINT('Ctrl Pts',(-0.107508502335302,-0.697093112894644,
-4.19405274974529));
#50856=CARTESIAN_POINT('Ctrl Pts',(0.238647982882395,-0.663734906710268,
-4.17819523916935));
#50857=CARTESIAN_POINT('Ctrl Pts',(0.526791259328862,-0.469028629418541,
-4.1623377285934));
#50858=CARTESIAN_POINT('Ctrl Pts',(0.68687625119572,-0.160305650751426,
-4.14648021801746));
#50859=CARTESIAN_POINT('Ctrl Pts',(0.679987716283376,0.187386210333744,
-4.13062270744152));
#50860=CARTESIAN_POINT('Ctrl Pts',(0.507800196354854,0.489526145064282,
-4.11476519686557));
#50861=CARTESIAN_POINT('Ctrl Pts',(0.212170950879785,0.672666614098168,
-4.09890768628963));
#50862=CARTESIAN_POINT('Ctrl Pts',(-0.135035171633647,0.692287793147759,
-4.08305017571368));
#50863=CARTESIAN_POINT('Ctrl Pts',(-0.449415441152957,0.543619947548669,
-4.06719266513775));
#50864=CARTESIAN_POINT('Ctrl Pts',(-0.63857363386037,0.28466957177687,-4.05256994710618));
#50865=CARTESIAN_POINT('Ctrl Pts',(-0.676611046385397,0.0861029950325273,
-4.04323306593326));
#50866=CARTESIAN_POINT('Ctrl Pts',(-0.676698966456529,-1.74541653144393E-5,
-4.039182021619));
#50867=CARTESIAN_POINT('Origin',(0.,0.,-6.17861797838101));
#50868=CARTESIAN_POINT('',(-0.676740262348679,-1.17706457744123E-5,-4.478617978381));
#50869=CARTESIAN_POINT('',(-0.676644019679501,-4.3116399903731E-6,-4.439182021619));
#50870=CARTESIAN_POINT('',(-0.6767,7.27977111083166E-14,-6.17861797838101));
#50871=CARTESIAN_POINT('Ctrl Pts',(-0.676740262348678,-1.17706457744317E-5,
-4.478617978381));
#50872=CARTESIAN_POINT('Ctrl Pts',(-0.676750346481431,-0.0124025401036787,
-4.47803502279425));
#50873=CARTESIAN_POINT('Ctrl Pts',(-0.673394647811649,-0.137138751468068,
-4.47216623034886));
#50874=CARTESIAN_POINT('Ctrl Pts',(-0.600161619846482,-0.370544083537301,
-4.46101160104481));
#50875=CARTESIAN_POINT('Ctrl Pts',(-0.350158990608888,-0.61227899610963,
-4.44515409046887));
#50876=CARTESIAN_POINT('Ctrl Pts',(-0.0150358152851096,-0.705174313230397,
-4.42929657989292));
#50877=CARTESIAN_POINT('Ctrl Pts',(0.32374243342603,-0.626648006923061,
-4.41343906931699));
#50878=CARTESIAN_POINT('Ctrl Pts',(0.583821766891339,-0.39578912603194,
-4.39758155874103));
#50879=CARTESIAN_POINT('Ctrl Pts',(0.701979205024536,-0.0687174176928368,
-4.3817240481651));
#50880=CARTESIAN_POINT('Ctrl Pts',(0.649491722206451,0.275058885634601,
-4.36586653758914));
#50881=CARTESIAN_POINT('Ctrl Pts',(0.439118560152959,0.551970812553023,
-4.35000902701321));
#50882=CARTESIAN_POINT('Ctrl Pts',(0.121999569378052,0.694703528746487,
-4.33415151643726));
#50883=CARTESIAN_POINT('Ctrl Pts',(-0.224776435057083,0.668559976385276,
-4.31829400586132));
#50884=CARTESIAN_POINT('Ctrl Pts',(-0.516911281011339,0.479895421258078,
-4.30243649528538));
#50885=CARTESIAN_POINT('Ctrl Pts',(-0.65575605607782,0.225252701430372,
-4.28921115279194));
#50886=CARTESIAN_POINT('Ctrl Pts',(-0.676641787209029,0.0564272013647705,
-4.28127164715715));
#50887=CARTESIAN_POINT('Ctrl Pts',(-0.676642404370006,-2.12118767984465E-7,
-4.27861797838101));
#50888=CARTESIAN_POINT('Ctrl Pts',(-0.676644019679501,-4.31163999035922E-6,
-4.439182021619));
#50889=CARTESIAN_POINT('Ctrl Pts',(-0.676655503400418,-0.0515095321842119,
-4.43675981720748));
#50890=CARTESIAN_POINT('Ctrl Pts',(-0.658181313981681,-0.215403514966007,
-4.42905177593732));
#50891=CARTESIAN_POINT('Ctrl Pts',(-0.527256376882394,-0.468505708776717,
-4.41605789780849));
#50892=CARTESIAN_POINT('Ctrl Pts',(-0.239306432604977,-0.663497790074244,
-4.40020038723256));
#50893=CARTESIAN_POINT('Ctrl Pts',(0.106816783733375,-0.697199441216343,
-4.38434287665661));
#50894=CARTESIAN_POINT('Ctrl Pts',(0.426973786990221,-0.561418089611258,
-4.36848536608067));
#50895=CARTESIAN_POINT('Ctrl Pts',(0.64333724820522,-0.289160977988487,
-4.35262785550472));
#50896=CARTESIAN_POINT('Ctrl Pts',(0.703311128248571,0.0533886036645251,
-4.33677034492878));
#50897=CARTESIAN_POINT('Ctrl Pts',(0.592316308613785,0.382959889113288,
-4.32091283435284));
#50898=CARTESIAN_POINT('Ctrl Pts',(0.337334645867288,0.619437020864201,
-4.3050553237769));
#50899=CARTESIAN_POINT('Ctrl Pts',(0.000349921539867571,0.7053345048092,
-4.28919781320095));
#50900=CARTESIAN_POINT('Ctrl Pts',(-0.336719865611468,0.619771424173557,
-4.27334030262501));
#50901=CARTESIAN_POINT('Ctrl Pts',(-0.591936038811396,0.383547405252334,
-4.25748279204906));
#50902=CARTESIAN_POINT('Ctrl Pts',(-0.671867885490126,0.146986079704804,
-4.2460966983804));
#50903=CARTESIAN_POINT('Ctrl Pts',(-0.676743403478689,0.0173264837064653,
-4.23999644157037));
#50904=CARTESIAN_POINT('Ctrl Pts',(-0.676726753762749,1.49205000514446E-5,
-4.239182021619));
#50905=CARTESIAN_POINT('Origin',(0.,0.,-6.17861797838101));
#50906=CARTESIAN_POINT('',(-0.676683918556463,1.70183238131909E-5,-4.678617978381));
#50907=CARTESIAN_POINT('',(-0.67675000022537,-8.01283250001505E-6,-4.639182021619));
#50908=CARTESIAN_POINT('',(-0.6767,7.27977111083166E-14,-6.17861797838101));
#50909=CARTESIAN_POINT('Ctrl Pts',(-0.676683918556463,1.7018323813206E-5,
-4.678617978381));
#50910=CARTESIAN_POINT('Ctrl Pts',(-0.676606241781625,-0.0811879617933027,
-4.67479839843136));
#50911=CARTESIAN_POINT('Ctrl Pts',(-0.64172719032616,-0.274835745774313,
-4.66569298162307));
#50912=CARTESIAN_POINT('Ctrl Pts',(-0.461166638918949,-0.533687379398699,
-4.65130172795613));
#50913=CARTESIAN_POINT('Ctrl Pts',(-0.15010410398989,-0.689177513958953,
-4.63544421738019));
#50914=CARTESIAN_POINT('Ctrl Pts',(0.197447407787028,-0.677134705165401,
-4.61958670680424));
#50915=CARTESIAN_POINT('Ctrl Pts',(0.497001205311606,-0.500486453063479,
-4.6037291962283));
#50916=CARTESIAN_POINT('Ctrl Pts',(0.675738416267745,-0.202174381565054,
-4.58787168565236));
#50917=CARTESIAN_POINT('Ctrl Pts',(0.690209609366951,0.145284489601514,
-4.57201417507641));
#50918=CARTESIAN_POINT('Ctrl Pts',(0.536896965869284,0.457425989447045,
-4.55615666450047));
#50919=CARTESIAN_POINT('Ctrl Pts',(0.253069430129838,0.658371286824547,
-4.54029915392453));
#50920=CARTESIAN_POINT('Ctrl Pts',(-0.0922770403452622,0.699272361534738,
-4.52444164334858));
#50921=CARTESIAN_POINT('Ctrl Pts',(-0.415191780446262,0.570186524946981,
-4.50858413277264));
#50922=CARTESIAN_POINT('Ctrl Pts',(-0.629016431300928,0.312334364230696,
-4.49330957778344));
#50923=CARTESIAN_POINT('Ctrl Pts',(-0.67665891056109,0.0999483617424532,
-4.4833208596529));
#50924=CARTESIAN_POINT('Ctrl Pts',(-0.676740262348678,-1.17706457744317E-5,
-4.478617978381));
#50925=CARTESIAN_POINT('Ctrl Pts',(-0.67675000022537,-8.01283250002199E-6,
-4.639182021619));
#50926=CARTESIAN_POINT('Ctrl Pts',(-0.676754741008023,-0.00793565612024164,
-4.63880902970323));
#50927=CARTESIAN_POINT('Ctrl Pts',(-0.674685149586979,-0.128207033147944,
-4.63315020092882));
#50928=CARTESIAN_POINT('Ctrl Pts',(-0.607376188029295,-0.358595945786518,
-4.62220553529577));
#50929=CARTESIAN_POINT('Ctrl Pts',(-0.362205792415875,-0.605230410719679,
-4.60634802471981));
#50930=CARTESIAN_POINT('Ctrl Pts',(-0.0289863800046666,-0.704738728816396,
-4.59049051414388));
#50931=CARTESIAN_POINT('Ctrl Pts',(0.311279364390673,-0.632931310194133,
-4.57463300356793));
#50932=CARTESIAN_POINT('Ctrl Pts',(0.575875855124356,-0.407263901671038,
-4.55877549299199));
#50933=CARTESIAN_POINT('Ctrl Pts',(0.700482031227543,-0.0825942494781502,
-4.54291798241604));
#50934=CARTESIAN_POINT('Ctrl Pts',(0.654807236055464,0.262153332477254,
-4.5270604718401));
#50935=CARTESIAN_POINT('Ctrl Pts',(0.449954607358944,0.543173763574772,
-4.51120296126416));
#50936=CARTESIAN_POINT('Ctrl Pts',(0.13572200293829,0.692153468558775,-4.49534545068821));
#50937=CARTESIAN_POINT('Ctrl Pts',(-0.211503417077158,0.672876802010746,
-4.47948794011228));
#50938=CARTESIAN_POINT('Ctrl Pts',(-0.507314231603265,0.49002975066042,
-4.46363042953633));
#50939=CARTESIAN_POINT('Ctrl Pts',(-0.653454360935392,0.234185989462344,
-4.4501951233719));
#50940=CARTESIAN_POINT('Ctrl Pts',(-0.676630443139192,0.0608873373247691,
-4.44204565406613));
#50941=CARTESIAN_POINT('Ctrl Pts',(-0.676644019679501,-4.31163999035922E-6,
-4.439182021619));
#50942=CARTESIAN_POINT('Origin',(0.,0.,-6.17861797838101));
#50943=CARTESIAN_POINT('',(-0.676666391545702,-1.46161483497048E-5,-4.878617978381));
#50944=CARTESIAN_POINT('',(-0.676671450604501,1.55654194976124E-5,-4.839182021619));
#50945=CARTESIAN_POINT('',(-0.6767,7.27977111083166E-14,-6.17861797838101));
#50946=CARTESIAN_POINT('Ctrl Pts',(-0.676666391545702,-1.46161483497304E-5,
-4.87861797838101));
#50947=CARTESIAN_POINT('Ctrl Pts',(-0.676696108666216,-0.0376557552017236,
-4.87684761092712));
#50948=CARTESIAN_POINT('Ctrl Pts',(-0.664388562722288,-0.187663893074887,
-4.86979140661458));
#50949=CARTESIAN_POINT('Ctrl Pts',(-0.555025881375534,-0.435250684990344,
-4.85744936544339));
#50950=CARTESIAN_POINT('Ctrl Pts',(-0.279590796199469,-0.647553761831247,
-4.84159185486746));
#50951=CARTESIAN_POINT('Ctrl Pts',(0.0638103326637412,-0.702442260421875,
-4.8257343442915));
#50952=CARTESIAN_POINT('Ctrl Pts',(0.391699735402671,-0.586573273399606,
-4.80987683371557));
#50953=CARTESIAN_POINT('Ctrl Pts',(0.624370405298808,-0.32811352420809,
-4.79401932313962));
#50954=CARTESIAN_POINT('Ctrl Pts',(0.705262165372666,0.0101077136440157,
-4.77816181256367));
#50955=CARTESIAN_POINT('Ctrl Pts',(0.614710945941539,0.345871855924866,
-4.76230430198774));
#50956=CARTESIAN_POINT('Ctrl Pts',(0.374728945616527,0.597557616551221,
-4.74644679141179));
#50957=CARTESIAN_POINT('Ctrl Pts',(0.0436536609816854,0.703982418576024,
-4.73058928083585));
#50958=CARTESIAN_POINT('Ctrl Pts',(-0.298033441601801,0.639275336195787,
-4.71473177025991));
#50959=CARTESIAN_POINT('Ctrl Pts',(-0.567271256914447,0.419166087440235,
-4.69887425968396));
#50960=CARTESIAN_POINT('Ctrl Pts',(-0.666974939736738,0.17472219918873,
-4.68683632905766));
#50961=CARTESIAN_POINT('Ctrl Pts',(-0.676713737046788,0.0311899129122367,
-4.68008423529001));
#50962=CARTESIAN_POINT('Ctrl Pts',(-0.676683918556463,1.7018323813206E-5,
-4.678617978381));
#50963=CARTESIAN_POINT('Ctrl Pts',(-0.676671450604501,1.55654194976401E-5,
-4.839182021619));
#50964=CARTESIAN_POINT('Ctrl Pts',(-0.67660621972088,-0.076729606307988,
-4.83557240534034));
#50965=CARTESIAN_POINT('Ctrl Pts',(-0.64448073360313,-0.265911822706924,
-4.82667695220303));
#50966=CARTESIAN_POINT('Ctrl Pts',(-0.471636589224496,-0.524457637778504,
-4.81249566220709));
#50967=CARTESIAN_POINT('Ctrl Pts',(-0.163711689954952,-0.686072422337189,
-4.79663815163114));
#50968=CARTESIAN_POINT('Ctrl Pts',(0.184010069664874,-0.680909083785385,
-4.7807806410552));
#50969=CARTESIAN_POINT('Ctrl Pts',(0.487000612793599,-0.510222783946564,
-4.76492313047925));
#50970=CARTESIAN_POINT('Ctrl Pts',(0.671605624729155,-0.215505848996464,
-4.74906561990332));
#50971=CARTESIAN_POINT('Ctrl Pts',(0.692949263789228,0.131598647156757,
-4.73320810932736));
#50972=CARTESIAN_POINT('Ctrl Pts',(0.545843080552321,0.446712678947753,
-4.71735059875143));
#50973=CARTESIAN_POINT('Ctrl Pts',(0.266047283910979,0.653234819068239,
-4.70149308817548));
#50974=CARTESIAN_POINT('Ctrl Pts',(-0.0784222486577756,0.700961366292738,
-4.68563557759954));
#50975=CARTESIAN_POINT('Ctrl Pts',(-0.403828027874236,0.578290420137434,
-4.66977806702359));
#50976=CARTESIAN_POINT('Ctrl Pts',(-0.625721804684535,0.321234184394516,
-4.65429354836342));
#50977=CARTESIAN_POINT('Ctrl Pts',(-0.676687557236402,0.104410556549851,
-4.64409486656188));
#50978=CARTESIAN_POINT('Ctrl Pts',(-0.67675000022537,-8.01283250002199E-6,
-4.639182021619));
#50979=CARTESIAN_POINT('Origin',(0.,0.,-6.17861797838101));
#50980=CARTESIAN_POINT('',(-0.67675329042481,6.10867791108173E-6,-5.078617978381));
#50981=CARTESIAN_POINT('',(-0.67667814830283,-1.64852909755597E-5,-5.039182021619));
#50982=CARTESIAN_POINT('',(-0.6767,7.27977111083166E-14,-6.17861797838101));
#50983=CARTESIAN_POINT('Ctrl Pts',(-0.67675329042481,6.10867791109304E-6,
-5.078617978381));
#50984=CARTESIAN_POINT('Ctrl Pts',(-0.676702849224836,-0.106411973995982,
-5.07361098656422));
#50985=CARTESIAN_POINT('Ctrl Pts',(-0.624209800255466,-0.325222693532886,
-5.06331815788879));
#50986=CARTESIAN_POINT('Ctrl Pts',(-0.398680950495202,-0.581850829245344,
-5.04773949235472));
#50987=CARTESIAN_POINT('Ctrl Pts',(-0.0721995192170595,-0.701629615399804,
-5.03188198177877));
#50988=CARTESIAN_POINT('Ctrl Pts',(0.271832975057436,-0.650848462741271,
-5.01602447120283));
#50989=CARTESIAN_POINT('Ctrl Pts',(0.549785283183103,-0.441851819252255,
-5.00016696062688));
#50990=CARTESIAN_POINT('Ctrl Pts',(0.694089663396602,-0.125444915988027,
-4.98430945005094));
#50991=CARTESIAN_POINT('Ctrl Pts',(0.669667000279414,0.221456534150661,
-4.968451939475));
#50992=CARTESIAN_POINT('Ctrl Pts',(0.482454226702515,0.514523864284379,
-4.95259442889905));
#50993=CARTESIAN_POINT('Ctrl Pts',(0.177961108082654,0.682515004810329,
-4.93673691832311));
#50994=CARTESIAN_POINT('Ctrl Pts',(-0.169792778098127,0.684592798886295,
-4.92087940774717));
#50995=CARTESIAN_POINT('Ctrl Pts',(-0.476271545316318,0.520252153194254,
-4.90502189717122));
#50996=CARTESIAN_POINT('Ctrl Pts',(-0.645682600184146,0.261909416791567,
-4.89093475404917));
#50997=CARTESIAN_POINT('Ctrl Pts',(-0.676607381407591,0.0747304727380146,
-4.88213344778577));
#50998=CARTESIAN_POINT('Ctrl Pts',(-0.676666391545702,-1.46161483497304E-5,
-4.87861797838101));
#50999=CARTESIAN_POINT('Ctrl Pts',(-0.67667814830283,-1.64852909755875E-5,
-5.039182021619));
#51000=CARTESIAN_POINT('Ctrl Pts',(-0.676708467968247,-0.0331917720224041,
-5.03762161783609));
#51001=CARTESIAN_POINT('Ctrl Pts',(-0.666195069508018,-0.178728635692127,
-5.03077537719454));
#51002=CARTESIAN_POINT('Ctrl Pts',(-0.563529656794226,-0.424182993568702,
-5.01864329969435));
#51003=CARTESIAN_POINT('Ctrl Pts',(-0.292349407557091,-0.641894625324549,
-5.00278578911841));
#51004=CARTESIAN_POINT('Ctrl Pts',(0.0498983906696054,-0.703567364740653,
-4.98692827854246));
#51005=CARTESIAN_POINT('Ctrl Pts',(0.380016332526679,-0.594209115659208,
-4.97107076796653));
#51006=CARTESIAN_POINT('Ctrl Pts',(0.617755673194353,-0.340403898855044,
-4.95521325739056));
#51007=CARTESIAN_POINT('Ctrl Pts',(0.705324086767725,-0.00384951228082019,
-4.93935574681464));
#51008=CARTESIAN_POINT('Ctrl Pts',(0.621434468293966,0.333640656598862,
-4.92349823623868));
#51009=CARTESIAN_POINT('Ctrl Pts',(0.386479640253609,0.590025739937645,
-4.90764072566275));
#51010=CARTESIAN_POINT('Ctrl Pts',(0.0575750382195188,0.702980797101559,
-4.8917832150868));
#51011=CARTESIAN_POINT('Ctrl Pts',(-0.285325545141958,0.645047455160447,
-4.87592570451086));
#51012=CARTESIAN_POINT('Ctrl Pts',(-0.558866018193005,0.430308795899666,
-4.86006819393491));
#51013=CARTESIAN_POINT('Ctrl Pts',(-0.665210108609933,0.183657329584508,
-4.84782029963763));
#51014=CARTESIAN_POINT('Ctrl Pts',(-0.676701742286812,0.0356542112847855,
-4.84085824219899));
#51015=CARTESIAN_POINT('Ctrl Pts',(-0.676671450604501,1.55654194976401E-5,
-4.839182021619));
#51016=CARTESIAN_POINT('Origin',(0.,0.,-6.17861797838101));
#51017=CARTESIAN_POINT('',(-0.676645685622293,6.08692033333708E-6,-5.278617978381));
#51018=CARTESIAN_POINT('',(-0.676744992161023,1.01792954273136E-5,-5.239182021619));
#51019=CARTESIAN_POINT('',(-0.6767,7.27977111083166E-14,-6.17861797838101));
#51020=CARTESIAN_POINT('Ctrl Pts',(-0.676645685622293,6.08692033332928E-6,
-5.278617978381));
#51021=CARTESIAN_POINT('Ctrl Pts',(-0.676625829214806,-0.0628870377702795,
-5.27566019905998));
#51022=CARTESIAN_POINT('Ctrl Pts',(-0.652390634777465,-0.238191234465806,
-5.2674165828803));
#51023=CARTESIAN_POINT('Ctrl Pts',(-0.502946219016085,-0.49451186897655,
-5.25388712984198));
#51024=CARTESIAN_POINT('Ctrl Pts',(-0.205524643813888,-0.674726988171084,
-5.23802961926603));
#51025=CARTESIAN_POINT('Ctrl Pts',(0.141858150105515,-0.690921958711615,
-5.2221721086901));
#51026=CARTESIAN_POINT('Ctrl Pts',(0.454756485457226,-0.539159926845312,
-5.20631459811414));
#51027=CARTESIAN_POINT('Ctrl Pts',(0.65710755109285,-0.256332896987509,
-5.19045708753821));
#51028=CARTESIAN_POINT('Ctrl Pts',(0.699721597013181,0.0888063874649557,
-5.17459957696226));
#51029=CARTESIAN_POINT('Ctrl Pts',(0.572239526473699,0.412357626487503,
-5.15874206638632));
#51030=CARTESIAN_POINT('Ctrl Pts',(0.30565110055879,0.635668382498652,-5.14288455581037));
#51031=CARTESIAN_POINT('Ctrl Pts',(-0.035238397980778,0.704453790598787,
-5.12702704523444));
#51032=CARTESIAN_POINT('Ctrl Pts',(-0.367561754396992,0.601992727934364,
-5.11116953465848));
#51033=CARTESIAN_POINT('Ctrl Pts',(-0.610534107144088,0.353192570413113,
-5.09531202408255));
#51034=CARTESIAN_POINT('Ctrl Pts',(-0.675234784868236,0.124202376260447,
-5.08446150532338));
#51035=CARTESIAN_POINT('Ctrl Pts',(-0.676756099552333,0.00593265216038066,
-5.07889682342287));
#51036=CARTESIAN_POINT('Ctrl Pts',(-0.67675329042481,6.10867791109304E-6,
-5.078617978381));
#51037=CARTESIAN_POINT('Ctrl Pts',(-0.676744992161023,1.01792954273032E-5,
-5.239182021619));
#51038=CARTESIAN_POINT('Ctrl Pts',(-0.67667085383716,-0.101948986768809,
-5.2343849934732));
#51039=CARTESIAN_POINT('Ctrl Pts',(-0.627552308620193,-0.316325790578849,
-5.22430212846876));
#51040=CARTESIAN_POINT('Ctrl Pts',(-0.410116160373992,-0.573848081916823,
-5.20893342660567));
#51041=CARTESIAN_POINT('Ctrl Pts',(-0.0860687518011682,-0.700063608597757,
-5.19307591602972));
#51042=CARTESIAN_POINT('Ctrl Pts',(0.25890120724375,-0.656099878834963,
-5.17721840545379));
#51043=CARTESIAN_POINT('Ctrl Pts',(0.540934578241509,-0.452644085548684,
-5.16136089487784));
#51044=CARTESIAN_POINT('Ctrl Pts',(0.691471549227516,-0.139154528235421,
-5.1455033843019));
#51045=CARTESIAN_POINT('Ctrl Pts',(0.673917917224984,0.208162261139392,
-5.12964587372595));
#51046=CARTESIAN_POINT('Ctrl Pts',(0.492540814542161,0.504876650410443,
-5.11378836315001));
#51047=CARTESIAN_POINT('Ctrl Pts',(0.191431406740854,0.678860002233702,
-5.09793085257407));
#51048=CARTESIAN_POINT('Ctrl Pts',(-0.156213278796698,0.687818506327875,
-5.08207334199812));
#51049=CARTESIAN_POINT('Ctrl Pts',(-0.465883901255171,0.529574429774311,
-5.06621583142218));
#51050=CARTESIAN_POINT('Ctrl Pts',(-0.642974403145626,0.27083467858935,
-5.05191872462914));
#51051=CARTESIAN_POINT('Ctrl Pts',(-0.676605760703141,0.0791888536353506,
-5.04290745469474));
#51052=CARTESIAN_POINT('Ctrl Pts',(-0.67667814830283,-1.64852909755875E-5,
-5.039182021619));
#51053=CARTESIAN_POINT('Origin',(0.,0.,-6.17861797838101));
#51054=CARTESIAN_POINT('',(-0.676720731008515,-1.58587921748656E-5,-5.47861797838101));
#51055=CARTESIAN_POINT('',(-0.676642766387654,2.06514063441632E-6,-5.439182021619));
#51056=CARTESIAN_POINT('',(-0.6767,7.27977111083166E-14,-6.17861797838101));
#51057=CARTESIAN_POINT('Ctrl Pts',(-0.676720731008515,-1.58587921748089E-5,
-5.47861797838101));
#51058=CARTESIAN_POINT('Ctrl Pts',(-0.676739988800954,-0.0193291336136783,
-5.47770941155573));
#51059=CARTESIAN_POINT('Ctrl Pts',(-0.67121548086959,-0.150991703321477,
-5.47151500787181));
#51060=CARTESIAN_POINT('Ctrl Pts',(-0.588509514849396,-0.388784565910968,
-5.46003476732924));
#51061=CARTESIAN_POINT('Ctrl Pts',(-0.331207368228394,-0.622734748534038,
-5.4441772567533));
#51062=CARTESIAN_POINT('Ctrl Pts',(0.00660835310116418,-0.705303634925465,
-5.42831974617736));
#51063=CARTESIAN_POINT('Ctrl Pts',(0.342817642383509,-0.616419460965605,
-5.41246223560141));
#51064=CARTESIAN_POINT('Ctrl Pts',(0.595691002243588,-0.377689181239748,
-5.39660472502547));
#51065=CARTESIAN_POINT('Ctrl Pts',(0.703757160891212,-0.0471460101786735,
-5.38074721444953));
#51066=CARTESIAN_POINT('Ctrl Pts',(0.64074619327961,0.294857937962055,-5.36488970387358));
#51067=CARTESIAN_POINT('Ctrl Pts',(0.421975506976434,0.565184535610204,
-5.34903219329764));
#51068=CARTESIAN_POINT('Ctrl Pts',(0.100626316187652,0.698119783613068,
-5.3331746827217));
#51069=CARTESIAN_POINT('Ctrl Pts',(-0.245184239907299,0.661348301791295,
-5.31731717214575));
#51070=CARTESIAN_POINT('Ctrl Pts',(-0.531392681099133,0.463808911358507,
-5.30145966156981));
#51071=CARTESIAN_POINT('Ctrl Pts',(-0.659134379441101,0.211397173063012,
-5.2885599303149));
#51072=CARTESIAN_POINT('Ctrl Pts',(-0.676661314529693,0.0495090406936801,
-5.28094603591862));
#51073=CARTESIAN_POINT('Ctrl Pts',(-0.676645685622293,6.08692033332928E-6,
-5.278617978381));
#51074=CARTESIAN_POINT('Ctrl Pts',(-0.676642766387654,2.06514063443713E-6,
-5.439182021619));
#51075=CARTESIAN_POINT('Ctrl Pts',(-0.676636540647253,-0.0584271905943807,
-5.43643420596896));
#51076=CARTESIAN_POINT('Ctrl Pts',(-0.654736005126173,-0.229258492031468,
-5.42840055346027));
#51077=CARTESIAN_POINT('Ctrl Pts',(-0.512632811011637,-0.484463091673161,
-5.41508106409294));
#51078=CARTESIAN_POINT('Ctrl Pts',(-0.218835441848411,-0.670528101954526,
-5.39922355351699));
#51079=CARTESIAN_POINT('Ctrl Pts',(0.128158883019949,-0.693593675592924,
-5.38336604294105));
#51080=CARTESIAN_POINT('Ctrl Pts',(0.443998919690547,-0.548052776138566,
-5.3675085323651));
#51081=CARTESIAN_POINT('Ctrl Pts',(0.651906755505725,-0.269285105873896,
-5.35165102178917));
#51082=CARTESIAN_POINT('Ctrl Pts',(0.701341838902262,0.0749433861305649,
-5.33579351121321));
#51083=CARTESIAN_POINT('Ctrl Pts',(0.580286939400919,0.400953805419331,
-5.31993600063728));
#51084=CARTESIAN_POINT('Ctrl Pts',(0.31816942979039,0.62949590949138,-5.30407849006133));
#51085=CARTESIAN_POINT('Ctrl Pts',(-0.0212922472927337,0.705013139114975,
-5.28822097948539));
#51086=CARTESIAN_POINT('Ctrl Pts',(-0.355577967837347,0.609147925308939,
-5.27236346890944));
#51087=CARTESIAN_POINT('Ctrl Pts',(-0.603425836976519,0.365204251602734,
-5.2565059583335));
#51088=CARTESIAN_POINT('Ctrl Pts',(-0.673984377760133,0.13313369579333,
-5.24544547590335));
#51089=CARTESIAN_POINT('Ctrl Pts',(-0.676752546725549,0.0103996386049762,
-5.23967083033185));
#51090=CARTESIAN_POINT('Ctrl Pts',(-0.676744992161023,1.01792954273032E-5,
-5.239182021619));
#51091=CARTESIAN_POINT('Origin',(0.,0.,-6.17861797838101));
#51092=CARTESIAN_POINT('',(-0.676705286336412,1.7378251266052E-5,-5.678617978381));
#51093=CARTESIAN_POINT('',(-0.676733793626987,-1.34876458774968E-5,-5.63918202161899));
#51094=CARTESIAN_POINT('',(-0.6767,7.27977111083166E-14,-6.17861797838101));
#51095=CARTESIAN_POINT('Ctrl Pts',(-0.676705286336412,1.73782512660377E-5,
-5.678617978381));
#51096=CARTESIAN_POINT('Ctrl Pts',(-0.676614630128216,-0.088102164827456,
-5.67447278719284));
#51097=CARTESIAN_POINT('Ctrl Pts',(-0.637255231935198,-0.288668254515342,
-5.66504175914603));
#51098=CARTESIAN_POINT('Ctrl Pts',(-0.444574205494435,-0.547586123312261,
-5.65032489424056));
#51099=CARTESIAN_POINT('Ctrl Pts',(-0.128887172109694,-0.69345876028638,
-5.63446738366463));
#51100=CARTESIAN_POINT('Ctrl Pts',(0.218131180300111,-0.670757513336377,
-5.61860987308867));
#51101=CARTESIAN_POINT('Ctrl Pts',(0.512123781755499,-0.485001168094135,
-5.60275236251274));
#51102=CARTESIAN_POINT('Ctrl Pts',(0.681623629821306,-0.181345284572452,
-5.58689485193679));
#51103=CARTESIAN_POINT('Ctrl Pts',(0.685426818106913,0.166394001985959,
-5.57103734136085));
#51104=CARTESIAN_POINT('Ctrl Pts',(0.522608823274475,0.47368439616164,-5.5551798307849));
#51105=CARTESIAN_POINT('Ctrl Pts',(0.232749257329435,0.665826306056506,
-5.53932232020896));
#51106=CARTESIAN_POINT('Ctrl Pts',(-0.113689589679385,0.69611174793571,
-5.52346480963302));
#51107=CARTESIAN_POINT('Ctrl Pts',(-0.432491505325853,0.557178593751515,
-5.50760729905708));
#51108=CARTESIAN_POINT('Ctrl Pts',(-0.633916371127028,0.298520956886305,
-5.4926583553064));
#51109=CARTESIAN_POINT('Ctrl Pts',(-0.676627951308215,0.0930311431135412,
-5.48299524841438));
#51110=CARTESIAN_POINT('Ctrl Pts',(-0.676720731008515,-1.58587921748089E-5,
-5.47861797838101));
#51111=CARTESIAN_POINT('Ctrl Pts',(-0.676733793626987,-1.34876458775003E-5,
-5.639182021619));
#51112=CARTESIAN_POINT('Ctrl Pts',(-0.676747142672881,-0.0148627663377926,
-5.63848341846471));
#51113=CARTESIAN_POINT('Ctrl Pts',(-0.672645515489534,-0.142058689415187,
-5.63249897845178));
#51114=CARTESIAN_POINT('Ctrl Pts',(-0.596087294840688,-0.377063422523974,
-5.6212287015802));
#51115=CARTESIAN_POINT('Ctrl Pts',(-0.343464771761306,-0.61605911690008,
-5.60537119100425));
#51116=CARTESIAN_POINT('Ctrl Pts',(-0.00734900831199806,-0.705296305700142,
-5.58951368042832));
#51117=CARTESIAN_POINT('Ctrl Pts',(0.330553234139647,-0.623082213877371,
-5.57365616985237));
#51118=CARTESIAN_POINT('Ctrl Pts',(0.588100915954884,-0.389402361121922,
-5.55779865927643));
#51119=CARTESIAN_POINT('Ctrl Pts',(0.70268647930235,-0.0610622463428964,
-5.54194114870048));
#51120=CARTESIAN_POINT('Ctrl Pts',(0.646455189560342,0.282121558884655,
-5.52608363812454));
#51121=CARTESIAN_POINT('Ctrl Pts',(0.433076374763486,0.556724114585172,
-5.5102261275486));
#51122=CARTESIAN_POINT('Ctrl Pts',(0.114420532934634,0.695991973912722,
-5.49436861697265));
#51123=CARTESIAN_POINT('Ctrl Pts',(-0.232049925986955,0.666070355123448,
-5.47851110639671));
#51124=CARTESIAN_POINT('Ctrl Pts',(-0.522111105272023,0.47423293840623,
-5.46265359582076));
#51125=CARTESIAN_POINT('Ctrl Pts',(-0.656982431274472,0.22033182852696,
-5.44954390089486));
#51126=CARTESIAN_POINT('Ctrl Pts',(-0.676648516795683,0.0539702744914142,
-5.4417200428276));
#51127=CARTESIAN_POINT('Ctrl Pts',(-0.676642766387654,2.06514063443713E-6,
-5.439182021619));
#51128=CARTESIAN_POINT('Origin',(1.87869726832665E-16,-4.25270154953079E-17,
-0.0711000000000004));
#51129=CARTESIAN_POINT('',(0.533647856309002,-0.584002718706691,-0.0711000000000004));
#51130=CARTESIAN_POINT('Ctrl Pts',(-0.657933807534666,-0.158364149874852,
-0.0710999999999999));
#51131=CARTESIAN_POINT('Ctrl Pts',(-0.655067175170568,-0.176843370863458,
-0.0711));
#51132=CARTESIAN_POINT('Ctrl Pts',(-0.651433858321437,-0.195176279166223,
-0.0711000000000002));
#51133=CARTESIAN_POINT('Ctrl Pts',(-0.647039750703694,-0.213314001327678,
-0.0711000000000001));
#51134=CARTESIAN_POINT('Ctrl Pts',(-0.640230933967416,-0.241419008522359,
-0.0711));
#51135=CARTESIAN_POINT('Ctrl Pts',(-0.63159703034734,-0.269055704981072,
-0.0711000000000006));
#51136=CARTESIAN_POINT('Ctrl Pts',(-0.621244545257689,-0.296079436761064,
-0.0711000000000008));
#51137=CARTESIAN_POINT('Ctrl Pts',(-0.617380417573146,-0.306166208121415,
-0.0711000000000009));
#51138=CARTESIAN_POINT('Ctrl Pts',(-0.613276543861295,-0.316167552672532,
-0.0710999999999993));
#51139=CARTESIAN_POINT('Ctrl Pts',(-0.608937382020534,-0.32607575008205,
-0.0710999999999992));
#51140=CARTESIAN_POINT('Ctrl Pts',(-0.605509041370034,-0.333904145795049,
-0.0710999999999991));
#51141=CARTESIAN_POINT('Ctrl Pts',(-0.601935083523056,-0.341671178642489,
-0.0710999999999995));
#51142=CARTESIAN_POINT('Ctrl Pts',(-0.598222557587975,-0.349364132086584,
-0.0710999999999997));
#51143=CARTESIAN_POINT('Ctrl Pts',(-0.583545036283053,-0.37977832717853,
-0.0711000000000002));
#51144=CARTESIAN_POINT('Ctrl Pts',(-0.566687660332639,-0.409077303745793,
-0.0711000000000005));
#51145=CARTESIAN_POINT('Ctrl Pts',(-0.547808142714083,-0.437035513090251,
-0.0711000000000012));
#51146=CARTESIAN_POINT('Ctrl Pts',(-0.540578555953244,-0.447741628798144,
-0.0711000000000015));
#51147=CARTESIAN_POINT('Ctrl Pts',(-0.533051911273803,-0.458251009655921,
-0.0711000000000012));
#51148=CARTESIAN_POINT('Ctrl Pts',(-0.525235161508019,-0.468550294116621,
-0.0711000000000016));
#51149=CARTESIAN_POINT('Ctrl Pts',(-0.520149637961148,-0.475250937633454,
-0.0711000000000018));
#51150=CARTESIAN_POINT('Ctrl Pts',(-0.514940349991532,-0.481863803139074,
-0.0711000000000006));
#51151=CARTESIAN_POINT('Ctrl Pts',(-0.50961195342397,-0.488381464082369,
-0.0711000000000006));
#51152=CARTESIAN_POINT('Ctrl Pts',(-0.50174268945366,-0.498007097944534,
-0.0711000000000006));
#51153=CARTESIAN_POINT('Ctrl Pts',(-0.493626185487008,-0.507409974947679,
-0.0711000000000007));
#51154=CARTESIAN_POINT('Ctrl Pts',(-0.485270890711584,-0.516579714254148,
-0.0711000000000008));
#51155=CARTESIAN_POINT('Ctrl Pts',(-0.462359319831774,-0.541724623885286,
-0.0711000000000012));
#51156=CARTESIAN_POINT('Ctrl Pts',(-0.437655716777344,-0.565118419515218,
-0.0711000000000013));
#51157=CARTESIAN_POINT('Ctrl Pts',(-0.411418393873527,-0.586660131434357,
-0.0711000000000024));
#51158=CARTESIAN_POINT('Ctrl Pts',(-0.384942907216212,-0.608397383690681,
-0.0711000000000035));
#51159=CARTESIAN_POINT('Ctrl Pts',(-0.356904820962166,-0.628249603900737,
-0.0711));
#51160=CARTESIAN_POINT('Ctrl Pts',(-0.327527570258942,-0.646080286484725,
-0.0710999999999997));
#51161=CARTESIAN_POINT('Ctrl Pts',(-0.318239054031453,-0.651718002083155,
-0.0710999999999996));
#51162=CARTESIAN_POINT('Ctrl Pts',(-0.308816404956276,-0.657153329266888,
-0.0711000000000009));
#51163=CARTESIAN_POINT('Ctrl Pts',(-0.299266053289952,-0.662381069497827,
-0.0711000000000009));
#51164=CARTESIAN_POINT('Ctrl Pts',(-0.29268155396986,-0.665985340125641,
-0.0711000000000009));
#51165=CARTESIAN_POINT('Ctrl Pts',(-0.286043387081773,-0.66948701230259,
-0.0711000000000016));
#51166=CARTESIAN_POINT('Ctrl Pts',(-0.279358582158395,-0.672882728805687,
-0.0711000000000016));
#51167=CARTESIAN_POINT('Ctrl Pts',(-0.249273658782167,-0.688165130008715,
-0.0711000000000017));
#51168=CARTESIAN_POINT('Ctrl Pts',(-0.218218521949027,-0.701319368658359,
-0.0711000000000021));
#51169=CARTESIAN_POINT('Ctrl Pts',(-0.186415735009314,-0.712239574350195,
-0.0711000000000015));
#51170=CARTESIAN_POINT('Ctrl Pts',(-0.156944284161696,-0.722359263102722,
-0.071100000000001));
#51171=CARTESIAN_POINT('Ctrl Pts',(-0.12682988518337,-0.730560652357132,
-0.0711000000000014));
#51172=CARTESIAN_POINT('Ctrl Pts',(-0.0962629225125643,-0.736850720931549,
-0.0711000000000013));
#51173=CARTESIAN_POINT('Ctrl Pts',(-0.078716983307866,-0.74046132372479,
-0.0711000000000012));
#51174=CARTESIAN_POINT('Ctrl Pts',(-0.0610216276845667,-0.743441599523475,
-0.0711000000000011));
#51175=CARTESIAN_POINT('Ctrl Pts',(-0.0432113397414346,-0.745788198486428,
-0.0711000000000013));
#51176=CARTESIAN_POINT('Ctrl Pts',(-0.0322456473157928,-0.747232986047204,
-0.0711000000000014));
#51177=CARTESIAN_POINT('Ctrl Pts',(-0.0212297038631688,-0.748437831918465,
-0.0711000000000008));
#51178=CARTESIAN_POINT('Ctrl Pts',(-0.0102078164611569,-0.749398841582625,
-0.0711000000000007));
#51179=CARTESIAN_POINT('Ctrl Pts',(0.0255783266149804,-0.752519072091687,
-0.0711000000000004));
#51180=CARTESIAN_POINT('Ctrl Pts',(0.0614807257563876,-0.753082924998665,
-0.0711000000000016));
#51181=CARTESIAN_POINT('Ctrl Pts',(0.0972146459662916,-0.751115790681787,
-0.0711000000000007));
#51182=CARTESIAN_POINT('Ctrl Pts',(0.126022429919159,-0.749529936678811,
-0.0711000000000001));
#51183=CARTESIAN_POINT('Ctrl Pts',(0.154721556272749,-0.746298281511085,
-0.0710999999999997));
#51184=CARTESIAN_POINT('Ctrl Pts',(0.183168524859653,-0.741410164954474,
-0.0710999999999994));
#51185=CARTESIAN_POINT('Ctrl Pts',(0.199846793288582,-0.738544294737266,
-0.0710999999999992));
#51186=CARTESIAN_POINT('Ctrl Pts',(0.216438437569116,-0.73510861830928,
-0.0710999999999984));
#51187=CARTESIAN_POINT('Ctrl Pts',(0.232919227747053,-0.731115468971878,
-0.0710999999999985));
#51188=CARTESIAN_POINT('Ctrl Pts',(0.241823558807982,-0.72895802850379,
-0.0710999999999985));
#51189=CARTESIAN_POINT('Ctrl Pts',(0.250695524136604,-0.72663781184377,
-0.0711000000000005));
#51190=CARTESIAN_POINT('Ctrl Pts',(0.25953123057737,-0.724156453648781,
-0.0711000000000006));
#51191=CARTESIAN_POINT('Ctrl Pts',(0.266656117644727,-0.722155550038926,
-0.0711000000000008));
#51192=CARTESIAN_POINT('Ctrl Pts',(0.27375672049831,-0.720049926629994,
-0.0711000000000007));
#51193=CARTESIAN_POINT('Ctrl Pts',(0.280818325570169,-0.717844754206751,
-0.0711000000000006));
#51194=CARTESIAN_POINT('Ctrl Pts',(0.315496365708099,-0.70701562159085,
-0.0711000000000003));
#51195=CARTESIAN_POINT('Ctrl Pts',(0.349314461131609,-0.693768119967408,
-0.0710999999999986));
#51196=CARTESIAN_POINT('Ctrl Pts',(0.382044763390059,-0.678267148964668,
-0.0710999999999989));
#51197=CARTESIAN_POINT('Ctrl Pts',(0.415042655619168,-0.662639448170585,
-0.0710999999999991));
#51198=CARTESIAN_POINT('Ctrl Pts',(0.446936060969254,-0.644720926130431,
-0.0710999999999995));
#51199=CARTESIAN_POINT('Ctrl Pts',(0.477482228286911,-0.624629210095727,
-0.0710999999999994));
#51200=CARTESIAN_POINT('Ctrl Pts',(0.496763176301389,-0.611947182646645,
-0.0710999999999993));
#51201=CARTESIAN_POINT('Ctrl Pts',(0.51550711528861,-0.598398299343742,
-0.0711000000000005));
#51202=CARTESIAN_POINT('Ctrl Pts',(0.533647856309002,-0.584002718706691,
-0.0711000000000004));
#51203=CARTESIAN_POINT('',(-0.7911,-9.68818082805472E-17,-0.0711000000000002));
#51204=CARTESIAN_POINT('Origin',(0.,0.,-0.0711000000000004));
#51205=CARTESIAN_POINT('',(0.789514313045754,0.0505148300805575,-0.0711000000000008));
#51206=CARTESIAN_POINT('Origin',(0.,0.,-0.0711000000000004));
#51207=CARTESIAN_POINT('Ctrl Pts',(0.789514313045754,0.0505148300805575,
-0.0711000000000008));
#51208=CARTESIAN_POINT('Ctrl Pts',(0.786646978061939,0.0720310274345683,
-0.0711000000000009));
#51209=CARTESIAN_POINT('Ctrl Pts',(0.782893056548073,0.0933955551493298,
-0.0711000000000011));
#51210=CARTESIAN_POINT('Ctrl Pts',(0.778246937672325,0.114553731850933,
-0.0711000000000015));
#51211=CARTESIAN_POINT('Ctrl Pts',(0.771351411757343,0.145955587821779,
-0.071100000000002));
#51212=CARTESIAN_POINT('Ctrl Pts',(0.762491759243552,0.176903771447525,
-0.0711000000000021));
#51213=CARTESIAN_POINT('Ctrl Pts',(0.751744397702525,0.207227273368498,
-0.0711000000000022));
#51214=CARTESIAN_POINT('Ctrl Pts',(0.747529533840752,0.219119441685457,
-0.0711000000000022));
#51215=CARTESIAN_POINT('Ctrl Pts',(0.743024048428749,0.2309153715258,-0.0711000000000015));
#51216=CARTESIAN_POINT('Ctrl Pts',(0.738231505771285,0.242604011376074,
-0.0711000000000015));
#51217=CARTESIAN_POINT('Ctrl Pts',(0.734846385381388,0.250860057470042,
-0.0711000000000016));
#51218=CARTESIAN_POINT('Ctrl Pts',(0.731318354610578,0.259061428072549,
-0.0711000000000027));
#51219=CARTESIAN_POINT('Ctrl Pts',(0.727654054345844,0.267193088850121,
-0.0711000000000026));
#51220=CARTESIAN_POINT('Ctrl Pts',(0.712237780878605,0.30140423347065,-0.0711000000000021));
#51221=CARTESIAN_POINT('Ctrl Pts',(0.694391329924917,0.334439112533965,
-0.0711000000000008));
#51222=CARTESIAN_POINT('Ctrl Pts',(0.674232315159198,0.366018489702608,
-0.0711000000000009));
#51223=CARTESIAN_POINT('Ctrl Pts',(0.661954695941359,0.385251551065925,
-0.071100000000001));
#51224=CARTESIAN_POINT('Ctrl Pts',(0.64881830561573,0.403944116210025,-0.0711000000000001));
#51225=CARTESIAN_POINT('Ctrl Pts',(0.634841970653168,0.422025133375404,
-0.0710999999999997));
#51226=CARTESIAN_POINT('Ctrl Pts',(0.629531677098083,0.428894996553405,
-0.0710999999999995));
#51227=CARTESIAN_POINT('Ctrl Pts',(0.624104492788437,0.435670645433795,
-0.0711000000000013));
#51228=CARTESIAN_POINT('Ctrl Pts',(0.618566742729686,0.442342896181215,
-0.0711000000000013));
#51229=CARTESIAN_POINT('Ctrl Pts',(0.614748344734689,0.44694355684769,-0.0711000000000013));
#51230=CARTESIAN_POINT('Ctrl Pts',(0.610876694281843,0.451495942259902,
-0.0711000000000009));
#51231=CARTESIAN_POINT('Ctrl Pts',(0.606952317219739,0.455998969182275,
-0.0711000000000009));
#51232=CARTESIAN_POINT('Ctrl Pts',(0.583540589687488,0.48286275869808,-0.071100000000001));
#51233=CARTESIAN_POINT('Ctrl Pts',(0.558255129692067,0.507973159032313,
-0.0711000000000011));
#51234=CARTESIAN_POINT('Ctrl Pts',(0.531324903596647,0.53118307146707,-0.0711000000000014));
#51235=CARTESIAN_POINT('Ctrl Pts',(0.504630859305665,0.554189429762315,
-0.0711000000000016));
#51236=CARTESIAN_POINT('Ctrl Pts',(0.47631965093766,0.575329052982221,-0.0711000000000001));
#51237=CARTESIAN_POINT('Ctrl Pts',(0.446590446866821,0.59441407859226,-0.0711));
#51238=CARTESIAN_POINT('Ctrl Pts',(0.437640726063256,0.60015946115722,-0.0711));
#51239=CARTESIAN_POINT('Ctrl Pts',(0.428562395620676,0.605718303647675,
-0.0710999999999995));
#51240=CARTESIAN_POINT('Ctrl Pts',(0.419360692132523,0.611084560737194,
-0.0710999999999993));
#51241=CARTESIAN_POINT('Ctrl Pts',(0.413137738253102,0.614713668153683,
-0.0710999999999991));
#51242=CARTESIAN_POINT('Ctrl Pts',(0.406859115394236,0.618254100749264,
-0.0711000000000006));
#51243=CARTESIAN_POINT('Ctrl Pts',(0.400537808541689,0.621698188698112,
-0.0711000000000007));
#51244=CARTESIAN_POINT('Ctrl Pts',(0.369358146635338,0.638686052177249,
-0.0711000000000012));
#51245=CARTESIAN_POINT('Ctrl Pts',(0.337070510684383,0.65337634097395,-0.0711000000000023));
#51246=CARTESIAN_POINT('Ctrl Pts',(0.303891343528074,0.665602796457808,
-0.0711000000000025));
#51247=CARTESIAN_POINT('Ctrl Pts',(0.275872617224997,0.675927640003309,
-0.0711000000000027));
#51248=CARTESIAN_POINT('Ctrl Pts',(0.2472171506619,0.684494612208159,-0.0711000000000028));
#51249=CARTESIAN_POINT('Ctrl Pts',(0.218096358592357,0.691272993639705,
-0.071100000000003));
#51250=CARTESIAN_POINT('Ctrl Pts',(0.202620172922082,0.694875350654172,
-0.0711000000000031));
#51251=CARTESIAN_POINT('Ctrl Pts',(0.187012534642492,0.697972065861056,
-0.0711000000000009));
#51252=CARTESIAN_POINT('Ctrl Pts',(0.171299516949898,0.700555257048155,
-0.071100000000001));
#51253=CARTESIAN_POINT('Ctrl Pts',(0.163746901610617,0.701796893108501,
-0.0711000000000011));
#51254=CARTESIAN_POINT('Ctrl Pts',(0.156169947568287,0.702919853992287,
-0.0711000000000002));
#51255=CARTESIAN_POINT('Ctrl Pts',(0.148571605417996,0.703923076234743,
-0.0711000000000002));
#51256=CARTESIAN_POINT('Ctrl Pts',(0.140949579614127,0.704929425470902,
-0.0711000000000003));
#51257=CARTESIAN_POINT('Ctrl Pts',(0.133314942393103,0.705814064021666,
-0.0711000000000012));
#51258=CARTESIAN_POINT('Ctrl Pts',(0.125675256770885,0.706576348697078,
-0.0711000000000011));
#51259=CARTESIAN_POINT('Ctrl Pts',(0.0918942032621264,0.709947008261146,
-0.0711000000000007));
#51260=CARTESIAN_POINT('Ctrl Pts',(0.0579854030734698,0.710933280173858,
-0.0710999999999987));
#51261=CARTESIAN_POINT('Ctrl Pts',(0.0242035334269883,0.709501173726401,
-0.0710999999999993));
#51262=CARTESIAN_POINT('Ctrl Pts',(-0.000358657995172887,0.70845991481837,
-0.0710999999999997));
#51263=CARTESIAN_POINT('Ctrl Pts',(-0.024853941788823,0.706139122614643,
-0.0711000000000006));
#51264=CARTESIAN_POINT('Ctrl Pts',(-0.0491808006996979,0.702508747012482,
-0.0711000000000007));
#51265=CARTESIAN_POINT('Ctrl Pts',(-0.0650275557039196,0.700143884662125,
-0.0711000000000008));
#51266=CARTESIAN_POINT('Ctrl Pts',(-0.080802759147321,0.697222993781091,
-0.0711000000000019));
#51267=CARTESIAN_POINT('Ctrl Pts',(-0.0964785109981452,0.693753240057663,
-0.0711000000000019));
#51268=CARTESIAN_POINT('Ctrl Pts',(-0.104693255733889,0.691934945062622,
-0.0711000000000019));
#51269=CARTESIAN_POINT('Ctrl Pts',(-0.112880665544142,0.689965885761257,
-0.071100000000001));
#51270=CARTESIAN_POINT('Ctrl Pts',(-0.121036547279302,0.687846867496625,
-0.071100000000001));
#51271=CARTESIAN_POINT('Ctrl Pts',(-0.12712368240448,0.686265340087524,
-0.071100000000001));
#51272=CARTESIAN_POINT('Ctrl Pts',(-0.133191875532908,0.684600545569067,
-0.0711000000000012));
#51273=CARTESIAN_POINT('Ctrl Pts',(-0.139230257177048,0.682855775576718,
-0.0711000000000012));
#51274=CARTESIAN_POINT('Ctrl Pts',(-0.171263564902799,0.673599859443985,
-0.0711000000000012));
#51275=CARTESIAN_POINT('Ctrl Pts',(-0.202532061429895,0.662078717887296,
-0.071100000000002));
#51276=CARTESIAN_POINT('Ctrl Pts',(-0.23280063481128,0.648397909317886,
-0.0711000000000016));
#51277=CARTESIAN_POINT('Ctrl Pts',(-0.262509394373431,0.634970125745688,
-0.0711000000000013));
#51278=CARTESIAN_POINT('Ctrl Pts',(-0.291255846843352,0.619461112155213,
-0.0710999999999998));
#51279=CARTESIAN_POINT('Ctrl Pts',(-0.318789308023056,0.601930587013271,
-0.0710999999999998));
#51280=CARTESIAN_POINT('Ctrl Pts',(-0.334282722599328,0.592065946603873,
-0.0710999999999997));
#51281=CARTESIAN_POINT('Ctrl Pts',(-0.349391454463959,0.581560537742664,
-0.0711000000000004));
#51282=CARTESIAN_POINT('Ctrl Pts',(-0.364065050236216,0.570420484551968,
-0.0711000000000004));
#51283=CARTESIAN_POINT('Ctrl Pts',(-0.292601934307084,0.610169646934156,
-5.87494887079529));
#51284=CARTESIAN_POINT('Ctrl Pts',(-0.393926377869307,0.561580327016552,
-5.86966303393665));
#51285=CARTESIAN_POINT('Ctrl Pts',(-0.571801589437153,0.41300180871426,
-5.85909136021935));
#51286=CARTESIAN_POINT('Ctrl Pts',(-0.699630454730174,0.089520482193593,
-5.84323384964341));
#51287=CARTESIAN_POINT('Ctrl Pts',(-0.65737507433218,-0.255632286976451,
-5.82737633906746));
#51288=CARTESIAN_POINT('Ctrl Pts',(-0.455323085285772,-0.53868739721303,
-5.81151882849152));
#51289=CARTESIAN_POINT('Ctrl Pts',(-0.142583287492297,-0.690769884805212,
-5.79566131791557));
#51290=CARTESIAN_POINT('Ctrl Pts',(0.204815806457288,-0.674943835808658,
-5.77980380733964));
#51291=CARTESIAN_POINT('Ctrl Pts',(0.502426729513632,-0.495039039708356,
-5.76394629676369));
#51292=CARTESIAN_POINT('Ctrl Pts',(0.677901792498161,-0.194797654574707,
-5.74808878618775));
#51293=CARTESIAN_POINT('Ctrl Pts',(0.688585132880224,0.152798855491627,
-5.7322312756118));
#51294=CARTESIAN_POINT('Ctrl Pts',(0.531879433776216,0.463250529001845,
-5.71637376503586));
#51295=CARTESIAN_POINT('Ctrl Pts',(0.245878610535506,0.661090510301056,
-5.70051625445991));
#51296=CARTESIAN_POINT('Ctrl Pts',(-0.0998931488246837,0.698225042897434,
-5.68465874388397));
#51297=CARTESIAN_POINT('Ctrl Pts',(-0.421381756118886,0.565627364000294,
-5.66880123330803));
#51298=CARTESIAN_POINT('Ctrl Pts',(-0.640436201277647,0.295530633571676,
-5.65294372273209));
#51299=CARTESIAN_POINT('Ctrl Pts',(-0.70380628058059,-0.0464069459234262,
-5.63708621215614));
#51300=CARTESIAN_POINT('Ctrl Pts',(-0.596087294840688,-0.377063422523974,
-5.6212287015802));
#51301=CARTESIAN_POINT('Ctrl Pts',(-0.343464771761306,-0.61605911690008,
-5.60537119100425));
#51302=CARTESIAN_POINT('Ctrl Pts',(-0.00734900831199806,-0.705296305700142,
-5.58951368042832));
#51303=CARTESIAN_POINT('Ctrl Pts',(0.330553234139647,-0.623082213877371,
-5.57365616985237));
#51304=CARTESIAN_POINT('Ctrl Pts',(0.588100915954884,-0.389402361121922,
-5.55779865927643));
#51305=CARTESIAN_POINT('Ctrl Pts',(0.70268647930235,-0.0610622463428964,
-5.54194114870048));
#51306=CARTESIAN_POINT('Ctrl Pts',(0.646455189560342,0.282121558884655,
-5.52608363812454));
#51307=CARTESIAN_POINT('Ctrl Pts',(0.433076374763486,0.556724114585172,
-5.5102261275486));
#51308=CARTESIAN_POINT('Ctrl Pts',(0.114420532934634,0.695991973912722,
-5.49436861697265));
#51309=CARTESIAN_POINT('Ctrl Pts',(-0.232049925986955,0.666070355123448,
-5.47851110639671));
#51310=CARTESIAN_POINT('Ctrl Pts',(-0.522111105272023,0.47423293840623,
-5.46265359582076));
#51311=CARTESIAN_POINT('Ctrl Pts',(-0.685251703933044,0.167113698949432,
-5.44679608524482));
#51312=CARTESIAN_POINT('Ctrl Pts',(-0.681813688851661,-0.180629399086395,
-5.43093857466888));
#51313=CARTESIAN_POINT('Ctrl Pts',(-0.512632811011637,-0.484463091673161,
-5.41508106409294));
#51314=CARTESIAN_POINT('Ctrl Pts',(-0.218835441848411,-0.670528101954526,
-5.39922355351699));
#51315=CARTESIAN_POINT('Ctrl Pts',(0.128158883019949,-0.693593675592924,
-5.38336604294105));
#51316=CARTESIAN_POINT('Ctrl Pts',(0.443998919690547,-0.548052776138566,
-5.3675085323651));
#51317=CARTESIAN_POINT('Ctrl Pts',(0.651906755505725,-0.269285105873896,
-5.35165102178917));
#51318=CARTESIAN_POINT('Ctrl Pts',(0.701341838902262,0.0749433861305649,
-5.33579351121321));
#51319=CARTESIAN_POINT('Ctrl Pts',(0.580286939400919,0.400953805419331,
-5.31993600063728));
#51320=CARTESIAN_POINT('Ctrl Pts',(0.31816942979039,0.62949590949138,-5.30407849006133));
#51321=CARTESIAN_POINT('Ctrl Pts',(-0.0212922472927337,0.705013139114975,
-5.28822097948539));
#51322=CARTESIAN_POINT('Ctrl Pts',(-0.355577967837347,0.609147925308939,
-5.27236346890944));
#51323=CARTESIAN_POINT('Ctrl Pts',(-0.603425836976519,0.365204251602734,
-5.2565059583335));
#51324=CARTESIAN_POINT('Ctrl Pts',(-0.704586235156745,0.0324826622549327,
-5.24064844775756));
#51325=CARTESIAN_POINT('Ctrl Pts',(-0.634467966474636,-0.30813517429379,
-5.22479093718161));
#51326=CARTESIAN_POINT('Ctrl Pts',(-0.410116160373992,-0.573848081916823,
-5.20893342660567));
#51327=CARTESIAN_POINT('Ctrl Pts',(-0.0860687518011682,-0.700063608597757,
-5.19307591602972));
#51328=CARTESIAN_POINT('Ctrl Pts',(0.25890120724375,-0.656099878834963,
-5.17721840545379));
#51329=CARTESIAN_POINT('Ctrl Pts',(0.540934578241509,-0.452644085548684,
-5.16136089487784));
#51330=CARTESIAN_POINT('Ctrl Pts',(0.691471549227516,-0.139154528235421,
-5.1455033843019));
#51331=CARTESIAN_POINT('Ctrl Pts',(0.673917917224984,0.208162261139392,
-5.12964587372595));
#51332=CARTESIAN_POINT('Ctrl Pts',(0.492540814542161,0.504876650410443,
-5.11378836315001));
#51333=CARTESIAN_POINT('Ctrl Pts',(0.191431406740854,0.678860002233702,
-5.09793085257407));
#51334=CARTESIAN_POINT('Ctrl Pts',(-0.156213278796698,0.687818506327875,
-5.08207334199812));
#51335=CARTESIAN_POINT('Ctrl Pts',(-0.465883901255171,0.529574429774311,
-5.06621583142218));
#51336=CARTESIAN_POINT('Ctrl Pts',(-0.662302277873419,0.242595504581606,
-5.05035832084624));
#51337=CARTESIAN_POINT('Ctrl Pts',(-0.697720842752782,-0.103356236908438,
-5.03450081027029));
#51338=CARTESIAN_POINT('Ctrl Pts',(-0.563529656794226,-0.424182993568702,
-5.01864329969435));
#51339=CARTESIAN_POINT('Ctrl Pts',(-0.292349407557091,-0.641894625324549,
-5.00278578911841));
#51340=CARTESIAN_POINT('Ctrl Pts',(0.0498983906696054,-0.703567364740653,
-4.98692827854246));
#51341=CARTESIAN_POINT('Ctrl Pts',(0.380016332526679,-0.594209115659208,
-4.97107076796653));
#51342=CARTESIAN_POINT('Ctrl Pts',(0.617755673194353,-0.340403898855044,
-4.95521325739056));
#51343=CARTESIAN_POINT('Ctrl Pts',(0.705324086767725,-0.00384951228082019,
-4.93935574681464));
#51344=CARTESIAN_POINT('Ctrl Pts',(0.621434468293966,0.333640656598862,
-4.92349823623868));
#51345=CARTESIAN_POINT('Ctrl Pts',(0.386479640253609,0.590025739937645,
-4.90764072566275));
#51346=CARTESIAN_POINT('Ctrl Pts',(0.0575750382195188,0.702980797101559,
-4.8917832150868));
#51347=CARTESIAN_POINT('Ctrl Pts',(-0.285325545141958,0.645047455160447,
-4.87592570451086));
#51348=CARTESIAN_POINT('Ctrl Pts',(-0.558866018193005,0.430308795899666,
-4.86006819393491));
#51349=CARTESIAN_POINT('Ctrl Pts',(-0.696551117161325,0.110965883499543,
-4.84421068335897));
#51350=CARTESIAN_POINT('Ctrl Pts',(-0.664910815212153,-0.23535185134907,
-4.82835317278303));
#51351=CARTESIAN_POINT('Ctrl Pts',(-0.471636589224496,-0.524457637778504,
-4.81249566220709));
#51352=CARTESIAN_POINT('Ctrl Pts',(-0.163711689954952,-0.686072422337189,
-4.79663815163114));
#51353=CARTESIAN_POINT('Ctrl Pts',(0.184010069664874,-0.680909083785385,
-4.7807806410552));
#51354=CARTESIAN_POINT('Ctrl Pts',(0.487000612793599,-0.510222783946564,
-4.76492313047925));
#51355=CARTESIAN_POINT('Ctrl Pts',(0.671605624729155,-0.215505848996464,
-4.74906561990332));
#51356=CARTESIAN_POINT('Ctrl Pts',(0.692949263789228,0.131598647156757,
-4.73320810932736));
#51357=CARTESIAN_POINT('Ctrl Pts',(0.545843080552321,0.446712678947753,
-4.71735059875143));
#51358=CARTESIAN_POINT('Ctrl Pts',(0.266047283910979,0.653234819068239,
-4.70149308817548));
#51359=CARTESIAN_POINT('Ctrl Pts',(-0.0784222486577756,0.700961366292738,
-4.68563557759954));
#51360=CARTESIAN_POINT('Ctrl Pts',(-0.403828027874236,0.578290420137434,
-4.66977806702359));
#51361=CARTESIAN_POINT('Ctrl Pts',(-0.631066793878241,0.315042200004637,
-4.65392055644765));
#51362=CARTESIAN_POINT('Ctrl Pts',(-0.704898817366892,-0.0247899857660444,
-4.6380630458717));
#51363=CARTESIAN_POINT('Ctrl Pts',(-0.607376188029295,-0.358595945786518,
-4.62220553529577));
#51364=CARTESIAN_POINT('Ctrl Pts',(-0.362205792415875,-0.605230410719679,
-4.60634802471981));
#51365=CARTESIAN_POINT('Ctrl Pts',(-0.0289863800046666,-0.704738728816396,
-4.59049051414388));
#51366=CARTESIAN_POINT('Ctrl Pts',(0.311279364390673,-0.632931310194133,
-4.57463300356793));
#51367=CARTESIAN_POINT('Ctrl Pts',(0.575875855124356,-0.407263901671038,
-4.55877549299199));
#51368=CARTESIAN_POINT('Ctrl Pts',(0.700482031227543,-0.0825942494781502,
-4.54291798241604));
#51369=CARTESIAN_POINT('Ctrl Pts',(0.654807236055464,0.262153332477254,
-4.5270604718401));
#51370=CARTESIAN_POINT('Ctrl Pts',(0.449954607358944,0.543173763574772,
-4.51120296126416));
#51371=CARTESIAN_POINT('Ctrl Pts',(0.13572200293829,0.692153468558775,-4.49534545068821));
#51372=CARTESIAN_POINT('Ctrl Pts',(-0.211503417077158,0.672876802010746,
-4.47948794011228));
#51373=CARTESIAN_POINT('Ctrl Pts',(-0.507314231603265,0.49002975066042,
-4.46363042953633));
#51374=CARTESIAN_POINT('Ctrl Pts',(-0.679801454305346,0.188060811558017,
-4.44777291896038));
#51375=CARTESIAN_POINT('Ctrl Pts',(-0.687034970626699,-0.159624043475585,
-4.43191540838445));
#51376=CARTESIAN_POINT('Ctrl Pts',(-0.527256376882394,-0.468505708776717,
-4.41605789780849));
#51377=CARTESIAN_POINT('Ctrl Pts',(-0.239306432604977,-0.663497790074244,
-4.40020038723256));
#51378=CARTESIAN_POINT('Ctrl Pts',(0.106816783733375,-0.697199441216343,
-4.38434287665661));
#51379=CARTESIAN_POINT('Ctrl Pts',(0.426973786990221,-0.561418089611258,
-4.36848536608067));
#51380=CARTESIAN_POINT('Ctrl Pts',(0.64333724820522,-0.289160977988487,
-4.35262785550472));
#51381=CARTESIAN_POINT('Ctrl Pts',(0.703311128248571,0.0533886036645251,
-4.33677034492878));
#51382=CARTESIAN_POINT('Ctrl Pts',(0.592316308613785,0.382959889113288,
-4.32091283435284));
#51383=CARTESIAN_POINT('Ctrl Pts',(0.337334645867288,0.619437020864201,
-4.3050553237769));
#51384=CARTESIAN_POINT('Ctrl Pts',(0.000349921539867571,0.7053345048092,
-4.28919781320095));
#51385=CARTESIAN_POINT('Ctrl Pts',(-0.336719865611468,0.619771424173557,
-4.27334030262501));
#51386=CARTESIAN_POINT('Ctrl Pts',(-0.591936038811396,0.383547405252334,
-4.25748279204906));
#51387=CARTESIAN_POINT('Ctrl Pts',(-0.70325780911707,0.0540864126688136,
-4.24162528147312));
#51388=CARTESIAN_POINT('Ctrl Pts',(-0.643623841152751,-0.288522507301082,
-4.22576777089717));
#51389=CARTESIAN_POINT('Ctrl Pts',(-0.427530623812185,-0.560994163804123,
-4.20991026032124));
#51390=CARTESIAN_POINT('Ctrl Pts',(-0.107508502335302,-0.697093112894644,
-4.19405274974529));
#51391=CARTESIAN_POINT('Ctrl Pts',(0.238647982882395,-0.663734906710268,
-4.17819523916935));
#51392=CARTESIAN_POINT('Ctrl Pts',(0.526791259328862,-0.469028629418541,
-4.1623377285934));
#51393=CARTESIAN_POINT('Ctrl Pts',(0.68687625119572,-0.160305650751426,
-4.14648021801746));
#51394=CARTESIAN_POINT('Ctrl Pts',(0.679987716283376,0.187386210333744,
-4.13062270744152));
#51395=CARTESIAN_POINT('Ctrl Pts',(0.507800196354854,0.489526145064282,
-4.11476519686557));
#51396=CARTESIAN_POINT('Ctrl Pts',(0.212170950879785,0.672666614098168,
-4.09890768628963));
#51397=CARTESIAN_POINT('Ctrl Pts',(-0.135035171633647,0.692287793147759,
-4.08305017571368));
#51398=CARTESIAN_POINT('Ctrl Pts',(-0.449415441152957,0.543619947548669,
-4.06719266513775));
#51399=CARTESIAN_POINT('Ctrl Pts',(-0.654546801472525,0.262802912467901,
-4.0513351545618));
#51400=CARTESIAN_POINT('Ctrl Pts',(-0.700563637605738,-0.0818991806072614,
-4.03547764398586));
#51401=CARTESIAN_POINT('Ctrl Pts',(-0.576279664676672,-0.406692308999895,
-4.01962013340991));
#51402=CARTESIAN_POINT('Ctrl Pts',(-0.311907214595146,-0.632622142833319,
-4.00376262283397));
#51403=CARTESIAN_POINT('Ctrl Pts',(0.0282871139661857,-0.70476714261023,
-3.98790511225803));
#51404=CARTESIAN_POINT('Ctrl Pts',(0.361605095917608,-0.6055894985268,-3.97204760168208));
#51405=CARTESIAN_POINT('Ctrl Pts',(0.607020085064156,-0.35919841654471,
-3.95619009110614));
#51406=CARTESIAN_POINT('Ctrl Pts',(0.704873873408482,-0.0254893841755349,
-3.9403325805302));
#51407=CARTESIAN_POINT('Ctrl Pts',(0.631379072581692,0.31441589149629,-3.92447506995425));
#51408=CARTESIAN_POINT('Ctrl Pts',(0.40440161705542,0.57788945157572,-3.90861755937831));
#51409=CARTESIAN_POINT('Ctrl Pts',(0.0791177138722245,0.700883209579997,
-3.89276004880237));
#51410=CARTESIAN_POINT('Ctrl Pts',(-0.265399004090862,0.653498473408395,
-3.87690253822642));
#51411=CARTESIAN_POINT('Ctrl Pts',(-0.545399577203117,0.447254052308289,
-3.86104502765048));
#51412=CARTESIAN_POINT('Ctrl Pts',(-0.692818348643004,0.132286136473575,
-3.84518751707454));
#51413=CARTESIAN_POINT('Ctrl Pts',(-0.67181912209725,-0.214839366280961,
-3.82933000649859));
#51414=CARTESIAN_POINT('Ctrl Pts',(-0.487506623358711,-0.50973932387144,
-3.81347249592265));
#51415=CARTESIAN_POINT('Ctrl Pts',(-0.184685586744943,-0.680726171208512,
-3.79761498534671));
#51416=CARTESIAN_POINT('Ctrl Pts',(0.163030878572916,-0.686234521684292,
-3.78175747477076));
#51417=CARTESIAN_POINT('Ctrl Pts',(0.471115982751349,-0.524925344135482,
-3.76589996419482));
#51418=CARTESIAN_POINT('Ctrl Pts',(0.664676968465788,-0.236011469447257,
-3.75004245361887));
#51419=CARTESIAN_POINT('Ctrl Pts',(0.696660876212486,0.110274700971604,
-3.73418494304293));
#51420=CARTESIAN_POINT('Ctrl Pts',(0.559292701589483,0.429754069286446,
-3.71832743246699));
#51421=CARTESIAN_POINT('Ctrl Pts',(0.285965429933078,0.644764033583383,
-3.70246992189105));
#51422=CARTESIAN_POINT('Ctrl Pts',(-0.0568775023532221,0.703037577833207,
-3.6866124113151));
#51423=CARTESIAN_POINT('Ctrl Pts',(-0.385894018096841,0.590408920085563,
-3.67075490073916));
#51424=CARTESIAN_POINT('Ctrl Pts',(-0.621103119400875,0.334257088466388,
-3.65489739016321));
#51425=CARTESIAN_POINT('Ctrl Pts',(-0.70532755911646,-0.00314967781535797,
-3.63903987958727));
#51426=CARTESIAN_POINT('Ctrl Pts',(-0.618093122687726,-0.339790785345425,
-3.62318236901133));
#51427=CARTESIAN_POINT('Ctrl Pts',(-0.380605728184695,-0.593831765563718,
-3.60732485843538));
#51428=CARTESIAN_POINT('Ctrl Pts',(-0.0505964556334205,-0.703517508521898,
-3.59146734785944));
#51429=CARTESIAN_POINT('Ctrl Pts',(0.291712366691096,-0.642184382587279,
-3.5756098372835));
#51430=CARTESIAN_POINT('Ctrl Pts',(0.563108499012531,-0.424741926891352,
-3.55975232670755));
#51431=CARTESIAN_POINT('Ctrl Pts',(0.697617947778104,-0.104048474555806,
-3.54389481613161));
#51432=CARTESIAN_POINT('Ctrl Pts',(0.66254265856183,0.241938239444174,-3.52803730555567));
#51433=CARTESIAN_POINT('Ctrl Pts',(0.466409123192545,0.529111912474371,
-3.51217979497972));
#51434=CARTESIAN_POINT('Ctrl Pts',(0.156895665186708,0.687663170720335,
-3.49632228440378));
#51435=CARTESIAN_POINT('Ctrl Pts',(-0.19075773797954,0.679049609027539,
-3.48046477382783));
#51436=CARTESIAN_POINT('Ctrl Pts',(-0.492039626312628,0.505365107875141,
-3.4646072632519));
#51437=CARTESIAN_POINT('Ctrl Pts',(-0.67371104394227,0.208830829595975,
-3.44874975267595));
#51438=CARTESIAN_POINT('Ctrl Pts',(-0.691609279952494,-0.138468371851177,
-3.43289224210001));
#51439=CARTESIAN_POINT('Ctrl Pts',(-0.541383431856071,-0.452107139770282,
-3.41703473152406));
#51440=CARTESIAN_POINT('Ctrl Pts',(-0.259552071413764,-0.655842670420542,
-3.40117722094812));
#51441=CARTESIAN_POINT('Ctrl Pts',(0.0853740963848333,-0.700148662632442,
-3.38531971037218));
#51442=CARTESIAN_POINT('Ctrl Pts',(0.409546578284193,-0.574254722518878,
-3.36946219979623));
#51443=CARTESIAN_POINT('Ctrl Pts',(0.634161918067455,-0.308764550738151,
-3.35360468922029));
#51444=CARTESIAN_POINT('Ctrl Pts',(0.70461811808652,0.0317835458017981,
-3.33774717864434));
#51445=CARTESIAN_POINT('Ctrl Pts',(0.603787900785698,0.364605344152174,
-3.32188966806841));
#51446=CARTESIAN_POINT('Ctrl Pts',(0.356182198023997,0.608794815952237,
-3.30603215749246));
#51447=CARTESIAN_POINT('Ctrl Pts',(0.021991760855621,0.704991665606051,
-3.29017464691652));
#51448=CARTESIAN_POINT('Ctrl Pts',(-0.317544678396473,0.629811291849872,
-3.27431713634057));
#51449=CARTESIAN_POINT('Ctrl Pts',(-0.579888821700749,0.401529376990078,
-3.25845962576463));
#51450=CARTESIAN_POINT('Ctrl Pts',(-0.701267133779017,0.0756392305677909,
-3.24260211518869));
#51451=CARTESIAN_POINT('Ctrl Pts',(-0.652173623112518,-0.268638142183524,
-3.22674460461274));
#51452=CARTESIAN_POINT('Ctrl Pts',(-0.44454248687824,-0.547611964332075,
-3.2108870940368));
#51453=CARTESIAN_POINT('Ctrl Pts',(-0.128847013424495,-0.693466173112368,
-3.19502958346085));
#51454=CARTESIAN_POINT('Ctrl Pts',(0.218170026627314,-0.670744903522167,
-3.17917207288491));
#51455=CARTESIAN_POINT('Ctrl Pts',(0.512151867514703,-0.484971494750699,
-3.16331456230897));
#51456=CARTESIAN_POINT('Ctrl Pts',(0.681634130178766,-0.181305815392006,
-3.14745705173302));
#51457=CARTESIAN_POINT('Ctrl Pts',(0.68541717920589,0.166433700220129,-3.13159954115708));
#51458=CARTESIAN_POINT('Ctrl Pts',(0.522581388918324,0.473714658920027,
-3.11574203058114));
#51459=CARTESIAN_POINT('Ctrl Pts',(0.232710696222986,0.665839784019352,
-3.0998845200052));
#51460=CARTESIAN_POINT('Ctrl Pts',(-0.113729903497026,0.696105160999459,
-3.08402700942925));
#51461=CARTESIAN_POINT('Ctrl Pts',(-0.432523772013128,0.557153545051146,
-3.0681694988533));
#51462=CARTESIAN_POINT('Ctrl Pts',(-0.646174946334819,0.282762842058002,
-3.05231198827737));
#51463=CARTESIAN_POINT('Ctrl Pts',(-0.702746720228755,-0.0603650008469461,
-3.03645447770142));
#51464=CARTESIAN_POINT('Ctrl Pts',(-0.588486997030099,-0.388818647245757,
-3.02059696712548));
#51465=CARTESIAN_POINT('Ctrl Pts',(-0.331171302414811,-0.62275392778882,
-3.00473945654953));
#51466=CARTESIAN_POINT('Ctrl Pts',(0.00664919963267667,-0.70530324986049,
-2.98888194597359));
#51467=CARTESIAN_POINT('Ctrl Pts',(0.342853340201669,-0.61639960515244,
-2.97302443539765));
#51468=CARTESIAN_POINT('Ctrl Pts',(0.595712873526129,-0.377654681468092,
-2.9571669248217));
#51469=CARTESIAN_POINT('Ctrl Pts',(0.703759888922834,-0.0471052530281482,
-2.94130941424576));
#51470=CARTESIAN_POINT('Ctrl Pts',(0.640729114900228,0.29489504478491,-2.92545190366982));
#51471=CARTESIAN_POINT('Ctrl Pts',(0.421942773788548,0.565208971768099,
-2.90959439309387));
#51472=CARTESIAN_POINT('Ctrl Pts',(0.100585885339081,0.698125608891462,
-2.89373688251793));
#51473=CARTESIAN_POINT('Ctrl Pts',(-0.245222540035754,0.661334100117283,
-2.87787937194199));
#51474=CARTESIAN_POINT('Ctrl Pts',(-0.531419540085806,0.463778135032813,
-2.86202186136604));
#51475=CARTESIAN_POINT('Ctrl Pts',(-0.688433161538855,0.153481817206925,
-2.8461643507901));
#51476=CARTESIAN_POINT('Ctrl Pts',(-0.678094785111951,-0.194124569602876,
-2.83030684021415));
#51477=CARTESIAN_POINT('Ctrl Pts',(-0.502917578453797,-0.494540994662418,
-2.81444932963821));
#51478=CARTESIAN_POINT('Ctrl Pts',(-0.205485567371259,-0.674738888549961,
-2.79859181906227));
#51479=CARTESIAN_POINT('Ctrl Pts',(0.141898163291737,-0.690913740906892,
-2.78273430848633));
#51480=CARTESIAN_POINT('Ctrl Pts',(0.454787708536229,-0.539133588532463,
-2.76687679791038));
#51481=CARTESIAN_POINT('Ctrl Pts',(0.657122394010951,-0.256294840776867,
-2.75101928733444));
#51482=CARTESIAN_POINT('Ctrl Pts',(0.69971645158859,0.0888469104459926,
-2.7351617767585));
#51483=CARTESIAN_POINT('Ctrl Pts',(0.572215643513511,0.412390765461524,
-2.71930426618255));
#51484=CARTESIAN_POINT('Ctrl Pts',(0.305614285798879,0.635686081674883,
-2.70344675560661));
#51485=CARTESIAN_POINT('Ctrl Pts',(-0.0352791951986797,0.704451747464407,
-2.68758924503067));
#51486=CARTESIAN_POINT('Ctrl Pts',(-0.367596616630921,0.601971439157228,
-2.67173173445472));
#51487=CARTESIAN_POINT('Ctrl Pts',(-0.610554559694072,0.353157211106192,
-2.65587422387878));
#51488=CARTESIAN_POINT('Ctrl Pts',(-0.705092102509325,0.0184935961484815,
-2.64001671330283));
#51489=CARTESIAN_POINT('Ctrl Pts',(-0.628228006593883,-0.320665648067582,
-2.62415920272689));
#51490=CARTESIAN_POINT('Ctrl Pts',(-0.398647252183052,-0.581873916279484,
-2.60830169215095));
#51491=CARTESIAN_POINT('Ctrl Pts',(-0.072158885197231,-0.701633794373258,
-2.59244418157501));
#51492=CARTESIAN_POINT('Ctrl Pts',(0.271870667014987,-0.650832717782648,
-2.57658667099906));
#51493=CARTESIAN_POINT('Ctrl Pts',(0.549810870497681,-0.441819977821406,
-2.56072916042312));
#51494=CARTESIAN_POINT('Ctrl Pts',(0.694096926018893,-0.125404718454481,
-2.54487164984717));
#51495=CARTESIAN_POINT('Ctrl Pts',(0.669654172730331,0.221495316122894,
-2.52901413927123));
#51496=CARTESIAN_POINT('Ctrl Pts',(0.48242442724551,0.514551803141691,-2.51315662869529));
#51497=CARTESIAN_POINT('Ctrl Pts',(0.17792158070152,0.682525308864219,-2.49729911811934));
#51498=CARTESIAN_POINT('Ctrl Pts',(-0.169832424647492,0.684582963312612,
-2.4814416075434));
#51499=CARTESIAN_POINT('Ctrl Pts',(-0.476301673309269,0.520224568933759,
-2.46558409696745));
#51500=CARTESIAN_POINT('Ctrl Pts',(-0.666986208109069,0.229404194189668,
-2.44972658639152));
#51501=CARTESIAN_POINT('Ctrl Pts',(-0.695532309257702,-0.11718230625044,
-2.43386907581557));
#51502=CARTESIAN_POINT('Ctrl Pts',(-0.555000672657401,-0.435282826986497,
-2.41801156523963));
#51503=CARTESIAN_POINT('Ctrl Pts',(-0.27955329320369,-0.647569951726063,
-2.40215405466368));
#51504=CARTESIAN_POINT('Ctrl Pts',(0.0638510132913964,-0.702438562595467,
-2.38629654408774));
#51505=CARTESIAN_POINT('Ctrl Pts',(0.391733704562298,-0.586550586760786,
-2.3704390335118));
#51506=CARTESIAN_POINT('Ctrl Pts',(0.624389405388874,-0.328077363677613,
-2.35458152293585));
#51507=CARTESIAN_POINT('Ctrl Pts',(0.70526157763973,0.0101485577617963,
-2.33872401235991));
#51508=CARTESIAN_POINT('Ctrl Pts',(0.614690913258262,0.345907454787038,
-2.32286650178397));
#51509=CARTESIAN_POINT('Ctrl Pts',(0.374694337750614,0.59757931639001,-2.30700899120802));
#51510=CARTESIAN_POINT('Ctrl Pts',(0.0436128907985044,0.703984944353017,
-2.29115148063208));
#51511=CARTESIAN_POINT('Ctrl Pts',(-0.298070463232192,0.639258073916999,
-2.27529397005614));
#51512=CARTESIAN_POINT('Ctrl Pts',(-0.567295530361938,0.419133233412588,
-2.25943645948019));
#51513=CARTESIAN_POINT('Ctrl Pts',(-0.698616083737257,0.0971208199262295,
-2.24357894890425));
#51514=CARTESIAN_POINT('Ctrl Pts',(-0.660109261128591,-0.248500803805119,
-2.22772143832831));
#51515=CARTESIAN_POINT('Ctrl Pts',(-0.461135729708285,-0.533714085354632,
-2.21186392775236));
#51516=CARTESIAN_POINT('Ctrl Pts',(-0.150064190853226,-0.689186204695865,
-2.19600641717642));
#51517=CARTESIAN_POINT('Ctrl Pts',(0.197486622320041,-0.677123268042198,
-2.18014890660047));
#51518=CARTESIAN_POINT('Ctrl Pts',(0.497030188535669,-0.500457668343409,
-2.16429139602453));
#51519=CARTESIAN_POINT('Ctrl Pts',(0.675750122618055,-0.20213524655836,
-2.14843388544859));
#51520=CARTESIAN_POINT('Ctrl Pts',(0.690201193133537,0.145324461521679,
-2.13257637487265));
#51521=CARTESIAN_POINT('Ctrl Pts',(0.536870472963871,0.457457081461282,
-2.1167188642967));
#51522=CARTESIAN_POINT('Ctrl Pts',(0.253031300742842,0.65838594073986,-2.10086135372076));
#51523=CARTESIAN_POINT('Ctrl Pts',(-0.0923175372979227,0.699267015114235,
-2.08500384314482));
#51524=CARTESIAN_POINT('Ctrl Pts',(-0.415224800514443,0.57016247785808,
-2.06914633256887));
#51525=CARTESIAN_POINT('Ctrl Pts',(-0.637194596134153,0.302456497329714,
-2.05328882199293));
#51526=CARTESIAN_POINT('Ctrl Pts',(-0.70426803483956,-0.0387739761018672,
-2.03743131141698));
#51527=CARTESIAN_POINT('Ctrl Pts',(-0.600140158358559,-0.370578839715501,
-2.02157380084104));
#51528=CARTESIAN_POINT('Ctrl Pts',(-0.350123530259618,-0.612299272968753,
-2.0057162902651));
#51529=CARTESIAN_POINT('Ctrl Pts',(-0.0149949761710098,-0.705175181645777,
-1.98985877968915));
#51530=CARTESIAN_POINT('Ctrl Pts',(0.323778723678411,-0.626629255790618,
-1.97400126911321));
#51531=CARTESIAN_POINT('Ctrl Pts',(0.583844686443398,-0.395755313585723,
-1.95814375853727));
#51532=CARTESIAN_POINT('Ctrl Pts',(0.701983182336375,-0.0686767634387369,
-1.94228624796132));
#51533=CARTESIAN_POINT('Ctrl Pts',(0.649475790428822,0.275096499007858,
-1.92642873738538));
#51534=CARTESIAN_POINT('Ctrl Pts',(0.439086592159748,0.551996241567879,
-1.91057122680944));
#51535=CARTESIAN_POINT('Ctrl Pts',(0.121959336304979,0.694710591834882,
-1.89471371623349));
#51536=CARTESIAN_POINT('Ctrl Pts',(-0.224815152906662,0.668546956573044,
-1.87885620565755));
#51537=CARTESIAN_POINT('Ctrl Pts',(-0.516939071671466,0.479865483546136,
-1.86299869508161));
#51538=CARTESIAN_POINT('Ctrl Pts',(-0.68339968532608,0.174532965985627,
-1.84714118450566));
#51539=CARTESIAN_POINT('Ctrl Pts',(-0.683731894540956,-0.173226968186133,
-1.83128367392972));
#51540=CARTESIAN_POINT('Ctrl Pts',(-0.51785494220135,-0.478876962232637,
-1.81542616335378));
#51541=CARTESIAN_POINT('Ctrl Pts',(-0.226092044745908,-0.668116212512566,
-1.79956865277784));
#51542=CARTESIAN_POINT('Ctrl Pts',(0.120631824241489,-0.694942335089534,
-1.78371114220189));
#51543=CARTESIAN_POINT('Ctrl Pts',(0.438031166284854,-0.552834137407103,
-1.76785363162595));
#51544=CARTESIAN_POINT('Ctrl Pts',(0.648949015415239,-0.276336862381976,
-1.75199612105));
#51545=CARTESIAN_POINT('Ctrl Pts',(0.702113112519488,0.0673354538688382,
-1.73613861047406));
#51546=CARTESIAN_POINT('Ctrl Pts',(0.584599736947659,0.394639118284352,
-1.72028109989812));
#51547=CARTESIAN_POINT('Ctrl Pts',(0.324975348420559,0.626009511939285,
-1.70442358932217));
#51548=CARTESIAN_POINT('Ctrl Pts',(-0.0136476660564434,0.705202543480052,
-1.68856607874623));
#51549=CARTESIAN_POINT('Ctrl Pts',(-0.348953053916159,0.612967089069317,
-1.67270856817029));
#51550=CARTESIAN_POINT('Ctrl Pts',(-0.599431048207782,0.371724769909193,
-1.65685105759434));
#51551=CARTESIAN_POINT('Ctrl Pts',(-0.704192669272103,0.0401194549184884,
-1.6409935470184));
#51552=CARTESIAN_POINT('Ctrl Pts',(-0.637771295851261,-0.301238543861383,
-1.62513603644245));
#51553=CARTESIAN_POINT('Ctrl Pts',(-0.416313374927947,-0.569368123427741,
-1.60927852586652));
#51554=CARTESIAN_POINT('Ctrl Pts',(-0.0936533636192634,-0.699089360241109,
-1.59342101529057));
#51555=CARTESIAN_POINT('Ctrl Pts',(0.251772950048864,-0.658868171748504,
-1.57756350471463));
#51556=CARTESIAN_POINT('Ctrl Pts',(0.535995491794349,-0.458481972268986,
-1.56170599413868));
#51557=CARTESIAN_POINT('Ctrl Pts',(0.689922281653143,-0.146642870259839,
-1.54584848356274));
#51558=CARTESIAN_POINT('Ctrl Pts',(0.676135081734832,0.200843813364896,
-1.5299909729868));
#51559=CARTESIAN_POINT('Ctrl Pts',(0.49798543810141,0.49950714665405,-1.51413346241085));
#51560=CARTESIAN_POINT('Ctrl Pts',(0.198779949634609,0.676744721252252,
-1.49827595183491));
#51561=CARTESIAN_POINT('Ctrl Pts',(-0.148747182193283,0.689471654173747,
-1.48241844125896));
#51562=CARTESIAN_POINT('Ctrl Pts',(-0.460115192831522,0.534594140863082,
-1.46656093068302));
#51563=CARTESIAN_POINT('Ctrl Pts',(-0.659633279501605,0.249761531652658,
-1.45070342010708));
#51564=CARTESIAN_POINT('Ctrl Pts',(-0.698800364273488,-0.0957858915016492,
-1.43484590953114));
#51565=CARTESIAN_POINT('Ctrl Pts',(-0.568095276096871,-0.418048613675424,
-1.41898839895519));
#51566=CARTESIAN_POINT('Ctrl Pts',(-0.299291263068257,-0.638687424309053,
-1.40313088837925));
#51567=CARTESIAN_POINT('Ctrl Pts',(0.0422678024777705,-0.704066984734566,
-1.3872733778033));
#51568=CARTESIAN_POINT('Ctrl Pts',(0.373551939990352,-0.598294103471671,
-1.37141586722736));
#51569=CARTESIAN_POINT('Ctrl Pts',(0.614028912825419,-0.347081230166595,
-1.35555835665142));
#51570=CARTESIAN_POINT('Ctrl Pts',(0.705240900970187,-0.0114959870512474,
-1.33970084607548));
#51571=CARTESIAN_POINT('Ctrl Pts',(0.625015078797678,0.326883828592142,
-1.32384333549953));
#51572=CARTESIAN_POINT('Ctrl Pts',(0.392853632391026,0.585801083676619,
-1.30798582492359));
#51573=CARTESIAN_POINT('Ctrl Pts',(0.0651929510142312,0.702315289067225,
-1.29212831434764));
#51574=CARTESIAN_POINT('Ctrl Pts',(-0.27831555874946,0.648102874455513,
-1.2762708037717));
#51575=CARTESIAN_POINT('Ctrl Pts',(-0.554168023743774,0.43634239718304,
-1.26041329319576));
#51576=CARTESIAN_POINT('Ctrl Pts',(-0.69530715545327,0.118510951793518,
-1.24455578261981));
#51577=CARTESIAN_POINT('Ctrl Pts',(-0.667423282307466,-0.228129455251735,
-1.22869827204387));
#51578=CARTESIAN_POINT('Ctrl Pts',(-0.477294726647991,-0.519313614334867,
-1.21284076146793));
#51579=CARTESIAN_POINT('Ctrl Pts',(-0.171140054664367,-0.684257238039178,
-1.19698325089199));
#51580=CARTESIAN_POINT('Ctrl Pts',(0.176617247270067,-0.682863993842307,
-1.18112574031604));
#51581=CARTESIAN_POINT('Ctrl Pts',(0.481440462292368,-0.515472567055936,
-1.1652682297401));
#51582=CARTESIAN_POINT('Ctrl Pts',(0.669229769411713,-0.222774329429288,
-1.14941071916415));
#51583=CARTESIAN_POINT('Ctrl Pts',(0.694335253018772,0.124078372550911,
-1.13355320858821));
#51584=CARTESIAN_POINT('Ctrl Pts',(0.550653992635405,0.440768722250355,
-1.11769569801226));
#51585=CARTESIAN_POINT('Ctrl Pts',(0.273113628774048,0.650312103452947,
-1.10183818743633));
#51586=CARTESIAN_POINT('Ctrl Pts',(-0.0708182368002938,0.701770378012652,
-1.08598067686038));
#51587=CARTESIAN_POINT('Ctrl Pts',(-0.397534816887265,0.582634495616192,
-1.07012316628444));
#51588=CARTESIAN_POINT('Ctrl Pts',(-0.627614207556722,0.321865333008187,
-1.05426565570849));
#51589=CARTESIAN_POINT('Ctrl Pts',(-0.705126148834749,-0.0171464383765556,
-1.03840814513255));
#51590=CARTESIAN_POINT('Ctrl Pts',(-0.61122817502222,-0.35199006261332,
-1.0225506345566));
#51591=CARTESIAN_POINT('Ctrl Pts',(-0.368746051047842,-0.601268023394017,
-1.00669312398066));
#51592=CARTESIAN_POINT('Ctrl Pts',(-0.0366250313885693,-0.704383058566367,
-0.990835613404718));
#51593=CARTESIAN_POINT('Ctrl Pts',(0.304399208681507,-0.636268817304129,
-0.974978102828775));
#51594=CARTESIAN_POINT('Ctrl Pts',(0.571426699942949,-0.413483267753163,
-0.959120592252834));
#51595=CARTESIAN_POINT('Ctrl Pts',(0.699545426752022,-0.0901836017791227,
-0.943263081676888));
#51596=CARTESIAN_POINT('Ctrl Pts',(0.657610862529838,0.25503889821415,-0.927405571100947));
#51597=CARTESIAN_POINT('Ctrl Pts',(0.455816928044417,0.538263703241892,
-0.911548060525));
#51598=CARTESIAN_POINT('Ctrl Pts',(0.14321793965191,0.690641374290149,-0.89569054994906));
#51599=CARTESIAN_POINT('Ctrl Pts',(-0.204196060091041,0.675130250516757,
-0.879833039373114));
#51600=CARTESIAN_POINT('Ctrl Pts',(-0.501971808040508,0.495500948588465,
-0.863975528797173));
#51601=CARTESIAN_POINT('Ctrl Pts',(-0.677722659967801,0.195419759199761,
-0.848118018221228));
#51602=CARTESIAN_POINT('Ctrl Pts',(-0.688725141987106,-0.152166241046976,
-0.832260507645285));
#51603=CARTESIAN_POINT('Ctrl Pts',(-0.532304648268198,-0.462761977210308,
-0.816402997069341));
#51604=CARTESIAN_POINT('Ctrl Pts',(-0.246485614000569,-0.660864379589555,
-0.800545486493398));
#51605=CARTESIAN_POINT('Ctrl Pts',(0.0992518876742048,-0.698316510554226,
-0.784687975917454));
#51606=CARTESIAN_POINT('Ctrl Pts',(0.420862135428632,-0.566014089119677,
-0.76883046534151));
#51607=CARTESIAN_POINT('Ctrl Pts',(0.64016452944956,-0.296118660935354,
-0.752972954765568));
#51608=CARTESIAN_POINT('Ctrl Pts',(0.703848602098822,0.0457605883163558,
-0.737115444189624));
#51609=CARTESIAN_POINT('Ctrl Pts',(0.596433319942227,0.37651584426451,-0.721257933613681));
#51610=CARTESIAN_POINT('Ctrl Pts',(0.34403038572165,0.615743436684253,-0.705400423037737));
#51611=CARTESIAN_POINT('Ctrl Pts',(0.0079967149263957,0.705289258864694,
-0.689542912461795));
#51612=CARTESIAN_POINT('Ctrl Pts',(-0.329980886368106,0.623385515352452,
-0.67368540188585));
#51613=CARTESIAN_POINT('Ctrl Pts',(-0.58774305981707,0.389942280031795,
-0.657827891309908));
#51614=CARTESIAN_POINT('Ctrl Pts',(-0.702630106390092,0.0617075336872955,
-0.641970380733964));
#51615=CARTESIAN_POINT('Ctrl Pts',(-0.646714003660805,-0.281527766993847,
-0.62611287015802));
#51616=CARTESIAN_POINT('Ctrl Pts',(-0.433587460447112,-0.556326163561039,
-0.610255359582076));
#51617=CARTESIAN_POINT('Ctrl Pts',(-0.11505964981147,-0.695886602188015,
-0.594397849006135));
#51618=CARTESIAN_POINT('Ctrl Pts',(0.231438141567586,-0.66628317759591,
-0.578540338430189));
#51619=CARTESIAN_POINT('Ctrl Pts',(0.521675372676006,-0.474712219837212,
-0.562682827854247));
#51620=CARTESIAN_POINT('Ctrl Pts',(0.685097945892652,-0.167742930263535,
-0.546825317278303));
#51621=CARTESIAN_POINT('Ctrl Pts',(0.681979282582143,0.180003178438481,
-0.53096780670236));
#51622=CARTESIAN_POINT('Ctrl Pts',(0.513077502146677,0.483992110380683,
-0.515110296126415));
#51623=CARTESIAN_POINT('Ctrl Pts',(0.219451129913428,0.670326851393724,
-0.499252785550473));
#51624=CARTESIAN_POINT('Ctrl Pts',(-0.127521866330539,0.693711077989502,
-0.483395274974529));
#51625=CARTESIAN_POINT('Ctrl Pts',(-0.443495427494386,0.54846029201429,
-0.467537764398586));
#51626=CARTESIAN_POINT('Ctrl Pts',(-0.651659182275599,0.269883671725193,
-0.451680253822642));
#51627=CARTESIAN_POINT('Ctrl Pts',(-0.701410367526853,-0.0742992763408459,
-0.435822743246699));
#51628=CARTESIAN_POINT('Ctrl Pts',(-0.580654911117769,-0.400420729098558,
-0.419965232670754));
#51629=CARTESIAN_POINT('Ctrl Pts',(-0.318747394057519,-0.629203452711689,
-0.404107722094813));
#51630=CARTESIAN_POINT('Ctrl Pts',(0.0206447886986398,-0.705032395634334,
-0.388250211518869));
#51631=CARTESIAN_POINT('Ctrl Pts',(0.355018405902544,-0.609474213827725,
-0.372392700942925));
#51632=CARTESIAN_POINT('Ctrl Pts',(0.603090197140036,-0.365758254686112,
-0.356535190366982));
#51633=CARTESIAN_POINT('Ctrl Pts',(0.704556106741155,-0.0331297058619517,
-0.340677679791039));
#51634=CARTESIAN_POINT('Ctrl Pts',(0.634750676840949,0.307552379158318,
-0.324820169215095));
#51635=CARTESIAN_POINT('Ctrl Pts',(0.410642978477166,0.573471210647949,
-0.308962658639151));
#51636=CARTESIAN_POINT('Ctrl Pts',(0.0867116258434061,0.699984269273112,
-0.293105148063209));
#51637=CARTESIAN_POINT('Ctrl Pts',(-0.258298579659923,0.656337369834618,
-0.277247637487264));
#51638=CARTESIAN_POINT('Ctrl Pts',(-0.540518640889337,0.453140652074363,
-0.261390126911321));
#51639=CARTESIAN_POINT('Ctrl Pts',(-0.69134350977243,0.139789503985527,
-0.245532616335378));
#51640=CARTESIAN_POINT('Ctrl Pts',(-0.674108711481695,-0.207543320295039,
-0.229675105759435));
#51641=CARTESIAN_POINT('Ctrl Pts',(-0.493004432164587,-0.504424033259022,
-0.21381759518349));
#51642=CARTESIAN_POINT('Ctrl Pts',(-0.192054423564975,-0.67868406853937,
-0.197960084607548));
#51643=CARTESIAN_POINT('Ctrl Pts',(0.155580900692857,-0.687961374427907,
-0.182102574031604));
#51644=CARTESIAN_POINT('Ctrl Pts',(0.465398645427725,-0.530002638582951,
-0.16624506345566));
#51645=CARTESIAN_POINT('Ctrl Pts',(0.662076718045427,-0.243202481582967,
-0.150387552879718));
#51646=CARTESIAN_POINT('Ctrl Pts',(0.697820336995596,0.102713198692547,
-0.134530042303775));
#51647=CARTESIAN_POINT('Ctrl Pts',(0.563909430812559,0.423669692494884,
-0.11867253172783));
#51648=CARTESIAN_POINT('Ctrl Pts',(0.292957635797326,0.641617108208754,
-0.102815021151888));
#51649=CARTESIAN_POINT('Ctrl Pts',(-0.0492916150247689,0.703631926771629,
-0.0869575105759442));
#51650=CARTESIAN_POINT('Ctrl Pts',(-0.269341331211303,0.630876931084481,
-0.0763858368586482));
#51651=CARTESIAN_POINT('Ctrl Pts',(-0.364065050236216,0.570420484551968,
-0.0711000000000004));
#51652=CARTESIAN_POINT('Ctrl Pts',(-0.309090610374637,0.644553868208607,
-5.8529325805302));
#51653=CARTESIAN_POINT('Ctrl Pts',(-0.416124879237838,0.59322644760701,
-5.84764674367155));
#51654=CARTESIAN_POINT('Ctrl Pts',(-0.604023697624738,0.436275246927602,
-5.83707506995425));
#51655=CARTESIAN_POINT('Ctrl Pts',(-0.739055962843632,0.0945651317985082,
-5.82121755937831));
#51656=CARTESIAN_POINT('Ctrl Pts',(-0.694419411312428,-0.270037653032367,
-5.80536004880237));
#51657=CARTESIAN_POINT('Ctrl Pts',(-0.480981408007158,-0.569043457624426,
-5.78950253822642));
#51658=CARTESIAN_POINT('Ctrl Pts',(-0.150618127199263,-0.729696082934229,
-5.77364502765047));
#51659=CARTESIAN_POINT('Ctrl Pts',(0.21635756708914,-0.712978205946341,
-5.75778751707454));
#51660=CARTESIAN_POINT('Ctrl Pts',(0.5307394322654,-0.522935432074558,-5.74193000649859));
#51661=CARTESIAN_POINT('Ctrl Pts',(0.716102849126797,-0.205774873274938,
-5.72607249592265));
#51662=CARTESIAN_POINT('Ctrl Pts',(0.727388216078832,0.161409361904243,
-5.71021498534671));
#51663=CARTESIAN_POINT('Ctrl Pts',(0.561851852486622,0.489355578269279,
-5.69435747477076));
#51664=CARTESIAN_POINT('Ctrl Pts',(0.259734338354457,0.698344219171774,
-5.67849996419482));
#51665=CARTESIAN_POINT('Ctrl Pts',(-0.10552231794224,0.737571353378428,
-5.66264245361887));
#51666=CARTESIAN_POINT('Ctrl Pts',(-0.445127420322624,0.597501542829726,
-5.64678494304293));
#51667=CARTESIAN_POINT('Ctrl Pts',(-0.676526000512249,0.312184347418576,
-5.63092743246699));
#51668=CARTESIAN_POINT('Ctrl Pts',(-0.743467104430853,-0.0490220656779446,
-5.61506992189104));
#51669=CARTESIAN_POINT('Ctrl Pts',(-0.629677948764027,-0.398311664254308,
-5.59921241131511));
#51670=CARTESIAN_POINT('Ctrl Pts',(-0.362819665554462,-0.650775221019765,
-5.58335490073915));
#51671=CARTESIAN_POINT('Ctrl Pts',(-0.00776313892176305,-0.745041095302672,
-5.56749739016322));
#51672=CARTESIAN_POINT('Ctrl Pts',(0.349180538206236,-0.658194082882626,
-5.55163987958727));
#51673=CARTESIAN_POINT('Ctrl Pts',(0.621241522223168,-0.411345925533695,
-5.53578236901133));
#51674=CARTESIAN_POINT('Ctrl Pts',(0.742284200218653,-0.0645032201774955,
-5.51992485843538));
#51675=CARTESIAN_POINT('Ctrl Pts',(0.682884170243905,0.298019645844122,
-5.50406734785944));
#51676=CARTESIAN_POINT('Ctrl Pts',(0.457481052992605,0.58809657835964,-5.4882098372835));
#51677=CARTESIAN_POINT('Ctrl Pts',(0.120868347804697,0.735212446705008,
-5.47235232670755));
#51678=CARTESIAN_POINT('Ctrl Pts',(-0.245126381103904,0.703604687730767,
-5.45649481613161));
#51679=CARTESIAN_POINT('Ctrl Pts',(-0.551533060073818,0.500956867352424,
-5.44063730555566));
#51680=CARTESIAN_POINT('Ctrl Pts',(-0.723866942064143,0.176530874044159,
-5.42477979497972));
#51681=CARTESIAN_POINT('Ctrl Pts',(-0.720235188287465,-0.190808209615675,
-5.40892228440378));
#51682=CARTESIAN_POINT('Ctrl Pts',(-0.541520645886632,-0.511763509232599,
-5.39306477382784));
#51683=CARTESIAN_POINT('Ctrl Pts',(-0.231167235625787,-0.708313637082648,
-5.37720726325189));
#51684=CARTESIAN_POINT('Ctrl Pts',(0.135380880073045,-0.732678999708892,
-5.36134975267595));
#51685=CARTESIAN_POINT('Ctrl Pts',(0.469019104121168,-0.578936593482661,
-5.3454922421));
#51686=CARTESIAN_POINT('Ctrl Pts',(0.688642942309262,-0.284459834267554,
-5.32963473152407));
#51687=CARTESIAN_POINT('Ctrl Pts',(0.74086378677203,0.0791665886197745,
-5.31377722094811));
#51688=CARTESIAN_POINT('Ctrl Pts',(0.612987213213766,0.423548315709454,
-5.29791971037218));
#51689=CARTESIAN_POINT('Ctrl Pts',(0.336098882905021,0.664969202455183,
-5.28206219979623));
#51690=CARTESIAN_POINT('Ctrl Pts',(-0.0224921059648668,0.744741971741325,
-5.26620468922029));
#51691=CARTESIAN_POINT('Ctrl Pts',(-0.375615463291068,0.643474570624608,
-5.25034717864435));
#51692=CARTESIAN_POINT('Ctrl Pts',(-0.637430031720678,0.3857842064736,-5.23448966806841));
#51693=CARTESIAN_POINT('Ctrl Pts',(-0.744291010932289,0.0343131221150161,
-5.21863215749246));
#51694=CARTESIAN_POINT('Ctrl Pts',(-0.670221444315478,-0.325499178007507,
-5.20277464691652));
#51695=CARTESIAN_POINT('Ctrl Pts',(-0.433226986809527,-0.606185513851847,
-5.18691713634057));
#51696=CARTESIAN_POINT('Ctrl Pts',(-0.090918889826903,-0.739513525756312,
-5.17105962576463));
#51697=CARTESIAN_POINT('Ctrl Pts',(0.273490783180252,-0.693072356121164,
-5.15520211518868));
#51698=CARTESIAN_POINT('Ctrl Pts',(0.57141727158215,-0.478151441534479,
-5.13934460461274));
#51699=CARTESIAN_POINT('Ctrl Pts',(0.730437287482592,-0.146996150830428,
-5.1234870940368));
#51700=CARTESIAN_POINT('Ctrl Pts',(0.711894474897284,0.219892600863718,
-5.10762958346085));
#51701=CARTESIAN_POINT('Ctrl Pts',(0.52029642716401,0.533327410869022,-5.09177207288491));
#51702=CARTESIAN_POINT('Ctrl Pts',(0.202218930966826,0.71711505580522,-5.07591456230897));
#51703=CARTESIAN_POINT('Ctrl Pts',(-0.165016194463095,0.726578388660719,
-5.06005705173302));
#51704=CARTESIAN_POINT('Ctrl Pts',(-0.492137346062618,0.559416957120834,
-5.04419954115708));
#51705=CARTESIAN_POINT('Ctrl Pts',(-0.699624272153859,0.256266223129524,
-5.02834203058114));
#51706=CARTESIAN_POINT('Ctrl Pts',(-0.737038740595704,-0.109180557632705,
-5.01248452000518));
#51707=CARTESIAN_POINT('Ctrl Pts',(-0.595285625828881,-0.448086512835865,
-4.99662700942926));
#51708=CARTESIAN_POINT('Ctrl Pts',(-0.308823853261501,-0.67806660953081,
-4.98076949885331));
#51709=CARTESIAN_POINT('Ctrl Pts',(0.0527102599827489,-0.743214725228477,
-4.96491198827736));
#51710=CARTESIAN_POINT('Ctrl Pts',(0.401430976357553,-0.627693930609904,
-4.94905447770142));
#51711=CARTESIAN_POINT('Ctrl Pts',(0.652567381491205,-0.359586306632499,
-4.93319696712547));
#51712=CARTESIAN_POINT('Ctrl Pts',(0.745070441886303,-0.00406643962672281,
-4.91733945654954));
#51713=CARTESIAN_POINT('Ctrl Pts',(0.656453483698541,0.352441942799008,
-4.90148194597359));
#51714=CARTESIAN_POINT('Ctrl Pts',(0.408258503780039,0.623274813701928,
-4.88562443539765));
#51715=CARTESIAN_POINT('Ctrl Pts',(0.0608195012372539,0.742595103386185,
-4.8697669248217));
#51716=CARTESIAN_POINT('Ctrl Pts',(-0.301404182826923,0.681397107330463,
-4.85390941424576));
#51717=CARTESIAN_POINT('Ctrl Pts',(-0.590359182313632,0.454557515790763,
-4.83805190366981));
#51718=CARTESIAN_POINT('Ctrl Pts',(-0.735803098740191,0.117219022296814,
-4.82219439309388));
#51719=CARTESIAN_POINT('Ctrl Pts',(-0.702379805537885,-0.248614376246535,
-4.80633688251792));
#51720=CARTESIAN_POINT('Ctrl Pts',(-0.498214208951246,-0.554011824154478,
-4.79047937194199));
#51721=CARTESIAN_POINT('Ctrl Pts',(-0.172937155365935,-0.724733909512883,
-4.77462186136604));
#51722=CARTESIAN_POINT('Ctrl Pts',(0.194379387417532,-0.719279607003476,
-4.7587643507901));
#51723=CARTESIAN_POINT('Ctrl Pts',(0.514444024499226,-0.538974809208119,
-4.74290684021415));
#51724=CARTESIAN_POINT('Ctrl Pts',(0.709451880317066,-0.227650013877596,
-4.72704932963821));
#51725=CARTESIAN_POINT('Ctrl Pts',(0.731998274073198,0.139014481467747,
-4.71119181906227));
#51726=CARTESIAN_POINT('Ctrl Pts',(0.576602377343207,0.471885788879101,
-4.69533430848633));
#51727=CARTESIAN_POINT('Ctrl Pts',(0.281039554872709,0.690045844781952,
-4.67947679791038));
#51728=CARTESIAN_POINT('Ctrl Pts',(-0.0828414916736168,0.7404618738066,
-4.66361928733444));
#51729=CARTESIAN_POINT('Ctrl Pts',(-0.426584506071773,0.610878186288715,
-4.6477617767585));
#51730=CARTESIAN_POINT('Ctrl Pts',(-0.666628609167968,0.332795427767074,
-4.63190426618255));
#51731=CARTESIAN_POINT('Ctrl Pts',(-0.744621207745086,-0.0261869486603079,
-4.61604675560661));
#51732=CARTESIAN_POINT('Ctrl Pts',(-0.641602992576138,-0.378803510043443,
-4.60018924503066));
#51733=CARTESIAN_POINT('Ctrl Pts',(-0.382616778402954,-0.639336296629898,
-4.58433173445473));
#51734=CARTESIAN_POINT('Ctrl Pts',(-0.0306198177035606,-0.744452097899986,
-4.56847422387878));
#51735=CARTESIAN_POINT('Ctrl Pts',(0.328820549202407,-0.668598194528011,
-4.55261671330283));
#51736=CARTESIAN_POINT('Ctrl Pts',(0.608327555940194,-0.430213997898396,
-4.53675920272689));
#51737=CARTESIAN_POINT('Ctrl Pts',(0.7399555272979,-0.087248592683062,-4.52090169215095));
#51738=CARTESIAN_POINT('Ctrl Pts',(0.691706870460046,0.276926171862212,
-4.50504418157501));
#51739=CARTESIAN_POINT('Ctrl Pts',(0.475310406128392,0.573782639272009,
-4.48918667099905));
#51740=CARTESIAN_POINT('Ctrl Pts',(0.1433701961978,0.731157634266437,-4.47332916042313));
#51741=CARTESIAN_POINT('Ctrl Pts',(-0.223422037299627,0.7107946908586,-4.45747164984717));
#51742=CARTESIAN_POINT('Ctrl Pts',(-0.535902354402842,0.517643860051851,
-4.44161413927123));
#51743=CARTESIAN_POINT('Ctrl Pts',(-0.718109560493481,0.198658396328338,
-4.42575662869528));
#51744=CARTESIAN_POINT('Ctrl Pts',(-0.72575069923105,-0.16861916222521,
-4.40989911811935));
#51745=CARTESIAN_POINT('Ctrl Pts',(-0.556968277535239,-0.494906897429525,
-4.39404160754339));
#51746=CARTESIAN_POINT('Ctrl Pts',(-0.252791805685121,-0.700887153743271,
-4.37818409696747));
#51747=CARTESIAN_POINT('Ctrl Pts',(0.11283611285958,-0.73648795709002,-4.3623265863915));
#51748=CARTESIAN_POINT('Ctrl Pts',(0.451034572779929,-0.59305506781505,
-4.34646907581558));
#51749=CARTESIAN_POINT('Ctrl Pts',(0.679590526957342,-0.305455749616425,
-4.33061156523962));
#51750=CARTESIAN_POINT('Ctrl Pts',(0.742944049322229,0.0563971531247643,
-4.31475405466369));
#51751=CARTESIAN_POINT('Ctrl Pts',(0.625694460283858,0.4045404079619,-4.29889654408774));
#51752=CARTESIAN_POINT('Ctrl Pts',(0.356344095395492,0.654343476303278,
-4.2830390335118));
#51753=CARTESIAN_POINT('Ctrl Pts',(0.000369640284832444,0.745081447004251,
-4.26718152293585));
#51754=CARTESIAN_POINT('Ctrl Pts',(-0.355694671101819,0.654696723875764,
-4.25132401235991));
#51755=CARTESIAN_POINT('Ctrl Pts',(-0.625292761554132,0.405161031753915,
-4.23546650178396));
#51756=CARTESIAN_POINT('Ctrl Pts',(-0.742887725556159,0.0571342849949572,
-4.21960899120803));
#51757=CARTESIAN_POINT('Ctrl Pts',(-0.679893269963091,-0.304781299890241,
-4.20375148063208));
#51758=CARTESIAN_POINT('Ctrl Pts',(-0.451622788416938,-0.592607252981601,
-4.18789397005613));
#51759=CARTESIAN_POINT('Ctrl Pts',(-0.113566811121643,-0.736375636964961,
-4.17203645948019));
#51760=CARTESIAN_POINT('Ctrl Pts',(0.252096251067092,-0.701137632353168,
-4.15617894890425));
#51761=CARTESIAN_POINT('Ctrl Pts',(0.556476949722059,-0.49545928564507,
-4.1403214383283));
#51762=CARTESIAN_POINT('Ctrl Pts',(0.725583035657959,-0.169339179368713,
-4.12446392775236));
#51763=CARTESIAN_POINT('Ctrl Pts',(0.718306318688587,0.197945780040748,
-4.10860641717642));
#51764=CARTESIAN_POINT('Ctrl Pts',(0.536415704193378,0.51711187532159,-4.09274890660048));
#51765=CARTESIAN_POINT('Ctrl Pts',(0.224127187902907,0.710572658456983,
-4.07689139602453));
#51766=CARTESIAN_POINT('Ctrl Pts',(-0.142644660641527,0.731299528301743,
-4.06103388544859));
#51767=CARTESIAN_POINT('Ctrl Pts',(-0.474740856880215,0.574253966562295,
-4.04517637487265));
#51768=CARTESIAN_POINT('Ctrl Pts',(-0.691431759892533,0.277612356922026,
-4.0293188642967));
#51769=CARTESIAN_POINT('Ctrl Pts',(-0.740041732350872,-0.0865143553580023,
-4.01346135372077));
#51770=CARTESIAN_POINT('Ctrl Pts',(-0.608754120929568,-0.429610194892017,
-3.99760384314481));
#51771=CARTESIAN_POINT('Ctrl Pts',(-0.329483779961226,-0.668271604997811,
-3.98174633256888));
#51772=CARTESIAN_POINT('Ctrl Pts',(0.0298811466925253,-0.744482112865198,
-3.96588882199293));
#51773=CARTESIAN_POINT('Ctrl Pts',(0.381982231513381,-0.639715619718594,
-3.95003131141699));
#51774=CARTESIAN_POINT('Ctrl Pts',(0.641226822530954,-0.379439931175865,
-3.93417380084104));
#51775=CARTESIAN_POINT('Ctrl Pts',(0.74459485814713,-0.0269257595017122,
-3.9183162902651));
#51776=CARTESIAN_POINT('Ctrl Pts',(0.666958485370885,0.332133825581894,
-3.90245877968916));
#51777=CARTESIAN_POINT('Ctrl Pts',(0.427190418095336,0.610454622385171,
-3.88660126911321));
#51778=CARTESIAN_POINT('Ctrl Pts',(0.0835761476769501,0.740379312814297,
-3.87074375853727));
#51779=CARTESIAN_POINT('Ctrl Pts',(-0.280354743250511,0.690324356546131,
-3.85488624796132));
#51780=CARTESIAN_POINT('Ctrl Pts',(-0.576133881735919,0.472457669659188,
-3.83902873738538));
#51781=CARTESIAN_POINT('Ctrl Pts',(-0.731859981609243,0.139740712116434,
-3.82317122680944));
#51782=CARTESIAN_POINT('Ctrl Pts',(-0.709677408668316,-0.226945973592202,
-3.80731371623349));
#51783=CARTESIAN_POINT('Ctrl Pts',(-0.514978549723044,-0.538464105237332,
-3.79145620565755));
#51784=CARTESIAN_POINT('Ctrl Pts',(-0.195092971171135,-0.71908638695466,
-3.77559869508161));
#51785=CARTESIAN_POINT('Ctrl Pts',(0.172217978966369,-0.724905143466804,
-3.75974118450566));
#51786=CARTESIAN_POINT('Ctrl Pts',(0.497664265312189,-0.554505886655109,
-3.74388367392972));
#51787=CARTESIAN_POINT('Ctrl Pts',(0.702132781082156,-0.249311165080358,
-3.72802616335378));
#51788=CARTESIAN_POINT('Ctrl Pts',(0.735919042922848,0.116488890317527,
-3.71216865277783));
#51789=CARTESIAN_POINT('Ctrl Pts',(0.590809910131837,0.453971529276781,
-3.69631114220189));
#51790=CARTESIAN_POINT('Ctrl Pts',(0.302080126344257,0.681097714407944,
-3.68045363162595));
#51791=CARTESIAN_POINT('Ctrl Pts',(-0.0600826578968981,0.742655083820162,
-3.66459612105001));
#51792=CARTESIAN_POINT('Ctrl Pts',(-0.407639880699809,0.623679586780693,
-3.64873861047406));
#51793=CARTESIAN_POINT('Ctrl Pts',(-0.656103462664489,0.353093111775854,
-3.63288109989812));
#51794=CARTESIAN_POINT('Ctrl Pts',(-0.745074109908502,-0.00332716815676224,
-3.61702358932217));
#51795=CARTESIAN_POINT('Ctrl Pts',(-0.652923846905976,-0.358938643009346,
-3.60116607874623));
#51796=CARTESIAN_POINT('Ctrl Pts',(-0.402053585583011,-0.627295316118121,
-3.58530856817028));
#51797=CARTESIAN_POINT('Ctrl Pts',(-0.0534476622362749,-0.743162059516877,
-3.56945105759435));
#51798=CARTESIAN_POINT('Ctrl Pts',(0.308150913929887,-0.678372695166945,
-3.5535935470184));
#51799=CARTESIAN_POINT('Ctrl Pts',(0.594840735004374,-0.448676943115362,
-3.53773603644246));
#51800=CARTESIAN_POINT('Ctrl Pts',(0.736930047293309,-0.109911804189408,
-3.52187852586651));
#51801=CARTESIAN_POINT('Ctrl Pts',(0.699878198751708,0.255571919850272,
-3.50602101529057));
#51802=CARTESIAN_POINT('Ctrl Pts',(0.492692165256099,0.558928376090486,
-3.49016350471463));
#51803=CARTESIAN_POINT('Ctrl Pts',(0.165737034625333,0.72641429959596,-3.47430599413868));
#51804=CARTESIAN_POINT('Ctrl Pts',(-0.201507299688257,0.71731534730287,
-3.45844848356274));
#51805=CARTESIAN_POINT('Ctrl Pts',(-0.519766996023564,0.533843393841798,
-3.44259097298679));
#51806=CARTESIAN_POINT('Ctrl Pts',(-0.711675943911235,0.220598844425674,
-3.42673346241086));
#51807=CARTESIAN_POINT('Ctrl Pts',(-0.730582779596139,-0.146271328227603,
-3.4108759518349));
#51808=CARTESIAN_POINT('Ctrl Pts',(-0.571891418952435,-0.477584237839209,
-3.39501844125897));
#51809=CARTESIAN_POINT('Ctrl Pts',(-0.274178324785384,-0.692800653522907,
-3.37916093068302));
#51810=CARTESIAN_POINT('Ctrl Pts',(0.0901850892553483,-0.739603372747782,
-3.36330342010708));
#51811=CARTESIAN_POINT('Ctrl Pts',(0.432625307684578,-0.606615069426003,
-3.34744590953114));
#51812=CARTESIAN_POINT('Ctrl Pts',(0.669898149497886,-0.326164021012737,
-3.33158839895519));
#51813=CARTESIAN_POINT('Ctrl Pts',(0.744324690525857,0.0335746091187453,
-3.31573088837925));
#51814=CARTESIAN_POINT('Ctrl Pts',(0.637812498514814,0.38515154944798,-3.2998733778033));
#51815=CARTESIAN_POINT('Ctrl Pts',(0.376253742999091,0.643101562883393,
-3.28401586722737));
#51816=CARTESIAN_POINT('Ctrl Pts',(0.0232310384487809,0.744719288159291,
-3.26815835665141));
#51817=CARTESIAN_POINT('Ctrl Pts',(-0.335438925580633,0.665302357210013,
-3.25230084607548));
#51818=CARTESIAN_POINT('Ctrl Pts',(-0.612566660823242,0.424156321834006,
-3.23644333549953));
#51819=CARTESIAN_POINT('Ctrl Pts',(-0.740784871872864,0.0799016452158113,
-3.22058582492359));
#51820=CARTESIAN_POINT('Ctrl Pts',(-0.688924848413769,-0.283776412941517,
-3.20472831434764));
#51821=CARTESIAN_POINT('Ctrl Pts',(-0.46959330235475,-0.578470941091642,
-3.1888708037717));
#51822=CARTESIAN_POINT('Ctrl Pts',(-0.136107787935974,-0.732544312220813,
-3.17301329319576));
#51823=CARTESIAN_POINT('Ctrl Pts',(0.23046432299014,-0.708542655831381,
-3.15715578261981));
#51824=CARTESIAN_POINT('Ctrl Pts',(0.541012600308007,-0.512300561791472,
-3.14129827204387));
#51825=CARTESIAN_POINT('Ctrl Pts',(0.720045511141503,-0.191522743267892,
-3.12544076146793));
#51826=CARTESIAN_POINT('Ctrl Pts',(0.724041742183651,0.175812556091856,
-3.10958325089198));
#51827=CARTESIAN_POINT('Ctrl Pts',(0.552029845098931,0.500409381830454,
-3.09372574031604));
#51828=CARTESIAN_POINT('Ctrl Pts',(0.245824387000732,0.703361123505987,
-3.0778682297401));
#51829=CARTESIAN_POINT('Ctrl Pts',(-0.120138800083435,0.73533201209957,
-3.06201071916415));
#51830=CARTESIAN_POINT('Ctrl Pts',(-0.456897310025201,0.588550208049937,
-3.04615320858821));
#51831=CARTESIAN_POINT('Ctrl Pts',(-0.682588134779086,0.298697066545184,
-3.03029569801227));
#51832=CARTESIAN_POINT('Ctrl Pts',(-0.742347835835951,-0.0637666835704077,
-3.01443818743632));
#51833=CARTESIAN_POINT('Ctrl Pts',(-0.621649359702007,-0.410729318269314,
-2.99858067686038));
#51834=CARTESIAN_POINT('Ctrl Pts',(-0.349833435805405,-0.657847297247982,
-2.98272316628444));
#51835=CARTESIAN_POINT('Ctrl Pts',(0.0070238946910416,-0.745048430779676,
-2.96686565570849));
#51836=CARTESIAN_POINT('Ctrl Pts',(0.362173778662374,-0.651134896433379,
-2.95100814513255));
#51837=CARTESIAN_POINT('Ctrl Pts',(0.629282428095556,-0.398936241765586,
-2.9351506345566));
#51838=CARTESIAN_POINT('Ctrl Pts',(0.74341809851486,-0.0497597237174798,
-2.91929312398067));
#51839=CARTESIAN_POINT('Ctrl Pts',(0.676835420375122,0.31151294199362,-2.90343561340472));
#51840=CARTESIAN_POINT('Ctrl Pts',(0.445720052406056,0.597059573398696,
-2.88757810282878));
#51841=CARTESIAN_POINT('Ctrl Pts',(0.106254091478081,0.737466316076915,
-2.87172059225283));
#51842=CARTESIAN_POINT('Ctrl Pts',(-0.259041297032996,0.698601535737899,
-2.85586308167689));
#51843=CARTESIAN_POINT('Ctrl Pts',(-0.561366042911193,0.489912915904567,
-2.84000557110094));
#51844=CARTESIAN_POINT('Ctrl Pts',(-0.727227680863051,0.162130809812444,
-2.824148060525));
#51845=CARTESIAN_POINT('Ctrl Pts',(-0.716306717241799,-0.205063858683501,
-2.80829054994906));
#51846=CARTESIAN_POINT('Ctrl Pts',(-0.531257941477839,-0.522409321242087,
-2.79243303937311));
#51847=CARTESIAN_POINT('Ctrl Pts',(-0.217065070305726,-0.71276170951943,
-2.77657552879717));
#51848=CARTESIAN_POINT('Ctrl Pts',(0.149894394945637,-0.729848045601117,
-2.76071801822123));
#51849=CARTESIAN_POINT('Ctrl Pts',(0.480415861758509,-0.569514792674184,
-2.74486050764528));
#51850=CARTESIAN_POINT('Ctrl Pts',(0.694152491974035,-0.270737543000829,
-2.72900299706934));
#51851=CARTESIAN_POINT('Ctrl Pts',(0.739146805788744,0.0938536030005615,
-2.7131454864934));
#51852=CARTESIAN_POINT('Ctrl Pts',(0.604461084436589,0.435629770224248,
-2.69728797591746));
#51853=CARTESIAN_POINT('Ctrl Pts',(0.322836232646514,0.671508202626368,
-2.68143046534151));
#51854=CARTESIAN_POINT('Ctrl Pts',(-0.0372672450143224,0.744148944602444,
-2.66557295476557));
#51855=CARTESIAN_POINT('Ctrl Pts',(-0.388311385825831,0.635893675815314,
-2.64971544418962));
#51856=CARTESIAN_POINT('Ctrl Pts',(-0.644960471535362,0.373058292309355,
-2.63385793361369));
#51857=CARTESIAN_POINT('Ctrl Pts',(-0.744825384873282,0.019535745500423,
-2.61800042303773));
#51858=CARTESIAN_POINT('Ctrl Pts',(-0.663629850815514,-0.338735767834558,
-2.6021429124618));
#51859=CARTESIAN_POINT('Ctrl Pts',(-0.42111178380698,-0.614663619260805,
-2.58628540188585));
#51860=CARTESIAN_POINT('Ctrl Pts',(-0.076225175757575,-0.741172194489656,
-2.57042789130991));
#51861=CARTESIAN_POINT('Ctrl Pts',(0.287191096701467,-0.687508380515683,
-2.55457038073397));
#51862=CARTESIAN_POINT('Ctrl Pts',(0.580793759806059,-0.466717374729323,
-2.53871287015802));
#51863=CARTESIAN_POINT('Ctrl Pts',(0.733210609254479,-0.132471513090796,
-2.52285535958208));
#51864=CARTESIAN_POINT('Ctrl Pts',(0.707390460282839,0.233976998879638,
-2.50699784900613));
#51865=CARTESIAN_POINT('Ctrl Pts',(0.509609962183139,0.543547776876688,
-2.49114033843019));
#51866=CARTESIAN_POINT('Ctrl Pts',(0.187947800509531,0.720986909442548,
-2.47528282785425));
#51867=CARTESIAN_POINT('Ctrl Pts',(-0.179402805111352,0.723160516636568,
-2.4594253172783));
#51868=CARTESIAN_POINT('Ctrl Pts',(-0.50314217940581,0.54954021382121,-2.44356780670236));
#51869=CARTESIAN_POINT('Ctrl Pts',(-0.704572150775774,0.242331557282762,
-2.42771029612642));
#51870=CARTESIAN_POINT('Ctrl Pts',(-0.734726879071544,-0.123785752304851,
-2.41185278555047));
#51871=CARTESIAN_POINT('Ctrl Pts',(-0.586276017198065,-0.459811842999138,
-2.39599527497453));
#51872=CARTESIAN_POINT('Ctrl Pts',(-0.295306653502441,-0.684061751380004,
-2.38013776439859));
#51873=CARTESIAN_POINT('Ctrl Pts',(0.0674491394529376,-0.742022312933343,
-2.36428025382264));
#51874=CARTESIAN_POINT('Ctrl Pts',(0.413808644615465,-0.619603829027388,
-2.3484227432467));
#51875=CARTESIAN_POINT('Ctrl Pts',(0.659574937124499,-0.34656514772998,
-2.33256523267076));
#51876=CARTESIAN_POINT('Ctrl Pts',(0.745004410249938,0.01072044831298,-2.31670772209481));
#51877=CARTESIAN_POINT('Ctrl Pts',(0.649329916497877,0.365399998419196,
-2.30085021151887));
#51878=CARTESIAN_POINT('Ctrl Pts',(0.395809077043586,0.631254048568238,
-2.28499270094292));
#51879=CARTESIAN_POINT('Ctrl Pts',(0.0460705602272718,0.743655836247005,
-2.26913519036698));
#51880=CARTESIAN_POINT('Ctrl Pts',(-0.314867301315917,0.675281483431852,
-2.25327767979104));
#51881=CARTESIAN_POINT('Ctrl Pts',(-0.599263713541787,0.442752189080975,
-2.2374201692151));
#51882=CARTESIAN_POINT('Ctrl Pts',(-0.737984430114058,0.10259376303226,
-2.22156265863915));
#51883=CARTESIAN_POINT('Ctrl Pts',(-0.697307674740288,-0.262504297207077,
-2.20570514806321));
#51884=CARTESIAN_POINT('Ctrl Pts',(-0.487121606009267,-0.563789890174383,
-2.18984763748727));
#51885=CARTESIAN_POINT('Ctrl Pts',(-0.158520593707075,-0.728023159435637,
-2.17399012691132));
#51886=CARTESIAN_POINT('Ctrl Pts',(0.208615369472112,-0.715280453335545,
-2.15813261633538));
#51887=CARTESIAN_POINT('Ctrl Pts',(0.525038785929141,-0.528659410749439,
-2.14227510575943));
#51888=CARTESIAN_POINT('Ctrl Pts',(0.713829928552495,-0.213525952536522,
-2.12641759518349));
#51889=CARTESIAN_POINT('Ctrl Pts',(0.729095344404152,0.153513771603985,
-2.11056008460755));
#51890=CARTESIAN_POINT('Ctrl Pts',(0.567124146234676,0.483235658929967,
-2.0947025740316));
#51891=CARTESIAN_POINT('Ctrl Pts',(0.267290096272606,0.695487241966717,
-2.07884506345566));
#51892=CARTESIAN_POINT('Ctrl Pts',(-0.0975198062831407,0.7386720427134,
-2.06298755287972));
#51893=CARTESIAN_POINT('Ctrl Pts',(-0.438623508547968,0.602292218987561,
-2.04713004230377));
#51894=CARTESIAN_POINT('Ctrl Pts',(-0.673101724747398,0.319500496785165,
-2.03127253172783));
#51895=CARTESIAN_POINT('Ctrl Pts',(-0.743954879421426,-0.0409589634749339,
-2.01541502115189));
#51896=CARTESIAN_POINT('Ctrl Pts',(-0.633959198857162,-0.391461662858922,
-1.99955751057594));
#51897=CARTESIAN_POINT('Ctrl Pts',(-0.369853657771412,-0.646803502724741,
-1.9837));
#51898=CARTESIAN_POINT('Ctrl Pts',(-0.015839971626384,-0.744913145677242,
-1.96784248942406));
#51899=CARTESIAN_POINT('Ctrl Pts',(0.342024271182878,-0.661941007360709,
-1.95198497884811));
#51900=CARTESIAN_POINT('Ctrl Pts',(0.6167454460755,-0.418056878963882,-1.93612746827217));
#51901=CARTESIAN_POINT('Ctrl Pts',(0.741541271129677,-0.0725468298085624,
-1.92026995769623));
#51902=CARTESIAN_POINT('Ctrl Pts',(0.686074987722085,0.290598710468627,
-1.90441244712028));
#51903=CARTESIAN_POINT('Ctrl Pts',(0.463829957581682,0.583102280696676,
-1.88855493654435));
#51904=CARTESIAN_POINT('Ctrl Pts',(0.12883197709769,0.733858856307525,-1.87269742596839));
#51905=CARTESIAN_POINT('Ctrl Pts',(-0.237483914786634,0.706220850387119,
-1.85683991539246));
#51906=CARTESIAN_POINT('Ctrl Pts',(-0.546069572533108,0.506906817134467,
-1.84098240481651));
#51907=CARTESIAN_POINT('Ctrl Pts',(-0.721910558682716,0.184368230902995,
-1.82512489424057));
#51908=CARTESIAN_POINT('Ctrl Pts',(-0.722261488519323,-0.182988637641087,
-1.80926738366462));
#51909=CARTESIAN_POINT('Ctrl Pts',(-0.547037054111024,-0.505862590762966,
-1.79340987308868));
#51910=CARTESIAN_POINT('Ctrl Pts',(-0.238832761912019,-0.705765833078766,
-1.77755236251274));
#51911=CARTESIAN_POINT('Ctrl Pts',(0.12742965720205,-0.734103658735778,
-1.76169485193679));
#51912=CARTESIAN_POINT('Ctrl Pts',(0.462715056449375,-0.583987393561662,
-1.74583734136085));
#51913=CARTESIAN_POINT('Ctrl Pts',(0.685518527933592,-0.29190897068033,
-1.72997983078491));
#51914=CARTESIAN_POINT('Ctrl Pts',(0.741678523125974,0.0711299348907594,
-1.71412232020896));
#51915=CARTESIAN_POINT('Ctrl Pts',(0.617543045113172,0.416877783932221,
-1.69826480963302));
#51916=CARTESIAN_POINT('Ctrl Pts',(0.343288328007429,0.66128633976346,-1.68240729905708));
#51917=CARTESIAN_POINT('Ctrl Pts',(-0.0144167380217974,0.744942049402972,
-1.66654978848113));
#51918=CARTESIAN_POINT('Ctrl Pts',(-0.368617222857599,0.647508951533985,
-1.65069227790519));
#51919=CARTESIAN_POINT('Ctrl Pts',(-0.633210128999356,0.392672168400699,
-1.63483476732924));
#51920=CARTESIAN_POINT('Ctrl Pts',(-0.743875266860757,0.0423802625844482,
-1.6189772567533));
#51921=CARTESIAN_POINT('Ctrl Pts',(-0.673710922591512,-0.318213909320104,
-1.60311974617735));
#51922=CARTESIAN_POINT('Ctrl Pts',(-0.439773426202145,-0.601453101172749,
-1.58726223560142));
#51923=CARTESIAN_POINT('Ctrl Pts',(-0.0989309089608898,-0.738484376649947,
-1.57140472502547));
#51924=CARTESIAN_POINT('Ctrl Pts',(0.265960835121323,-0.69599664761079,
-1.55554721444953));
#51925=CARTESIAN_POINT('Ctrl Pts',(0.566199858210426,-0.484318304285913,
-1.53968970387358));
#51926=CARTESIAN_POINT('Ctrl Pts',(0.728800715730834,-0.15490647518458,
-1.52383219329764));
#51927=CARTESIAN_POINT('Ctrl Pts',(0.714236580848404,0.212161744623924,
-1.5079746827217));
#51928=CARTESIAN_POINT('Ctrl Pts',(0.526047865626554,0.527655325353243,
-1.49211717214575));
#51929=CARTESIAN_POINT('Ctrl Pts',(0.209981578243146,0.714880574713293,
-1.47625966156981));
#51930=CARTESIAN_POINT('Ctrl Pts',(-0.157129369101771,0.728324694535046,
-1.46040215099387));
#51931=CARTESIAN_POINT('Ctrl Pts',(-0.486043559936557,0.564719538486219,
-1.44454464041792));
#51932=CARTESIAN_POINT('Ctrl Pts',(-0.696804870642429,0.263836069469049,
-1.42868712984198));
#51933=CARTESIAN_POINT('Ctrl Pts',(-0.738179095209345,-0.101183608849463,
-1.41282961926604));
#51934=CARTESIAN_POINT('Ctrl Pts',(-0.600108526471472,-0.441606448956679,
-1.39697210869009));
#51935=CARTESIAN_POINT('Ctrl Pts',(-0.316156895546953,-0.674678676632072,
-1.38111459811415));
#51936=CARTESIAN_POINT('Ctrl Pts',(0.0446496736188302,-0.743742499760246,
-1.36525708753821));
#51937=CARTESIAN_POINT('Ctrl Pts',(0.39460230299459,-0.632009115262792,
-1.34939957696226));
#51938=CARTESIAN_POINT('Ctrl Pts',(0.648630611080299,-0.366639918276074,
-1.33354206638632));
#51939=CARTESIAN_POINT('Ctrl Pts',(0.744982568410704,-0.0121438078081822,
-1.31768455581038));
#51940=CARTESIAN_POINT('Ctrl Pts',(0.66023586842107,0.345304354670142,-1.30182704523443));
#51941=CARTESIAN_POINT('Ctrl Pts',(0.414991682509506,0.618812090017495,
-1.28596953465849));
#51942=CARTESIAN_POINT('Ctrl Pts',(0.0688666979212898,0.741892092707091,
-1.27011202408255));
#51943=CARTESIAN_POINT('Ctrl Pts',(-0.293999170355266,0.684624705319858,
-1.2542545135066));
#51944=CARTESIAN_POINT('Ctrl Pts',(-0.585396446932924,0.46093112199351,
-1.23839700293066));
#51945=CARTESIAN_POINT('Ctrl Pts',(-0.734489037421575,0.12518926955381,
-1.22253949235471));
#51946=CARTESIAN_POINT('Ctrl Pts',(-0.705033854937372,-0.240984984378776,
-1.20668198177877));
#51947=CARTESIAN_POINT('Ctrl Pts',(-0.504191193190784,-0.54857792519636,
-1.19082447120283));
#51948=CARTESIAN_POINT('Ctrl Pts',(-0.180784122569197,-0.722816436123844,
-1.17496696062689));
#51949=CARTESIAN_POINT('Ctrl Pts',(0.186569965405974,-0.721344679963956,
-1.15910945005094));
#51950=CARTESIAN_POINT('Ctrl Pts',(0.508570548931574,-0.544520427590487,
-1.143251939475));
#51951=CARTESIAN_POINT('Ctrl Pts',(0.706942141029221,-0.235328087020886,
-1.12739442889906));
#51952=CARTESIAN_POINT('Ctrl Pts',(0.733462366434538,0.131070425070409,
-1.11153691832311));
#51953=CARTESIAN_POINT('Ctrl Pts',(0.581684393481415,0.46560687890542,-1.09567940774717));
#51954=CARTESIAN_POINT('Ctrl Pts',(0.288504101722052,0.686958428577336,
-1.07982189717123));
#51955=CARTESIAN_POINT('Ctrl Pts',(-0.0748089792710891,0.741316474877164,
-1.06396438659528));
#51956=CARTESIAN_POINT('Ctrl Pts',(-0.419936660664375,0.615467058691158,
-1.04810687601934));
#51957=CARTESIAN_POINT('Ctrl Pts',(-0.662981463034035,0.340003057305575,
-1.03224936544339));
#51958=CARTESIAN_POINT('Ctrl Pts',(-0.744861349773961,-0.0181126728232756,
-1.01639185486745));
#51959=CARTESIAN_POINT('Ctrl Pts',(-0.64567204636971,-0.371825372776845,
-1.00053434429151));
#51960=CARTESIAN_POINT('Ctrl Pts',(-0.389525593060484,-0.635150621234654,
-0.984676833715565));
#51961=CARTESIAN_POINT('Ctrl Pts',(-0.0386889216357713,-0.744076384954227,
-0.968819323139621));
#51962=CARTESIAN_POINT('Ctrl Pts',(0.321552683620266,-0.672123776517757,
-0.952961812563677));
#51963=CARTESIAN_POINT('Ctrl Pts',(0.603627682393802,-0.436783837099971,
-0.937104301987736));
#51964=CARTESIAN_POINT('Ctrl Pts',(0.738966143377032,-0.0952656194351606,
-0.92124679141179));
#51965=CARTESIAN_POINT('Ctrl Pts',(0.694668486623927,0.269410825683588,
-0.905389280835849));
#51966=CARTESIAN_POINT('Ctrl Pts',(0.481503079745453,0.568595887691366,
-0.889531770259903));
#51967=CARTESIAN_POINT('Ctrl Pts',(0.15128854321635,0.729560330606979,-0.873674259683962));
#51968=CARTESIAN_POINT('Ctrl Pts',(-0.215702896835252,0.713175125478146,
-0.857816749108016));
#51969=CARTESIAN_POINT('Ctrl Pts',(-0.530258875101165,0.523423370399467,
-0.841959238532075));
#51970=CARTESIAN_POINT('Ctrl Pts',(-0.715913622137308,0.206432034680005,
-0.82610172795613));
#51971=CARTESIAN_POINT('Ctrl Pts',(-0.727536114965444,-0.160741098431234,
-0.810244217380188));
#51972=CARTESIAN_POINT('Ctrl Pts',(-0.562301028624769,-0.488839495654161,
-0.794386706804242));
#51973=CARTESIAN_POINT('Ctrl Pts',(-0.260375547620419,-0.698105345564161,
-0.778529196228302));
#51974=CARTESIAN_POINT('Ctrl Pts',(0.104844920505069,-0.737667975411821,
-0.762671685652355));
#51975=CARTESIAN_POINT('Ctrl Pts',(0.444578518017195,-0.597910060645851,
-0.746814175076414));
#51976=CARTESIAN_POINT('Ctrl Pts',(0.676239019459429,-0.312805511243711,
-0.730956664500469));
#51977=CARTESIAN_POINT('Ctrl Pts',(0.743511810847211,0.0483392845891503,
-0.715099153924527));
#51978=CARTESIAN_POINT('Ctrl Pts',(0.630043473038817,0.397733228917417,
-0.699241643348582));
#51979=CARTESIAN_POINT('Ctrl Pts',(0.363417152938314,0.65044175162277,-0.68338413277264));
#51980=CARTESIAN_POINT('Ctrl Pts',(0.00844734503701607,0.74503365136463,
-0.667526622196697));
#51981=CARTESIAN_POINT('Ctrl Pts',(-0.348575937548106,0.658514475973267,
-0.651669111620753));
#51982=CARTESIAN_POINT('Ctrl Pts',(-0.620863500210685,0.411916269902062,
-0.63581160104481));
#51983=CARTESIAN_POINT('Ctrl Pts',(-0.742224650585465,0.0651848706922794,
-0.619954090468866));
#51984=CARTESIAN_POINT('Ctrl Pts',(-0.68315756901167,-0.297392392649777,
-0.604096579892923));
#51985=CARTESIAN_POINT('Ctrl Pts',(-0.458020939327533,-0.587676202037661,
-0.588239069316978));
#51986=CARTESIAN_POINT('Ctrl Pts',(-0.121543480134323,-0.735101137082999,
-0.572381558741037));
#51987=CARTESIAN_POINT('Ctrl Pts',(0.244480121467758,-0.703829503154735,
-0.556524048165091));
#51988=CARTESIAN_POINT('Ctrl Pts',(0.551072773116448,-0.50146315720452,
-0.54066653758915));
#51989=CARTESIAN_POINT('Ctrl Pts',(0.723704519465442,-0.177195563740772,
-0.524809027013205));
#51990=CARTESIAN_POINT('Ctrl Pts',(0.720410113539927,0.190146700242023,
-0.508951516437263));
#51991=CARTESIAN_POINT('Ctrl Pts',(0.541990396213754,0.511265987247614,
-0.493094005861317));
#51992=CARTESIAN_POINT('Ctrl Pts',(0.231817618885443,0.708101045669594,
-0.477236495285376));
#51993=CARTESIAN_POINT('Ctrl Pts',(-0.134707966280404,0.732803017954034,
-0.461378984709431));
#51994=CARTESIAN_POINT('Ctrl Pts',(-0.468487239181182,0.579367073653829,
-0.445521474133488));
#51995=CARTESIAN_POINT('Ctrl Pts',(-0.688381417856275,0.28509213044415,
-0.429663963557544));
#51996=CARTESIAN_POINT('Ctrl Pts',(-0.740936177115086,-0.0784861820171191,
-0.413806452981602));
#51997=CARTESIAN_POINT('Ctrl Pts',(-0.613375920837422,-0.422985199523109,
-0.397948942405657));
#51998=CARTESIAN_POINT('Ctrl Pts',(-0.336709416558958,-0.664660265179164,
-0.382091431829715));
#51999=CARTESIAN_POINT('Ctrl Pts',(0.0218081618463334,-0.744762313402212,
-0.366233921253771));
#52000=CARTESIAN_POINT('Ctrl Pts',(0.375024368975919,-0.643819246122629,
-0.350376410677828));
#52001=CARTESIAN_POINT('Ctrl Pts',(0.637075477940402,-0.386369428685465,
-0.334518900101884));
#52002=CARTESIAN_POINT('Ctrl Pts',(0.744259184723121,-0.0349966278611624,
-0.318661389525941));
#52003=CARTESIAN_POINT('Ctrl Pts',(0.67052008594917,0.324883541256598,-0.302803878949998));
#52004=CARTESIAN_POINT('Ctrl Pts',(0.433783492115795,0.605787405169466,
-0.286946368374054));
#52005=CARTESIAN_POINT('Ctrl Pts',(0.091597991045355,0.739429715509674,
-0.271088857798111));
#52006=CARTESIAN_POINT('Ctrl Pts',(-0.272854196384765,0.693323230190796,
-0.255231347222167));
#52007=CARTESIAN_POINT('Ctrl Pts',(-0.570977895368302,0.478675990529267,
-0.239373836646224));
#52008=CARTESIAN_POINT('Ctrl Pts',(-0.730302032760444,0.147666908672949,
-0.22351632607028));
#52009=CARTESIAN_POINT('Ctrl Pts',(-0.712096020773603,-0.219238781524417,
-0.207658815494337));
#52010=CARTESIAN_POINT('Ctrl Pts',(-0.520786170522117,-0.532849287879404,
-0.191801304918392));
#52011=CARTESIAN_POINT('Ctrl Pts',(-0.202877055975114,-0.716929207912262,
-0.17594379434245));
#52012=CARTESIAN_POINT('Ctrl Pts',(0.164348180649151,-0.726729307650186,
-0.160086283766506));
#52013=CARTESIAN_POINT('Ctrl Pts',(0.491624745145442,-0.559869296311085,
-0.144228773190563));
#52014=CARTESIAN_POINT('Ctrl Pts',(0.699386001600128,-0.256907404440502,
-0.12837126261462));
#52015=CARTESIAN_POINT('Ctrl Pts',(0.737143841528523,0.108501282989102,
-0.112513752038677));
#52016=CARTESIAN_POINT('Ctrl Pts',(0.595686800836177,0.44754428626929,-0.0966562414627327));
#52017=CARTESIAN_POINT('Ctrl Pts',(0.309466356321048,0.67777345379719,-0.0807987308867902));
#52018=CARTESIAN_POINT('Ctrl Pts',(-0.0520692913751179,0.743282925452814,
-0.0649412203108465));
#52019=CARTESIAN_POINT('Ctrl Pts',(-0.284519228009777,0.666428047244306,
-0.0543695465935505));
#52020=CARTESIAN_POINT('Ctrl Pts',(-0.384580808941221,0.602564764849855,
-0.0490837097349027));
#52021=CARTESIAN_POINT('Ctrl Pts',(-0.325579286442189,0.678938089483059,
-5.8309162902651));
#52022=CARTESIAN_POINT('Ctrl Pts',(-0.438323380606369,0.624872568197468,
-5.82563045340645));
#52023=CARTESIAN_POINT('Ctrl Pts',(-0.636245805812322,0.459548685140943,
-5.81505877968916));
#52024=CARTESIAN_POINT('Ctrl Pts',(-0.778481470957093,0.0996097814034236,
-5.79920126911321));
#52025=CARTESIAN_POINT('Ctrl Pts',(-0.731463748292673,-0.284443019088282,
-5.78334375853727));
#52026=CARTESIAN_POINT('Ctrl Pts',(-0.506639730728544,-0.599399518035823,
-5.76748624796132));
#52027=CARTESIAN_POINT('Ctrl Pts',(-0.158652966906228,-0.768622281063247,
-5.75162873738538));
#52028=CARTESIAN_POINT('Ctrl Pts',(0.227899327720991,-0.751012576084023,
-5.73577122680944));
#52029=CARTESIAN_POINT('Ctrl Pts',(0.559052135017169,-0.550831824440762,
-5.7199137162335));
#52030=CARTESIAN_POINT('Ctrl Pts',(0.754303905755431,-0.216752091975169,
-5.70405620565754));
#52031=CARTESIAN_POINT('Ctrl Pts',(0.766191299277441,0.170019868316858,
-5.68819869508161));
#52032=CARTESIAN_POINT('Ctrl Pts',(0.591824271197026,0.515460627536713,
-5.67234118450566));
#52033=CARTESIAN_POINT('Ctrl Pts',(0.273590066173409,0.735597928042492,
-5.65648367392972));
#52034=CARTESIAN_POINT('Ctrl Pts',(-0.111151487059797,0.776917663859421,
-5.64062616335378));
#52035=CARTESIAN_POINT('Ctrl Pts',(-0.468873084526362,0.629375721659158,
-5.62476865277783));
#52036=CARTESIAN_POINT('Ctrl Pts',(-0.712615799746851,0.328838061265476,
-5.60891114220189));
#52037=CARTESIAN_POINT('Ctrl Pts',(-0.783127928281117,-0.0516371854324633,
-5.59305363162595));
#52038=CARTESIAN_POINT('Ctrl Pts',(-0.663268602687365,-0.419559905984642,
-5.57719612105));
#52039=CARTESIAN_POINT('Ctrl Pts',(-0.382174559347619,-0.68549132513945,
-5.56133861047406));
#52040=CARTESIAN_POINT('Ctrl Pts',(-0.00817726953152785,-0.784785884905202,
-5.54548109989812));
#52041=CARTESIAN_POINT('Ctrl Pts',(0.367807842272825,-0.693305951887881,
-5.52962358932217));
#52042=CARTESIAN_POINT('Ctrl Pts',(0.654382128491452,-0.433289489945468,
-5.51376607874623));
#52043=CARTESIAN_POINT('Ctrl Pts',(0.781881921134958,-0.067944194012094,
-5.49790856817029));
#52044=CARTESIAN_POINT('Ctrl Pts',(0.719313150927466,0.313917732803588,
-5.48205105759434));
#52045=CARTESIAN_POINT('Ctrl Pts',(0.481885731221726,0.61946904213411,-5.4661935470184));
#52046=CARTESIAN_POINT('Ctrl Pts',(0.127316162674759,0.774432919497292,
-5.45033603644246));
#52047=CARTESIAN_POINT('Ctrl Pts',(-0.258202836220851,0.741139020338087,
-5.43447852586652));
#52048=CARTESIAN_POINT('Ctrl Pts',(-0.580955014875615,0.527680796298617,
-5.41862101529056));
#52049=CARTESIAN_POINT('Ctrl Pts',(-0.762482180195239,0.185948049138887,
-5.40276350471463));
#52050=CARTESIAN_POINT('Ctrl Pts',(-0.758656687723272,-0.200987020144955,
-5.38690599413869));
#52051=CARTESIAN_POINT('Ctrl Pts',(-0.570408480761624,-0.539063926792038,
-5.37104848356273));
#52052=CARTESIAN_POINT('Ctrl Pts',(-0.243499029403163,-0.746099172210769,
-5.3551909729868));
#52053=CARTESIAN_POINT('Ctrl Pts',(0.142602877126142,-0.771764323824862,
-5.33933346241085));
#52054=CARTESIAN_POINT('Ctrl Pts',(0.49403928855179,-0.609820410826756,
-5.3234759518349));
#52055=CARTESIAN_POINT('Ctrl Pts',(0.725379129112798,-0.299634562661213,
-5.30761844125897));
#52056=CARTESIAN_POINT('Ctrl Pts',(0.780385734641799,0.0833897911089845,
-5.29176093068301));
#52057=CARTESIAN_POINT('Ctrl Pts',(0.645687487026613,0.446142825999577,
-5.27590342010709));
#52058=CARTESIAN_POINT('Ctrl Pts',(0.354028336019651,0.700442495418987,
-5.26004590953113));
#52059=CARTESIAN_POINT('Ctrl Pts',(-0.0236919646369996,0.784470804367675,
-5.2441883989552));
#52060=CARTESIAN_POINT('Ctrl Pts',(-0.39565295874479,0.677801215940276,
-5.22833088837924));
#52061=CARTESIAN_POINT('Ctrl Pts',(-0.671434226464838,0.406364161344466,
-5.21247337780331));
#52062=CARTESIAN_POINT('Ctrl Pts',(-0.783995786707833,0.0361435819750997,
-5.19661586722736));
#52063=CARTESIAN_POINT('Ctrl Pts',(-0.705974922156322,-0.342863181721224,
-5.18075835665142));
#52064=CARTESIAN_POINT('Ctrl Pts',(-0.45633781324506,-0.638522945786869,
-5.16490084607547));
#52065=CARTESIAN_POINT('Ctrl Pts',(-0.0957690278526387,-0.778963442914869,
-5.14904333549954));
#52066=CARTESIAN_POINT('Ctrl Pts',(0.288080359116754,-0.730044833407365,
-5.13318582492359));
#52067=CARTESIAN_POINT('Ctrl Pts',(0.601899964922791,-0.503658797520275,
-5.11732831434764));
#52068=CARTESIAN_POINT('Ctrl Pts',(0.769403025737667,-0.154837773425435,
-5.1014708037717));
#52069=CARTESIAN_POINT('Ctrl Pts',(0.749871032569584,0.231622940588045,
-5.08561329319576));
#52070=CARTESIAN_POINT('Ctrl Pts',(0.548052039785859,0.5617781713276,-5.06975578261982));
#52071=CARTESIAN_POINT('Ctrl Pts',(0.213006455192798,0.755370109376738,
-5.05389827204387));
#52072=CARTESIAN_POINT('Ctrl Pts',(-0.173819110129491,0.765338270993563,
-5.03804076146793));
#52073=CARTESIAN_POINT('Ctrl Pts',(-0.518390790870064,0.589259484467356,
-5.02218325089199));
#52074=CARTESIAN_POINT('Ctrl Pts',(-0.7369462664343,0.269936941677441,-5.00632574031604));
#52075=CARTESIAN_POINT('Ctrl Pts',(-0.776356638438626,-0.115004878356971,
-4.9904682297401));
#52076=CARTESIAN_POINT('Ctrl Pts',(-0.627041594863537,-0.471990032103027,
-4.97461071916415));
#52077=CARTESIAN_POINT('Ctrl Pts',(-0.32529829896591,-0.714238593737072,
-4.95875320858822));
#52078=CARTESIAN_POINT('Ctrl Pts',(0.055522129295891,-0.7828620857163,-4.94289569801226));
#52079=CARTESIAN_POINT('Ctrl Pts',(0.422845620188429,-0.6611787455606,-4.92703818743633));
#52080=CARTESIAN_POINT('Ctrl Pts',(0.687379089788056,-0.378768714409952,
-4.91118067686037));
#52081=CARTESIAN_POINT('Ctrl Pts',(0.784816797004884,-0.00428336697262591,
-4.89532316628444));
#52082=CARTESIAN_POINT('Ctrl Pts',(0.691472499103114,0.371243228999155,
-4.87946565570849));
#52083=CARTESIAN_POINT('Ctrl Pts',(0.43003736730647,0.656523887466211,-4.86360814513256));
#52084=CARTESIAN_POINT('Ctrl Pts',(0.0640639642549887,0.782209409670812,
-4.8477506345566));
#52085=CARTESIAN_POINT('Ctrl Pts',(-0.317482820511887,0.71774675950048,
-4.83189312398067));
#52086=CARTESIAN_POINT('Ctrl Pts',(-0.621852346434259,0.47880623568186,
-4.81603561340471));
#52087=CARTESIAN_POINT('Ctrl Pts',(-0.775055080319058,0.123472161094084,
-4.80017810282878));
#52088=CARTESIAN_POINT('Ctrl Pts',(-0.739848795863616,-0.261876901143998,
-4.78432059225283));
#52089=CARTESIAN_POINT('Ctrl Pts',(-0.524791828677996,-0.583566010530454,
-4.76846308167689));
#52090=CARTESIAN_POINT('Ctrl Pts',(-0.182162620776919,-0.763395396688577,
-4.75260557110095));
#52091=CARTESIAN_POINT('Ctrl Pts',(0.204748705170189,-0.757650130221566,
-4.736748060525));
#52092=CARTESIAN_POINT('Ctrl Pts',(0.541887436204854,-0.567726834469673,
-4.72089054994906));
#52093=CARTESIAN_POINT('Ctrl Pts',(0.747298135904977,-0.239794178758729,
-4.70503303937311));
#52094=CARTESIAN_POINT('Ctrl Pts',(0.771047284357168,0.146430315778737,
-4.68917552879717));
#52095=CARTESIAN_POINT('Ctrl Pts',(0.607361674134095,0.497058898810449,
-4.67331801822123));
#52096=CARTESIAN_POINT('Ctrl Pts',(0.296031825834439,0.726856870495665,
-4.65746050764529));
#52097=CARTESIAN_POINT('Ctrl Pts',(-0.0872607346894568,0.77996238132046,
-4.64160299706934));
#52098=CARTESIAN_POINT('Ctrl Pts',(-0.449340984269311,0.643465952439997,
-4.6257454864934));
#52099=CARTESIAN_POINT('Ctrl Pts',(-0.702190424457694,0.350548655529511,
-4.60988797591746));
#52100=CARTESIAN_POINT('Ctrl Pts',(-0.784343598123281,-0.0275839115545715,
-4.59403046534151));
#52101=CARTESIAN_POINT('Ctrl Pts',(-0.675829797122982,-0.399011074300369,
-4.57817295476558));
#52102=CARTESIAN_POINT('Ctrl Pts',(-0.403027764390032,-0.673442182540117,
-4.56231544418962));
#52103=CARTESIAN_POINT('Ctrl Pts',(-0.0322532554024553,-0.784165466983575,
-4.54645793361368));
#52104=CARTESIAN_POINT('Ctrl Pts',(0.346361734014141,-0.704265078861889,
-4.53060042303774));
#52105=CARTESIAN_POINT('Ctrl Pts',(0.64077925675603,-0.453164094125754,
-4.5147429124618));
#52106=CARTESIAN_POINT('Ctrl Pts',(0.779429023368258,-0.0919029358879742,
-4.49888540188585));
#52107=CARTESIAN_POINT('Ctrl Pts',(0.728606504864627,0.291699011247172,
-4.48302789130991));
#52108=CARTESIAN_POINT('Ctrl Pts',(0.500666204897841,0.604391514969245,
-4.46717038073396));
#52109=CARTESIAN_POINT('Ctrl Pts',(0.15101838945731,0.7701617999741,-4.45131287015803));
#52110=CARTESIAN_POINT('Ctrl Pts',(-0.235340657522096,0.748712579706453,
-4.43545535958207));
#52111=CARTESIAN_POINT('Ctrl Pts',(-0.564490477202418,0.545257969443283,
-4.41959784900614));
#52112=CARTESIAN_POINT('Ctrl Pts',(-0.756417666681617,0.209255981098659,
-4.40374033843019));
#52113=CARTESIAN_POINT('Ctrl Pts',(-0.7644664278354,-0.177614280974837,
-4.38788282785425));
#52114=CARTESIAN_POINT('Ctrl Pts',(-0.586680178188085,-0.521308086082331,
-4.3720253172783));
#52115=CARTESIAN_POINT('Ctrl Pts',(-0.266277178765265,-0.738276517412301,
-4.35616780670236));
#52116=CARTESIAN_POINT('Ctrl Pts',(0.118855441985783,-0.775776472963695,
-4.34031029612641));
#52117=CARTESIAN_POINT('Ctrl Pts',(0.475095358569639,-0.624692046018845,
-4.32445278555048));
#52118=CARTESIAN_POINT('Ctrl Pts',(0.715843805709462,-0.321750521244362,
-4.30859527497453));
#52119=CARTESIAN_POINT('Ctrl Pts',(0.782576970395889,0.0594057025850026,
-4.29273776439859));
#52120=CARTESIAN_POINT('Ctrl Pts',(0.659072611953929,0.426120926810512,
-4.27688025382264));
#52121=CARTESIAN_POINT('Ctrl Pts',(0.375353544923698,0.689249931742353,
-4.2610227432467));
#52122=CARTESIAN_POINT('Ctrl Pts',(0.000389359029796799,0.784828389199302,
-4.24516523267075));
#52123=CARTESIAN_POINT('Ctrl Pts',(-0.374669476592169,0.689622023577971,
-4.22930772209482));
#52124=CARTESIAN_POINT('Ctrl Pts',(-0.658649484296868,0.426774658255496,
-4.21345021151887));
#52125=CARTESIAN_POINT('Ctrl Pts',(-0.782517641995249,0.0601821573211011,
-4.19759270094293));
#52126=CARTESIAN_POINT('Ctrl Pts',(-0.71616269877343,-0.321040092479401,
-4.18173519036698));
#52127=CARTESIAN_POINT('Ctrl Pts',(-0.47571495302169,-0.624220342159077,
-4.16587767979104));
#52128=CARTESIAN_POINT('Ctrl Pts',(-0.119625119907983,-0.775658161035277,
-4.15002016921509));
#52129=CARTESIAN_POINT('Ctrl Pts',(0.26554451925179,-0.738540357996068,
-4.13416265863915));
#52130=CARTESIAN_POINT('Ctrl Pts',(0.586162640115255,-0.521889941871598,
-4.11830514806321));
#52131=CARTESIAN_POINT('Ctrl Pts',(0.764289820120199,-0.178372707986,-4.10244763748727));
#52132=CARTESIAN_POINT('Ctrl Pts',(0.756624921093796,0.208505349747752,
-4.08659012691132));
#52133=CARTESIAN_POINT('Ctrl Pts',(0.565031212031903,0.544697605578897,
-4.07073261633538));
#52134=CARTESIAN_POINT('Ctrl Pts',(0.236083424926029,0.748478702815799,
-4.05487510575943));
#52135=CARTESIAN_POINT('Ctrl Pts',(-0.150254149649408,0.770311263455727,
-4.0390175951835));
#52136=CARTESIAN_POINT('Ctrl Pts',(-0.500066272607472,0.604887985575921,
-4.02316008460754));
#52137=CARTESIAN_POINT('Ctrl Pts',(-0.728316718312543,0.292421801376152,
-4.00730257403161));
#52138=CARTESIAN_POINT('Ctrl Pts',(-0.779519827096005,-0.0911295301087435,
-3.99144506345566));
#52139=CARTESIAN_POINT('Ctrl Pts',(-0.641228577182465,-0.452528080784138,
-3.97558755287972));
#52140=CARTESIAN_POINT('Ctrl Pts',(-0.347060345327305,-0.703921067162304,
-3.95973004230377));
#52141=CARTESIAN_POINT('Ctrl Pts',(0.0314751794188634,-0.784197083120166,
-3.94387253172783));
#52142=CARTESIAN_POINT('Ctrl Pts',(0.402359367109157,-0.673841740910389,
-3.92801502115189));
#52143=CARTESIAN_POINT('Ctrl Pts',(0.675433559997749,-0.399681445807019,
-3.91215751057594));
#52144=CARTESIAN_POINT('Ctrl Pts',(0.78431584288578,-0.0283621348278897,
-3.8963));
#52145=CARTESIAN_POINT('Ctrl Pts',(0.702537898160078,0.349851759667497,
-3.88044248942406));
#52146=CARTESIAN_POINT('Ctrl Pts',(0.449979219135252,0.643019793194622,
-3.86458497884811));
#52147=CARTESIAN_POINT('Ctrl Pts',(0.0880345814816758,0.779875416048597,
-3.84872746827217));
#52148=CARTESIAN_POINT('Ctrl Pts',(-0.295310482410159,0.727150239683866,
-3.83286995769623));
#52149=CARTESIAN_POINT('Ctrl Pts',(-0.606868186268723,0.497661287010088,
-3.81701244712028));
#52150=CARTESIAN_POINT('Ctrl Pts',(-0.770901614575481,0.147195287759293,
-3.80115493654434));
#52151=CARTESIAN_POINT('Ctrl Pts',(-0.747535695239384,-0.239052580903443,
-3.7852974259684));
#52152=CARTESIAN_POINT('Ctrl Pts',(-0.542450476087375,-0.567188886603224,
-3.76943991539245));
#52153=CARTESIAN_POINT('Ctrl Pts',(-0.205500355597327,-0.757446602700809,
-3.75358240481651));
#52154=CARTESIAN_POINT('Ctrl Pts',(0.181405079359823,-0.763575765249318,
-3.73772489424057));
#52155=CARTESIAN_POINT('Ctrl Pts',(0.524212547873029,-0.584086429174735,
-3.72186738366462));
#52156=CARTESIAN_POINT('Ctrl Pts',(0.739588593698525,-0.262610860713459,
-3.70600987308868));
#52157=CARTESIAN_POINT('Ctrl Pts',(0.775177209633211,0.122703079663451,
-3.69015236251273));
#52158=CARTESIAN_POINT('Ctrl Pts',(0.62232711867419,0.478188989267114,-3.67429485193679));
#52159=CARTESIAN_POINT('Ctrl Pts',(0.318194822755437,0.717431395232506,
-3.65843734136085));
#52160=CARTESIAN_POINT('Ctrl Pts',(-0.0632878134405744,0.782272589807117,
-3.6425798307849));
#52161=CARTESIAN_POINT('Ctrl Pts',(-0.429385743302777,0.656950253475823,
-3.62672232020896));
#52162=CARTESIAN_POINT('Ctrl Pts',(-0.691103805928104,0.37192913508532,
-3.61086480963302));
#52163=CARTESIAN_POINT('Ctrl Pts',(-0.784820660700543,-0.00350465849816745,
-3.59500729905707));
#52164=CARTESIAN_POINT('Ctrl Pts',(-0.687754571124228,-0.378086500673265,
-3.57914978848113));
#52165=CARTESIAN_POINT('Ctrl Pts',(-0.423501442981327,-0.660758866672525,
-3.56329227790519));
#52166=CARTESIAN_POINT('Ctrl Pts',(-0.0562988688391297,-0.782806610511855,
-3.54743476732924));
#52167=CARTESIAN_POINT('Ctrl Pts',(0.324589461168678,-0.714561007746612,
-3.5315772567533));
#52168=CARTESIAN_POINT('Ctrl Pts',(0.626572970996214,-0.472611959339373,
-3.51571974617736));
#52169=CARTESIAN_POINT('Ctrl Pts',(0.776242146808514,-0.115775133823011,
-3.49986223560142));
#52170=CARTESIAN_POINT('Ctrl Pts',(0.737213738941585,0.269205600256372,
-3.48400472502547));
#52171=CARTESIAN_POINT('Ctrl Pts',(0.518975207319653,0.588744839706599,
-3.46814721444953));
#52172=CARTESIAN_POINT('Ctrl Pts',(0.174578404063956,0.765165428471587,
-3.45228970387358));
#52173=CARTESIAN_POINT('Ctrl Pts',(-0.212256861396975,0.7555810855782,-3.43643219329765));
#52174=CARTESIAN_POINT('Ctrl Pts',(-0.5474943657345,0.562321679808455,-3.42057468272169));
#52175=CARTESIAN_POINT('Ctrl Pts',(-0.749640843880201,0.232366859255372,
-3.40471717214576));
#52176=CARTESIAN_POINT('Ctrl Pts',(-0.769556279239784,-0.15407428460403,
-3.38885966156981));
#52177=CARTESIAN_POINT('Ctrl Pts',(-0.602399406048799,-0.503061335908134,
-3.37300215099387));
#52178=CARTESIAN_POINT('Ctrl Pts',(-0.288804578157005,-0.729758636625274,
-3.35714464041792));
#52179=CARTESIAN_POINT('Ctrl Pts',(0.0949960821258639,-0.779058082863121,
-3.34128712984198));
#52180=CARTESIAN_POINT('Ctrl Pts',(0.455704037084961,-0.638975416333128,
-3.32542961926604));
#52181=CARTESIAN_POINT('Ctrl Pts',(0.705634380928318,-0.343563491287323,
-3.3095721086901));
#52182=CARTESIAN_POINT('Ctrl Pts',(0.784031262965194,0.0353656724356925,
-3.29371459811415));
#52183=CARTESIAN_POINT('Ctrl Pts',(0.671837096243931,0.405697754743786,
-3.27785708753821));
#52184=CARTESIAN_POINT('Ctrl Pts',(0.396325287974185,0.67740830981455,-3.26199957696226));
#52185=CARTESIAN_POINT('Ctrl Pts',(0.024470316041941,0.784446910712531,
-3.24614206638632));
#52186=CARTESIAN_POINT('Ctrl Pts',(-0.353333172764794,0.700793422570154,
-3.23028455581038));
#52187=CARTESIAN_POINT('Ctrl Pts',(-0.645244499945733,0.446783266677934,
-3.21442704523443));
#52188=CARTESIAN_POINT('Ctrl Pts',(-0.780302609966712,0.084164059863832,
-3.19856953465849));
#52189=CARTESIAN_POINT('Ctrl Pts',(-0.72567607371502,-0.298914683699512,
-3.18271202408255));
#52190=CARTESIAN_POINT('Ctrl Pts',(-0.494644117831261,-0.609329917851207,
-3.1668545135066));
#52191=CARTESIAN_POINT('Ctrl Pts',(-0.143368562447453,-0.771622451329261,
-3.15099700293066));
#52192=CARTESIAN_POINT('Ctrl Pts',(0.242758619352965,-0.746340408140593,
-3.13513949235471));
#52193=CARTESIAN_POINT('Ctrl Pts',(0.569873333101313,-0.539629628832245,
-3.11928198177877));
#52194=CARTESIAN_POINT('Ctrl Pts',(0.75845689210424,-0.201739671143779,
-3.10342447120283));
#52195=CARTESIAN_POINT('Ctrl Pts',(0.762666305161411,0.185191411963582,
-3.08756696062689));
#52196=CARTESIAN_POINT('Ctrl Pts',(0.581478301279538,0.527104104740881,
-3.07170945005094));
#52197=CARTESIAN_POINT('Ctrl Pts',(0.258938077778477,0.740882462992621,
-3.055851939475));
#52198=CARTESIAN_POINT('Ctrl Pts',(-0.126547696669843,0.774558863199681,
-3.03999442889905));
#52199=CARTESIAN_POINT('Ctrl Pts',(-0.481270848037274,0.619946871048728,
-3.02413691832312));
#52200=CARTESIAN_POINT('Ctrl Pts',(-0.719001323223353,0.314631291032365,
-3.00827940774716));
#52201=CARTESIAN_POINT('Ctrl Pts',(-0.781948951443148,-0.0671683662938689,
-2.99242189717123));
#52202=CARTESIAN_POINT('Ctrl Pts',(-0.654811722373912,-0.432639989292871,
-2.97656438659528));
#52203=CARTESIAN_POINT('Ctrl Pts',(-0.368495569196001,-0.692940666707143,
-2.96070687601934));
#52204=CARTESIAN_POINT('Ctrl Pts',(0.00739858974940715,-0.784793611698863,
-2.94484936544339));
#52205=CARTESIAN_POINT('Ctrl Pts',(0.381494217123079,-0.685870187714319,
-2.92899185486745));
#52206=CARTESIAN_POINT('Ctrl Pts',(0.662851982664983,-0.42021780206308,
-2.91313434429151));
#52207=CARTESIAN_POINT('Ctrl Pts',(0.783076308106886,-0.0524141944068109,
-2.89727683371557));
#52208=CARTESIAN_POINT('Ctrl Pts',(0.712941725850017,0.328130839202329,
-2.88141932313962));
#52209=CARTESIAN_POINT('Ctrl Pts',(0.469497331023564,0.628910175029293,
-2.86556181256368));
#52210=CARTESIAN_POINT('Ctrl Pts',(0.11192229761708,0.776807023262366,-2.84970430198773));
#52211=CARTESIAN_POINT('Ctrl Pts',(-0.272860054030235,0.735868971358516,
-2.83384679141179));
#52212=CARTESIAN_POINT('Ctrl Pts',(-0.591312545736583,0.516047696776321,
-2.81798928083585));
#52213=CARTESIAN_POINT('Ctrl Pts',(-0.766022200187245,0.170779802417963,
-2.80213177025991));
#52214=CARTESIAN_POINT('Ctrl Pts',(-0.754518649371647,-0.216003147764127,
-2.78627425968396));
#52215=CARTESIAN_POINT('Ctrl Pts',(-0.559598304501882,-0.550277647821756,
-2.77041674910802));
#52216=CARTESIAN_POINT('Ctrl Pts',(-0.228644573240195,-0.750784530488898,
-2.75455923853207));
#52217=CARTESIAN_POINT('Ctrl Pts',(0.157890626599538,-0.768782350295342,
-2.73870172795613));
#52218=CARTESIAN_POINT('Ctrl Pts',(0.506044014980788,-0.599895996815906,
-2.72284421738018));
#52219=CARTESIAN_POINT('Ctrl Pts',(0.73118258993712,-0.285180245224791,
-2.70698670680425));
#52220=CARTESIAN_POINT('Ctrl Pts',(0.778577159988897,0.0988602955551302,
-2.6911291962283));
#52221=CARTESIAN_POINT('Ctrl Pts',(0.636706525359668,0.458868774986972,
-2.67527168565236));
#52222=CARTESIAN_POINT('Ctrl Pts',(0.340058179494149,0.707330323577854,
-2.65941417507641));
#52223=CARTESIAN_POINT('Ctrl Pts',(-0.039255294829966,0.783846141740481,
-2.64355666450047));
#52224=CARTESIAN_POINT('Ctrl Pts',(-0.409026155020739,0.669815912473402,
-2.62769915392453));
#52225=CARTESIAN_POINT('Ctrl Pts',(-0.679366383376654,0.392959373512518,
-2.61184164334858));
#52226=CARTESIAN_POINT('Ctrl Pts',(-0.784558667237237,0.0205778948523656,
-2.59598413277264));
#52227=CARTESIAN_POINT('Ctrl Pts',(-0.699031695037147,-0.356805887601535,
-2.5801266221967));
#52228=CARTESIAN_POINT('Ctrl Pts',(-0.443576315430907,-0.647453322242124,
-2.56426911162075));
#52229=CARTESIAN_POINT('Ctrl Pts',(-0.0802914663179188,-0.780710594606057,
-2.54841160104481));
#52230=CARTESIAN_POINT('Ctrl Pts',(0.302511526387946,-0.724184043248715,
-2.53255409046886));
#52231=CARTESIAN_POINT('Ctrl Pts',(0.611776649114439,-0.49161477163724,
-2.51669657989292));
#52232=CARTESIAN_POINT('Ctrl Pts',(0.772324292490064,-0.139538307727111,
-2.50083906931698));
#52233=CARTESIAN_POINT('Ctrl Pts',(0.745126747835348,0.246458681636383,
-2.48498155874104));
#52234=CARTESIAN_POINT('Ctrl Pts',(0.536795497120767,0.572543750611684,
-2.46912404816509));
#52235=CARTESIAN_POINT('Ctrl Pts',(0.197974020317544,0.75944851002088,-2.45326653758915));
#52236=CARTESIAN_POINT('Ctrl Pts',(-0.188973185575212,0.761738069960523,
-2.4374090270132));
#52237=CARTESIAN_POINT('Ctrl Pts',(-0.52998268550235,0.578855858708663,
-2.42155151643726));
#52238=CARTESIAN_POINT('Ctrl Pts',(-0.742158093442481,0.255258920375855,
-2.40569400586132));
#52239=CARTESIAN_POINT('Ctrl Pts',(-0.773921448885386,-0.130389198359262,
-2.38983649528537));
#52240=CARTESIAN_POINT('Ctrl Pts',(-0.617551361738728,-0.484340859011778,
-2.37397898470943));
#52241=CARTESIAN_POINT('Ctrl Pts',(-0.311060013801192,-0.720553551033945,
-2.35812147413349));
#52242=CARTESIAN_POINT('Ctrl Pts',(0.0710472656144783,-0.781606063271219,
-2.34226396355755));
#52243=CARTESIAN_POINT('Ctrl Pts',(0.435883584668632,-0.65265707129399,
-2.3264064529816));
#52244=CARTESIAN_POINT('Ctrl Pts',(0.694760468860123,-0.365052931782348,
-2.31054894240566));
#52245=CARTESIAN_POINT('Ctrl Pts',(0.784747242860147,0.0112923388641639,
-2.29469143182971));
#52246=CARTESIAN_POINT('Ctrl Pts',(0.683968919737491,0.384892542051355,
-2.27883392125377));
#52247=CARTESIAN_POINT('Ctrl Pts',(0.416923816336558,0.664928780746467,
-2.26297641067783));
#52248=CARTESIAN_POINT('Ctrl Pts',(0.0485282296560387,0.783326728140994,
-2.24711890010188));
#52249=CARTESIAN_POINT('Ctrl Pts',(-0.331664139399642,0.711304892946703,
-2.23126138952594));
#52250=CARTESIAN_POINT('Ctrl Pts',(-0.631231896721636,0.466371144749363,
-2.21540387895));
#52251=CARTESIAN_POINT('Ctrl Pts',(-0.777352776490858,0.10806670613829,
-2.19954636837406));
#52252=CARTESIAN_POINT('Ctrl Pts',(-0.734506088351986,-0.276507790609034,
-2.18368885779811));
#52253=CARTESIAN_POINT('Ctrl Pts',(-0.513107482310247,-0.593865694994133,
-2.16783134722217));
#52254=CARTESIAN_POINT('Ctrl Pts',(-0.166976996560925,-0.766860114175407,
-2.15197383664622));
#52255=CARTESIAN_POINT('Ctrl Pts',(0.219744116624184,-0.753437638628893,
-2.13611632607028));
#52256=CARTESIAN_POINT('Ctrl Pts',(0.553047383322612,-0.556861153155467,
-2.12025881549434));
#52257=CARTESIAN_POINT('Ctrl Pts',(0.751909734486935,-0.224916658514685,
-2.10440130491839));
#52258=CARTESIAN_POINT('Ctrl Pts',(0.767989495674767,0.161703081686291,
-2.08854379434245));
#52259=CARTESIAN_POINT('Ctrl Pts',(0.597377819505481,0.509014236398652,
-2.07268628376651));
#52260=CARTESIAN_POINT('Ctrl Pts',(0.281548891802369,0.732588543193575,
-2.05682877319056));
#52261=CARTESIAN_POINT('Ctrl Pts',(-0.102722075268358,0.778077070312567,
-2.04097126261462));
#52262=CARTESIAN_POINT('Ctrl Pts',(-0.462022216581493,0.634421960117041,
-2.02511375203867));
#52263=CARTESIAN_POINT('Ctrl Pts',(-0.709008853360644,0.336544496240616,
-2.00925624146273));
#52264=CARTESIAN_POINT('Ctrl Pts',(-0.783641724003292,-0.0431439508480003,
-1.99339873088679));
#52265=CARTESIAN_POINT('Ctrl Pts',(-0.667778239355765,-0.412344486002345,
-1.97754122031085));
#52266=CARTESIAN_POINT('Ctrl Pts',(-0.389583785283206,-0.681307732480728,
-1.9616837097349));
#52267=CARTESIAN_POINT('Ctrl Pts',(-0.0166849670817576,-0.784651109708708,
-1.94582619915896));
#52268=CARTESIAN_POINT('Ctrl Pts',(0.360269818687344,-0.697252758930801,
-1.92996868858301));
#52269=CARTESIAN_POINT('Ctrl Pts',(0.649646205707602,-0.44035844434204,
-1.91411117800707));
#52270=CARTESIAN_POINT('Ctrl Pts',(0.781099359922979,-0.076416896178388,
-1.89825366743113));
#52271=CARTESIAN_POINT('Ctrl Pts',(0.722674185015349,0.306100921929396,
-1.88239615685518));
#52272=CARTESIAN_POINT('Ctrl Pts',(0.488573323003616,0.614208319825472,
-1.86653864627924));
#52273=CARTESIAN_POINT('Ctrl Pts',(0.1357046178904,0.773007120780168,-1.8506811357033));
#52274=CARTESIAN_POINT('Ctrl Pts',(-0.250152676666605,0.743894744201193,
-1.83482362512736));
#52275=CARTESIAN_POINT('Ctrl Pts',(-0.575200073394752,0.533948150722799,
-1.81896611455141));
#52276=CARTESIAN_POINT('Ctrl Pts',(-0.760421432039351,0.194203495820362,
-1.80310860397547));
#52277=CARTESIAN_POINT('Ctrl Pts',(-0.76079108249769,-0.192750307096041,
-1.78725109339952));
#52278=CARTESIAN_POINT('Ctrl Pts',(-0.576219166020697,-0.532848219293294,
-1.77139358282358));
#52279=CARTESIAN_POINT('Ctrl Pts',(-0.251573479078132,-0.743415453644965,
-1.75553607224764));
#52280=CARTESIAN_POINT('Ctrl Pts',(0.134227490162612,-0.773264982382023,
-1.73967856167169));
#52281=CARTESIAN_POINT('Ctrl Pts',(0.487398946613895,-0.615140649716218,
-1.72382105109575));
#52282=CARTESIAN_POINT('Ctrl Pts',(0.722088040451945,-0.307481078978686,
-1.70796354051981));
#52283=CARTESIAN_POINT('Ctrl Pts',(0.78124393373246,0.0749244159126821,
-1.69210602994387));
#52284=CARTESIAN_POINT('Ctrl Pts',(0.650486353278686,0.439116449580088,
-1.67624851936792));
#52285=CARTESIAN_POINT('Ctrl Pts',(0.361601307594298,0.696563167587635,
-1.66039100879198));
#52286=CARTESIAN_POINT('Ctrl Pts',(-0.0151858099871515,0.78468155532589,
-1.64453349821603));
#52287=CARTESIAN_POINT('Ctrl Pts',(-0.388281391799038,0.682050813998657,
-1.62867598764009));
#52288=CARTESIAN_POINT('Ctrl Pts',(-0.66698920979093,0.413619566892203,
-1.61281847706415));
#52289=CARTESIAN_POINT('Ctrl Pts',(-0.783557864449414,0.0446410702504095,
-1.5969609664882));
#52290=CARTESIAN_POINT('Ctrl Pts',(-0.70965054933176,-0.335189274778826,
-1.58110345591226));
#52291=CARTESIAN_POINT('Ctrl Pts',(-0.463233477476344,-0.633538078917755,
-1.56524594533632));
#52292=CARTESIAN_POINT('Ctrl Pts',(-0.104208454302516,-0.777879393058787,
-1.54938843476037));
#52293=CARTESIAN_POINT('Ctrl Pts',(0.280148720193781,-0.733125123473075,
-1.53353092418443));
#52294=CARTESIAN_POINT('Ctrl Pts',(0.596404224626504,-0.510154636302842,
-1.51767341360849));
#52295=CARTESIAN_POINT('Ctrl Pts',(0.767679149808526,-0.163170080109321,
-1.50181590303254));
#52296=CARTESIAN_POINT('Ctrl Pts',(0.752338079961976,0.223479675882952,
-1.4859583924566));
#52297=CARTESIAN_POINT('Ctrl Pts',(0.554110293151698,0.555803504052435,
-1.47010088188065));
#52298=CARTESIAN_POINT('Ctrl Pts',(0.221183206851683,0.753016428174334,
-1.45424337130472));
#52299=CARTESIAN_POINT('Ctrl Pts',(-0.165511556010258,0.767177734896347,
-1.43838586072877));
#52300=CARTESIAN_POINT('Ctrl Pts',(-0.511971927041593,0.594844936109356,
-1.42252835015283));
#52301=CARTESIAN_POINT('Ctrl Pts',(-0.733976461783252,0.277910607285441,
-1.40667083957688));
#52302=CARTESIAN_POINT('Ctrl Pts',(-0.777557826145205,-0.106581326197277,
-1.39081332900094));
#52303=CARTESIAN_POINT('Ctrl Pts',(-0.632121776846072,-0.465164284237934,
-1.37495581842499));
#52304=CARTESIAN_POINT('Ctrl Pts',(-0.33302252802565,-0.71066992895509,
-1.35909830784906));
#52305=CARTESIAN_POINT('Ctrl Pts',(0.0470315447598909,-0.783418014785927,
-1.34324079727311));
#52306=CARTESIAN_POINT('Ctrl Pts',(0.415652665998827,-0.665724127053912,
-1.32738328669717));
#52307=CARTESIAN_POINT('Ctrl Pts',(0.68323230933518,-0.386198606385552,
-1.31152577612122));
#52308=CARTESIAN_POINT('Ctrl Pts',(0.784724235851218,-0.0127916285651174,
-1.29566826554528));
#52309=CARTESIAN_POINT('Ctrl Pts',(0.695456658044464,0.363724880748143,
-1.27981075496933));
#52310=CARTESIAN_POINT('Ctrl Pts',(0.437129732627986,0.65182309635837,-1.26395324439339));
#52311=CARTESIAN_POINT('Ctrl Pts',(0.0725404448283483,0.781468896346956,
-1.24809573381745));
#52312=CARTESIAN_POINT('Ctrl Pts',(-0.309682781961072,0.721146536184204,
-1.23223822324151));
#52313=CARTESIAN_POINT('Ctrl Pts',(-0.616624870122073,0.485519846803979,
-1.21638071266556));
#52314=CARTESIAN_POINT('Ctrl Pts',(-0.77367091938988,0.131867587314102,
-1.20052320208962));
#52315=CARTESIAN_POINT('Ctrl Pts',(-0.742644427567277,-0.253840513505818,
-1.18466569151368));
#52316=CARTESIAN_POINT('Ctrl Pts',(-0.531087659733577,-0.577842236057851,
-1.16880818093773));
#52317=CARTESIAN_POINT('Ctrl Pts',(-0.190428190474026,-0.761375634208512,
-1.15295067036179));
#52318=CARTESIAN_POINT('Ctrl Pts',(0.19652268354188,-0.759825366085605,
-1.13709315978584));
#52319=CARTESIAN_POINT('Ctrl Pts',(0.535700635570782,-0.573568288125039,
-1.1212356492099));
#52320=CARTESIAN_POINT('Ctrl Pts',(0.744654512646728,-0.247881844612484,
-1.10537813863396));
#52321=CARTESIAN_POINT('Ctrl Pts',(0.772589479850304,0.138062477589907,
-1.08952062805802));
#52322=CARTESIAN_POINT('Ctrl Pts',(0.612714794327425,0.490445035560485,
-1.07366311748207));
#52323=CARTESIAN_POINT('Ctrl Pts',(0.303894574670057,0.723604753701724,
-1.05780560690613));
#52324=CARTESIAN_POINT('Ctrl Pts',(-0.0787997217418853,0.780862571741677,
-1.04194809633018));
#52325=CARTESIAN_POINT('Ctrl Pts',(-0.442338504441484,0.648299621766123,
-1.02609058575424));
#52326=CARTESIAN_POINT('Ctrl Pts',(-0.698348718511349,0.358140781602964,
-1.0102330751783));
#52327=CARTESIAN_POINT('Ctrl Pts',(-0.784596550713174,-0.0190789072699962,
-0.994375564602355));
#52328=CARTESIAN_POINT('Ctrl Pts',(-0.680115917717199,-0.391660682940369,
-0.978518054026408));
#52329=CARTESIAN_POINT('Ctrl Pts',(-0.410305135073127,-0.669033219075294,
-0.962660543450468));
#52330=CARTESIAN_POINT('Ctrl Pts',(-0.0407528118829727,-0.783769711342085,
-0.946803032874522));
#52331=CARTESIAN_POINT('Ctrl Pts',(0.338706158559024,-0.707978735731387,
-0.93094552229858));
#52332=CARTESIAN_POINT('Ctrl Pts',(0.635828664844656,-0.460084406446779,
-0.915088011722638));
#52333=CARTESIAN_POINT('Ctrl Pts',(0.778386860002041,-0.100347637091199,
-0.899230501146693));
#52334=CARTESIAN_POINT('Ctrl Pts',(0.731726110718017,0.283782753153026,
-0.883372990570751));
#52335=CARTESIAN_POINT('Ctrl Pts',(0.50718923144649,0.598928072140841,-0.867515479994805));
#52336=CARTESIAN_POINT('Ctrl Pts',(0.159359146780791,0.768479286923808,
-0.851657969418865));
#52337=CARTESIAN_POINT('Ctrl Pts',(-0.227209733579464,0.751220000439534,
-0.835800458842918));
#52338=CARTESIAN_POINT('Ctrl Pts',(-0.558545942161822,0.551345792210469,
-0.819942948266977));
#52339=CARTESIAN_POINT('Ctrl Pts',(-0.754104584306817,0.21744431016025,
-0.804085437691032));
#52340=CARTESIAN_POINT('Ctrl Pts',(-0.766347087943781,-0.169315955815492,
-0.78822792711509));
#52341=CARTESIAN_POINT('Ctrl Pts',(-0.592297408981341,-0.514917014098013,
-0.772370416539145));
#52342=CARTESIAN_POINT('Ctrl Pts',(-0.274265481240269,-0.735346311538768,
-0.756512905963204));
#52343=CARTESIAN_POINT('Ctrl Pts',(0.110437953335934,-0.777019440269414,
-0.740655395387258));
#52344=CARTESIAN_POINT('Ctrl Pts',(0.468294900605758,-0.629806032172024,
-0.724797884811316));
#52345=CARTESIAN_POINT('Ctrl Pts',(0.712313509469297,-0.329492361552069,
-0.708940374235371));
#52346=CARTESIAN_POINT('Ctrl Pts',(0.7831750195956,0.0509179808619445,-0.69308286365943));
#52347=CARTESIAN_POINT('Ctrl Pts',(0.663653626135406,0.418950613570325,
-0.677225353083484));
#52348=CARTESIAN_POINT('Ctrl Pts',(0.382803920154978,0.685140066561286,
-0.661367842507542));
#52349=CARTESIAN_POINT('Ctrl Pts',(0.00889797514763637,0.784778043864566,
-0.645510331931599));
#52350=CARTESIAN_POINT('Ctrl Pts',(-0.367170988728106,0.693643436594083,
-0.629652821355654));
#52351=CARTESIAN_POINT('Ctrl Pts',(-0.6539839406043,0.43389025977233,-0.613795310779713));
#52352=CARTESIAN_POINT('Ctrl Pts',(-0.781819194780839,0.0686622076972637,
-0.597937800203768));
#52353=CARTESIAN_POINT('Ctrl Pts',(-0.719601134362537,-0.313257018305708,
-0.582080289627826));
#52354=CARTESIAN_POINT('Ctrl Pts',(-0.482454418207954,-0.619026240514282,
-0.56622277905188));
#52355=CARTESIAN_POINT('Ctrl Pts',(-0.128027310457176,-0.774315671977985,
-0.55036526847594));
#52356=CARTESIAN_POINT('Ctrl Pts',(0.25752210136793,-0.741375828713559,
-0.534507757899993));
#52357=CARTESIAN_POINT('Ctrl Pts',(0.58047017355689,-0.528214094571827,
-0.518650247324052));
#52358=CARTESIAN_POINT('Ctrl Pts',(0.762311093038232,-0.18664819721801,
-0.502792736748107));
#52359=CARTESIAN_POINT('Ctrl Pts',(0.758840944497711,0.200290222045565,
-0.486935226172165));
#52360=CARTESIAN_POINT('Ctrl Pts',(0.570903290280831,0.538539864114544,
-0.471077715596219));
#52361=CARTESIAN_POINT('Ctrl Pts',(0.244184107857459,0.745875239945465,
-0.455220205020278));
#52362=CARTESIAN_POINT('Ctrl Pts',(-0.14189406623027,0.771894957918566,
-0.439362694444333));
#52363=CARTESIAN_POINT('Ctrl Pts',(-0.493479050867978,0.61027385529337,
-0.42350518386839));
#52364=CARTESIAN_POINT('Ctrl Pts',(-0.725103653436951,0.300300589163106,
-0.407647673292446));
#52365=CARTESIAN_POINT('Ctrl Pts',(-0.780461986703319,-0.0826730876933915,
-0.391790162716504));
#52366=CARTESIAN_POINT('Ctrl Pts',(-0.646096930557075,-0.445549669947661,
-0.375932652140559));
#52367=CARTESIAN_POINT('Ctrl Pts',(-0.354671439060398,-0.700117077646639,
-0.360075141564617));
#52368=CARTESIAN_POINT('Ctrl Pts',(0.0229715349940275,-0.784492231170089,
-0.344217630988674));
#52369=CARTESIAN_POINT('Ctrl Pts',(0.395030332049294,-0.678164278417535,
-0.32836012041273));
#52370=CARTESIAN_POINT('Ctrl Pts',(0.67106075874077,-0.406980602684816,
-0.312502609836786));
#52371=CARTESIAN_POINT('Ctrl Pts',(0.783962262705086,-0.0368635498603739,
-0.296645099260844));
#52372=CARTESIAN_POINT('Ctrl Pts',(0.706289495057392,0.342214703354879,
-0.280787588684899));
#52373=CARTESIAN_POINT('Ctrl Pts',(0.456924005754423,0.638103599690982,
-0.264930078108956));
#52374=CARTESIAN_POINT('Ctrl Pts',(0.0964843562473045,0.778875161746238,
-0.249072567533014));
#52375=CARTESIAN_POINT('Ctrl Pts',(-0.287409813109609,0.730309090546973,
-0.233215056957069));
#52376=CARTESIAN_POINT('Ctrl Pts',(-0.601437149847266,0.504211328984171,
-0.217357546381126));
#52377=CARTESIAN_POINT('Ctrl Pts',(-0.769260555748459,0.155544313360371,
-0.201500035805183));
#52378=CARTESIAN_POINT('Ctrl Pts',(-0.750083330065511,-0.230934242753795,
-0.185642525229239));
#52379=CARTESIAN_POINT('Ctrl Pts',(-0.548567908879648,-0.561274542499788,
-0.169785014653295));
#52380=CARTESIAN_POINT('Ctrl Pts',(-0.213699688385254,-0.755174347285152,
-0.153927504077352));
#52381=CARTESIAN_POINT('Ctrl Pts',(0.173115460605444,-0.765497240872467,
-0.138069993501409));
#52382=CARTESIAN_POINT('Ctrl Pts',(0.51785084486316,-0.589735954039219,
-0.122212482925465));
#52383=CARTESIAN_POINT('Ctrl Pts',(0.73669528515483,-0.270612327298038,
-0.106354972349523));
#52384=CARTESIAN_POINT('Ctrl Pts',(0.776467346061449,0.114289367285656,
-0.0904974617735793));
#52385=CARTESIAN_POINT('Ctrl Pts',(0.627464170859799,0.471418880043696,
-0.0746399511976351));
#52386=CARTESIAN_POINT('Ctrl Pts',(0.325975076844769,0.713929799385627,
-0.0587824406216925));
#52387=CARTESIAN_POINT('Ctrl Pts',(-0.0548469677254658,0.782933924134,-0.0429249300457488));
#52388=CARTESIAN_POINT('Ctrl Pts',(-0.29969712480825,0.701979163404131,
-0.0323532563284528));
#52389=CARTESIAN_POINT('Ctrl Pts',(-0.405096567646226,0.634709045147742,
-0.027067419469805));
#52390=CARTESIAN_POINT('Ctrl Pts',(-0.342067962509741,0.71332231075751,
-5.8089));
#52391=CARTESIAN_POINT('Ctrl Pts',(-0.460521881974901,0.656518688787926,
-5.80361416314135));
#52392=CARTESIAN_POINT('Ctrl Pts',(-0.668467913999907,0.482822123354284,
-5.79304248942406));
#52393=CARTESIAN_POINT('Ctrl Pts',(-0.81790697907055,0.104654431008339,
-5.77718497884811));
#52394=CARTESIAN_POINT('Ctrl Pts',(-0.76850808527292,-0.298848385144198,
-5.76132746827218));
#52395=CARTESIAN_POINT('Ctrl Pts',(-0.53229805344993,-0.629755578447219,
-5.74546995769623));
#52396=CARTESIAN_POINT('Ctrl Pts',(-0.166687806613194,-0.807548479192264,
-5.72961244712028));
#52397=CARTESIAN_POINT('Ctrl Pts',(0.239441088352843,-0.789046946221705,
-5.71375493654434));
#52398=CARTESIAN_POINT('Ctrl Pts',(0.587364837768938,-0.578728216806966,
-5.6978974259684));
#52399=CARTESIAN_POINT('Ctrl Pts',(0.792504962384066,-0.2277293106754,-5.68203991539245));
#52400=CARTESIAN_POINT('Ctrl Pts',(0.80499438247605,0.178630374729474,-5.66618240481651));
#52401=CARTESIAN_POINT('Ctrl Pts',(0.621796689907431,0.541565676804147,
-5.65032489424056));
#52402=CARTESIAN_POINT('Ctrl Pts',(0.287445793992361,0.772851636913208,
-5.63446738366463));
#52403=CARTESIAN_POINT('Ctrl Pts',(-0.116780656177354,0.816263974340416,
-5.61860987308867));
#52404=CARTESIAN_POINT('Ctrl Pts',(-0.492618748730099,0.661249900488588,
-5.60275236251274));
#52405=CARTESIAN_POINT('Ctrl Pts',(-0.748705598981454,0.345491775112376,
-5.58689485193679));
#52406=CARTESIAN_POINT('Ctrl Pts',(-0.822788752131379,-0.0542523051869823,
-5.57103734136086));
#52407=CARTESIAN_POINT('Ctrl Pts',(-0.696859256610704,-0.440808147714975,
-5.5551798307849));
#52408=CARTESIAN_POINT('Ctrl Pts',(-0.401529453140775,-0.720207429259136,
-5.53932232020897));
#52409=CARTESIAN_POINT('Ctrl Pts',(-0.00859140014129245,-0.824530674507732,
-5.52346480963302));
#52410=CARTESIAN_POINT('Ctrl Pts',(0.386435146339414,-0.728417820893135,
-5.50760729905707));
#52411=CARTESIAN_POINT('Ctrl Pts',(0.687522734759737,-0.455233054357242,
-5.49174978848114));
#52412=CARTESIAN_POINT('Ctrl Pts',(0.821479642051262,-0.0713851678466922,
-5.47589227790518));
#52413=CARTESIAN_POINT('Ctrl Pts',(0.755742131611029,0.329815819763054,
-5.46003476732925));
#52414=CARTESIAN_POINT('Ctrl Pts',(0.506290409450845,0.650841505908578,
-5.4441772567533));
#52415=CARTESIAN_POINT('Ctrl Pts',(0.133763977544822,0.813653392289577,
-5.42831974617736));
#52416=CARTESIAN_POINT('Ctrl Pts',(-0.271279291337799,0.778673352945406,
-5.41246223560142));
#52417=CARTESIAN_POINT('Ctrl Pts',(-0.61037696967741,0.55440472524481,-5.39660472502547));
#52418=CARTESIAN_POINT('Ctrl Pts',(-0.801097418326339,0.195365224233614,
-5.38074721444952));
#52419=CARTESIAN_POINT('Ctrl Pts',(-0.797078187159076,-0.211165830674235,
-5.36488970387359));
#52420=CARTESIAN_POINT('Ctrl Pts',(-0.599296315636618,-0.566364344351477,
-5.34903219329764));
#52421=CARTESIAN_POINT('Ctrl Pts',(-0.255830823180538,-0.783884707338891,
-5.3331746827217));
#52422=CARTESIAN_POINT('Ctrl Pts',(0.149824874179238,-0.810849647940832,
-5.31731717214575));
#52423=CARTESIAN_POINT('Ctrl Pts',(0.519059472982411,-0.64070422817085,
-5.30145966156981));
#52424=CARTESIAN_POINT('Ctrl Pts',(0.762115315916334,-0.31480929105487,
-5.28560215099387));
#52425=CARTESIAN_POINT('Ctrl Pts',(0.819907682511568,0.0876129935981942,
-5.26974464041792));
#52426=CARTESIAN_POINT('Ctrl Pts',(0.678387760839459,0.468737336289701,
-5.25388712984198));
#52427=CARTESIAN_POINT('Ctrl Pts',(0.371957789134283,0.73591578838279,-5.23802961926604));
#52428=CARTESIAN_POINT('Ctrl Pts',(-0.0248918233091328,0.824199636994026,
-5.22217210869009));
#52429=CARTESIAN_POINT('Ctrl Pts',(-0.415690454198512,0.712127861255944,
-5.20631459811415));
#52430=CARTESIAN_POINT('Ctrl Pts',(-0.705438421208997,0.426944116215333,
-5.19045708753821));
#52431=CARTESIAN_POINT('Ctrl Pts',(-0.823700562483377,0.0379740418351834,
-5.17459957696226));
#52432=CARTESIAN_POINT('Ctrl Pts',(-0.741728399997165,-0.360227185434942,
-5.15874206638631));
#52433=CARTESIAN_POINT('Ctrl Pts',(-0.479448639680594,-0.670860377721891,
-5.14288455581038));
#52434=CARTESIAN_POINT('Ctrl Pts',(-0.100619165878374,-0.818413360073425,
-5.12702704523443));
#52435=CARTESIAN_POINT('Ctrl Pts',(0.302669935053257,-0.767017310693566,
-5.11116953465849));
#52436=CARTESIAN_POINT('Ctrl Pts',(0.632382658263431,-0.52916615350607,
-5.09531202408254));
#52437=CARTESIAN_POINT('Ctrl Pts',(0.808368763992744,-0.162679396020442,
-5.0794545135066));
#52438=CARTESIAN_POINT('Ctrl Pts',(0.787847590241883,0.243353280312371,
-5.06359700293066));
#52439=CARTESIAN_POINT('Ctrl Pts',(0.575807652407709,0.590228931786179,
-5.04773949235471));
#52440=CARTESIAN_POINT('Ctrl Pts',(0.22379397941877,0.793625162948256,-5.03188198177878));
#52441=CARTESIAN_POINT('Ctrl Pts',(-0.182622025795887,0.804098153326407,
-5.01602447120283));
#52442=CARTESIAN_POINT('Ctrl Pts',(-0.544644235677511,0.619102011813879,
-5.00016696062689));
#52443=CARTESIAN_POINT('Ctrl Pts',(-0.77426826071474,0.283607660225359,
-4.98430945005094));
#52444=CARTESIAN_POINT('Ctrl Pts',(-0.815674536281549,-0.120829199081238,
-4.968451939475));
#52445=CARTESIAN_POINT('Ctrl Pts',(-0.658797563898192,-0.49589355137019,
-4.95259442889906));
#52446=CARTESIAN_POINT('Ctrl Pts',(-0.341772744670322,-0.750410577943334,
-4.93673691832311));
#52447=CARTESIAN_POINT('Ctrl Pts',(0.0583339986090347,-0.822509446204123,
-4.92087940774717));
#52448=CARTESIAN_POINT('Ctrl Pts',(0.444260264019303,-0.694663560511296,
-4.90502189717122));
#52449=CARTESIAN_POINT('Ctrl Pts',(0.722190798084908,-0.397951122187407,
-4.88916438659529));
#52450=CARTESIAN_POINT('Ctrl Pts',(0.824563152123462,-0.00450029431852763,
-4.87330687601934));
#52451=CARTESIAN_POINT('Ctrl Pts',(0.726491514507689,0.390044515199301,
-4.85744936544339));
#52452=CARTESIAN_POINT('Ctrl Pts',(0.451816230832899,0.689772961230496,
-4.84159185486746));
#52453=CARTESIAN_POINT('Ctrl Pts',(0.0673084272727246,0.821823715955436,
-4.8257343442915));
#52454=CARTESIAN_POINT('Ctrl Pts',(-0.333561458196853,0.754096411670499,
-4.80987683371557));
#52455=CARTESIAN_POINT('Ctrl Pts',(-0.653345510554885,0.503054955572955,
-4.79401932313961));
#52456=CARTESIAN_POINT('Ctrl Pts',(-0.814307061897926,0.129725299891355,
-4.77816181256369));
#52457=CARTESIAN_POINT('Ctrl Pts',(-0.777317786189346,-0.275139426041463,
-4.76230430198772));
#52458=CARTESIAN_POINT('Ctrl Pts',(-0.551369448404747,-0.613120196906429,
-4.7464467914118));
#52459=CARTESIAN_POINT('Ctrl Pts',(-0.191388086187902,-0.802056883864271,
-4.73058928083584));
#52460=CARTESIAN_POINT('Ctrl Pts',(0.215118022922846,-0.796020653439657,
-4.71473177025991));
#52461=CARTESIAN_POINT('Ctrl Pts',(0.569330847910481,-0.596478859731226,
-4.69887425968396));
#52462=CARTESIAN_POINT('Ctrl Pts',(0.785144391492888,-0.251938343639862,
-4.68301674910802));
#52463=CARTESIAN_POINT('Ctrl Pts',(0.810096294641137,0.153846150089727,
-4.66715923853207));
#52464=CARTESIAN_POINT('Ctrl Pts',(0.638120970924981,0.522232008741798,
-4.65130172795613));
#52465=CARTESIAN_POINT('Ctrl Pts',(0.311024096796169,0.763667896209378,
-4.63544421738018));
#52466=CARTESIAN_POINT('Ctrl Pts',(-0.0916799777052979,0.819462888834321,
-4.61958670680424));
#52467=CARTESIAN_POINT('Ctrl Pts',(-0.472097462466847,0.676053718591279,
-4.6037291962283));
#52468=CARTESIAN_POINT('Ctrl Pts',(-0.737752239747422,0.368301883291948,
-4.58787168565236));
#52469=CARTESIAN_POINT('Ctrl Pts',(-0.824065988501475,-0.0289808744488347,
-4.57201417507641));
#52470=CARTESIAN_POINT('Ctrl Pts',(-0.710056601669826,-0.419218638557295,
-4.55615666450047));
#52471=CARTESIAN_POINT('Ctrl Pts',(-0.423438750377111,-0.707548068450336,
-4.54029915392452));
#52472=CARTESIAN_POINT('Ctrl Pts',(-0.0338866931013497,-0.823878836067166,
-4.52444164334859));
#52473=CARTESIAN_POINT('Ctrl Pts',(0.363902918825875,-0.739931963195765,
-4.50858413277264));
#52474=CARTESIAN_POINT('Ctrl Pts',(0.673230957571867,-0.476114190353113,
-4.4927266221967));
#52475=CARTESIAN_POINT('Ctrl Pts',(0.818902519438615,-0.0965572790928855,
-4.47686911162076));
#52476=CARTESIAN_POINT('Ctrl Pts',(0.765506139269209,0.306471850632131,
-4.46101160104481));
#52477=CARTESIAN_POINT('Ctrl Pts',(0.526022003667289,0.635000390666482,
-4.44515409046887));
#52478=CARTESIAN_POINT('Ctrl Pts',(0.158666582716821,0.809165965681761,
-4.42929657989292));
#52479=CARTESIAN_POINT('Ctrl Pts',(-0.247259277744567,0.786630468554307,
-4.41343906931699));
#52480=CARTESIAN_POINT('Ctrl Pts',(-0.593078600001993,0.572872078834715,
-4.39758155874103));
#52481=CARTESIAN_POINT('Ctrl Pts',(-0.794725772869754,0.21985356586898,
-4.38172404816509));
#52482=CARTESIAN_POINT('Ctrl Pts',(-0.80318215643975,-0.186609399724462,
-4.36586653758915));
#52483=CARTESIAN_POINT('Ctrl Pts',(-0.616392078840929,-0.547709274735137,
-4.3500090270132));
#52484=CARTESIAN_POINT('Ctrl Pts',(-0.279762551845409,-0.775665881081332,
-4.33415151643726));
#52485=CARTESIAN_POINT('Ctrl Pts',(0.124874771111987,-0.815064988837368,
-4.31829400586132));
#52486=CARTESIAN_POINT('Ctrl Pts',(0.499156144359348,-0.65632902422264,
-4.30243649528538));
#52487=CARTESIAN_POINT('Ctrl Pts',(0.752097084461584,-0.338045292872298,
-4.28657898470943));
#52488=CARTESIAN_POINT('Ctrl Pts',(0.822209891469548,0.062414252045241,
-4.27072147413349));
#52489=CARTESIAN_POINT('Ctrl Pts',(0.692450763624001,0.447701445659124,
-4.25486396355754));
#52490=CARTESIAN_POINT('Ctrl Pts',(0.394362994451903,0.72415638718143,-4.23900645298161));
#52491=CARTESIAN_POINT('Ctrl Pts',(0.000409077774761542,0.824575331394352,
-4.22314894240565));
#52492=CARTESIAN_POINT('Ctrl Pts',(-0.39364428208252,0.724547323280179,
-4.20729143182972));
#52493=CARTESIAN_POINT('Ctrl Pts',(-0.692006207039603,0.448388284757077,
-4.19143392125377));
#52494=CARTESIAN_POINT('Ctrl Pts',(-0.822147558434337,0.0632300296472444,
-4.17557641067783));
#52495=CARTESIAN_POINT('Ctrl Pts',(-0.75243212758377,-0.33729888506856,
-4.15971890010188));
#52496=CARTESIAN_POINT('Ctrl Pts',(-0.499807117626442,-0.655833431336555,
-4.14386138952594));
#52497=CARTESIAN_POINT('Ctrl Pts',(-0.125683428694324,-0.814940685105593,
-4.12800387895));
#52498=CARTESIAN_POINT('Ctrl Pts',(0.278992787436487,-0.775943083638968,
-4.11214636837406));
#52499=CARTESIAN_POINT('Ctrl Pts',(0.61584833050845,-0.548320598098126,
-4.09628885779811));
#52500=CARTESIAN_POINT('Ctrl Pts',(0.802996604582439,-0.187406236603287,
-4.08043134722217));
#52501=CARTESIAN_POINT('Ctrl Pts',(0.794943523499005,0.219064919454756,
-4.06457383664622));
#52502=CARTESIAN_POINT('Ctrl Pts',(0.593646719870428,0.572283335836205,
-4.04871632607028));
#52503=CARTESIAN_POINT('Ctrl Pts',(0.24803966194915,0.786384747174615,-4.03285881549433));
#52504=CARTESIAN_POINT('Ctrl Pts',(-0.157863638657288,0.809322998609712,
-4.01700130491839));
#52505=CARTESIAN_POINT('Ctrl Pts',(-0.525391688334729,0.635522004589546,
-4.00114379434245));
#52506=CARTESIAN_POINT('Ctrl Pts',(-0.765201676732551,0.307231245830278,
-3.98528628376651));
#52507=CARTESIAN_POINT('Ctrl Pts',(-0.818997921841139,-0.0957447048594847,
-3.96942877319056));
#52508=CARTESIAN_POINT('Ctrl Pts',(-0.673703033435362,-0.475445966676259,
-3.95357126261462));
#52509=CARTESIAN_POINT('Ctrl Pts',(-0.364636910693384,-0.739570529326795,
-3.93771375203868));
#52510=CARTESIAN_POINT('Ctrl Pts',(0.0330692121452029,-0.823912053375134,
-3.92185624146273));
#52511=CARTESIAN_POINT('Ctrl Pts',(0.42273650270493,-0.707967862102183,
-3.90599873088679));
#52512=CARTESIAN_POINT('Ctrl Pts',(0.709640297464547,-0.419922960438174,
-3.89014122031084));
#52513=CARTESIAN_POINT('Ctrl Pts',(0.824036827624427,-0.029798510154067,
-3.8742837097349));
#52514=CARTESIAN_POINT('Ctrl Pts',(0.738117310949273,0.367569693753101,
-3.85842619915896));
#52515=CARTESIAN_POINT('Ctrl Pts',(0.472768020175167,0.675584964004073,
-3.84256868858302));
#52516=CARTESIAN_POINT('Ctrl Pts',(0.0924930152864017,0.819371519282897,
-3.82671117800707));
#52517=CARTESIAN_POINT('Ctrl Pts',(-0.310266221569808,0.763976122821601,
-3.81085366743113));
#52518=CARTESIAN_POINT('Ctrl Pts',(-0.637602490801524,0.522864904360988,
-3.79499615685519));
#52519=CARTESIAN_POINT('Ctrl Pts',(-0.809943247541721,0.154649863402152,
-3.77913864627924));
#52520=CARTESIAN_POINT('Ctrl Pts',(-0.78539398181045,-0.251159188214685,
-3.7632811357033));
#52521=CARTESIAN_POINT('Ctrl Pts',(-0.569922402451707,-0.595913667969116,
-3.74742362512736));
#52522=CARTESIAN_POINT('Ctrl Pts',(-0.21590774002352,-0.795806818446958,
-3.73156611455141));
#52523=CARTESIAN_POINT('Ctrl Pts',(0.190592179753276,-0.802246387031831,
-3.71570860397547));
#52524=CARTESIAN_POINT('Ctrl Pts',(0.550760830433868,-0.613666971694362,
-3.69985109339953));
#52525=CARTESIAN_POINT('Ctrl Pts',(0.777044406314893,-0.275910556346559,
-3.68399358282358));
#52526=CARTESIAN_POINT('Ctrl Pts',(0.814435376343574,0.128917269009375,
-3.66813607224764));
#52527=CARTESIAN_POINT('Ctrl Pts',(0.653844327216543,0.502406449257448,
-3.65227856167169));
#52528=CARTESIAN_POINT('Ctrl Pts',(0.334309519166617,0.753765076057067,
-3.63642105109575));
#52529=CARTESIAN_POINT('Ctrl Pts',(-0.0664929689842511,0.821890095794073,
-3.6205635405198));
#52530=CARTESIAN_POINT('Ctrl Pts',(-0.451131605905745,0.690220920170952,
-3.60470602994387));
#52531=CARTESIAN_POINT('Ctrl Pts',(-0.72610414919172,0.390765158394787,
-3.58884851936792));
#52532=CARTESIAN_POINT('Ctrl Pts',(-0.824567211492583,-0.00368214883957207,
-3.57299100879198));
#52533=CARTESIAN_POINT('Ctrl Pts',(-0.72258529534248,-0.397234358337186,
-3.55713349821603));
#52534=CARTESIAN_POINT('Ctrl Pts',(-0.444949300379643,-0.694222417226928,
-3.54127598764009));
#52535=CARTESIAN_POINT('Ctrl Pts',(-0.059150075441984,-0.822451161506835,
-3.52541847706415));
#52536=CARTESIAN_POINT('Ctrl Pts',(0.341028008407468,-0.750749320326278,
-3.50956096648821));
#52537=CARTESIAN_POINT('Ctrl Pts',(0.658305206988058,-0.496546975563384,
-3.49370345591226));
#52538=CARTESIAN_POINT('Ctrl Pts',(0.815554246323718,-0.121638463456612,
-3.47784594533632));
#52539=CARTESIAN_POINT('Ctrl Pts',(0.774549279131463,0.282839280662471,
-3.46198843476038));
#52540=CARTESIAN_POINT('Ctrl Pts',(0.545258249383206,0.618561303322714,
-3.44613092418443));
#52541=CARTESIAN_POINT('Ctrl Pts',(0.183419773502581,0.803916557347213,
-3.43027341360849));
#52542=CARTESIAN_POINT('Ctrl Pts',(-0.223006423105693,0.793846823853531,
-3.41441590303254));
#52543=CARTESIAN_POINT('Ctrl Pts',(-0.575221735445436,0.590799965775112,
-3.3985583924566));
#52544=CARTESIAN_POINT('Ctrl Pts',(-0.787605743849167,0.244134874085071,
-3.38270088188066));
#52545=CARTESIAN_POINT('Ctrl Pts',(-0.808529778883429,-0.161877240980456,
-3.36684337130471));
#52546=CARTESIAN_POINT('Ctrl Pts',(-0.632907393145164,-0.528538433977061,
-3.35098586072877));
#52547=CARTESIAN_POINT('Ctrl Pts',(-0.303430831528625,-0.76671661972764,
-3.33512835015283));
#52548=CARTESIAN_POINT('Ctrl Pts',(0.0998070749963794,-0.818512792978461,
-3.31927083957688));
#52549=CARTESIAN_POINT('Ctrl Pts',(0.478782766485345,-0.671335763240253,
-3.30341332900094));
#52550=CARTESIAN_POINT('Ctrl Pts',(0.741370612358751,-0.360962961561908,
-3.287555818425));
#52551=CARTESIAN_POINT('Ctrl Pts',(0.82373783540453,0.0371567357526397,
-3.27169830784905));
#52552=CARTESIAN_POINT('Ctrl Pts',(0.705861693973048,0.426243960039592,
-3.25584079727311));
#52553=CARTESIAN_POINT('Ctrl Pts',(0.416396832949279,0.711715056745706,
-3.23998328669717));
#52554=CARTESIAN_POINT('Ctrl Pts',(0.0257095936351012,0.82417453326577,
-3.22412577612122));
#52555=CARTESIAN_POINT('Ctrl Pts',(-0.371227419948954,0.736284487930295,
-3.20826826554528));
#52556=CARTESIAN_POINT('Ctrl Pts',(-0.677922339068225,0.469410211521862,
-3.19241075496933));
#52557=CARTESIAN_POINT('Ctrl Pts',(-0.81982034806056,0.0884264745118526,
-3.1765532443934));
#52558=CARTESIAN_POINT('Ctrl Pts',(-0.76242729901627,-0.314052954457505,
-3.16069573381745));
#52559=CARTESIAN_POINT('Ctrl Pts',(-0.519694933307771,-0.640188894610773,
-3.14483822324151));
#52560=CARTESIAN_POINT('Ctrl Pts',(-0.150629336958933,-0.810700590437707,
-3.12898071266556));
#52561=CARTESIAN_POINT('Ctrl Pts',(0.255052915715792,-0.784138160449806,
-3.11312320208962));
#52562=CARTESIAN_POINT('Ctrl Pts',(0.598734065894616,-0.566958695873019,
-3.09726569151368));
#52563=CARTESIAN_POINT('Ctrl Pts',(0.796868273066979,-0.211956599019665,
-3.08140818093773));
#52564=CARTESIAN_POINT('Ctrl Pts',(0.80129086813917,0.194570267835308,-3.06555067036179));
#52565=CARTESIAN_POINT('Ctrl Pts',(0.610926757460146,0.553798827651308,
-3.04969315978584));
#52566=CARTESIAN_POINT('Ctrl Pts',(0.272051768556222,0.778403802479257,
-3.0338356492099));
#52567=CARTESIAN_POINT('Ctrl Pts',(-0.132956593256252,0.813785714299792,
-3.01797813863396));
#52568=CARTESIAN_POINT('Ctrl Pts',(-0.505644386049347,0.65134353404752,
-3.00212062805802));
#52569=CARTESIAN_POINT('Ctrl Pts',(-0.755414511667619,0.330565515519547,
-2.98626311748207));
#52570=CARTESIAN_POINT('Ctrl Pts',(-0.821550067050345,-0.0705700490173305,
-2.97040560690613));
#52571=CARTESIAN_POINT('Ctrl Pts',(-0.68797408504582,-0.454550660316427,
-2.95454809633018));
#52572=CARTESIAN_POINT('Ctrl Pts',(-0.387157702586595,-0.728034036166306,
-2.93869058575424));
#52573=CARTESIAN_POINT('Ctrl Pts',(0.00777328480777176,-0.824538792618049,
-2.9228330751783));
#52574=CARTESIAN_POINT('Ctrl Pts',(0.400814655583785,-0.720605478995258,
-2.90697556460235));
#52575=CARTESIAN_POINT('Ctrl Pts',(0.69642153723441,-0.441499362360574,
-2.89111805402641));
#52576=CARTESIAN_POINT('Ctrl Pts',(0.822734517698912,-0.0550686650961424,
-2.87526054345047));
#52577=CARTESIAN_POINT('Ctrl Pts',(0.749048031324911,0.344748736411039,
-2.85940303287452));
#52578=CARTESIAN_POINT('Ctrl Pts',(0.493274609641072,0.660760776659891,
-2.84354552229858));
#52579=CARTESIAN_POINT('Ctrl Pts',(0.117590503756079,0.816147730447817,
-2.82768801172263));
#52580=CARTESIAN_POINT('Ctrl Pts',(-0.286678811027477,0.773136406979133,
-2.8118305011467));
#52581=CARTESIAN_POINT('Ctrl Pts',(-0.621259048561971,0.542182477648074,
-2.79597299057075));
#52582=CARTESIAN_POINT('Ctrl Pts',(-0.80481671951144,0.179428795023482,
-2.78011547999481));
#52583=CARTESIAN_POINT('Ctrl Pts',(-0.792730581501495,-0.226942436844752,
-2.76425796941886));
#52584=CARTESIAN_POINT('Ctrl Pts',(-0.587938667525923,-0.578145974401426,
-2.74840045884292));
#52585=CARTESIAN_POINT('Ctrl Pts',(-0.240224076174663,-0.788807351458366,
-2.73254294826698));
#52586=CARTESIAN_POINT('Ctrl Pts',(0.165886858253439,-0.807716654989569,
-2.71668543769103));
#52587=CARTESIAN_POINT('Ctrl Pts',(0.531672168203069,-0.630277200957627,
-2.70082792711509));
#52588=CARTESIAN_POINT('Ctrl Pts',(0.768212687900203,-0.299622947448753,
-2.68497041653915));
#52589=CARTESIAN_POINT('Ctrl Pts',(0.818007514189052,0.103866988109699,
-2.6691129059632));
#52590=CARTESIAN_POINT('Ctrl Pts',(0.668951966282746,0.482107779749695,
-2.65325539538726));
#52591=CARTESIAN_POINT('Ctrl Pts',(0.357280126341784,0.743152444529339,
-2.63739788481132));
#52592=CARTESIAN_POINT('Ctrl Pts',(-0.0412433446456093,0.823543338878517,
-2.62154037423537));
#52593=CARTESIAN_POINT('Ctrl Pts',(-0.429740924215648,0.703738149131488,
-2.60568286365943));
#52594=CARTESIAN_POINT('Ctrl Pts',(-0.713772295217946,0.412860454715681,
-2.58982535308349));
#52595=CARTESIAN_POINT('Ctrl Pts',(-0.824291949601193,0.0216200442043072,
-2.57396784250754));
#52596=CARTESIAN_POINT('Ctrl Pts',(-0.73443353925878,-0.374876007368511,
-2.5581103319316));
#52597=CARTESIAN_POINT('Ctrl Pts',(-0.466040847054833,-0.680243025223445,
-2.54225282135565));
#52598=CARTESIAN_POINT('Ctrl Pts',(-0.0843577568782632,-0.820248994722455,
-2.52639531077971));
#52599=CARTESIAN_POINT('Ctrl Pts',(0.317831956074426,-0.76085970598175,
-2.51053780020377));
#52600=CARTESIAN_POINT('Ctrl Pts',(0.642759538422818,-0.516512168545157,
-2.49468028962782));
#52601=CARTESIAN_POINT('Ctrl Pts',(0.811437975725651,-0.146605102363427,
-2.47882277905189));
#52602=CARTESIAN_POINT('Ctrl Pts',(0.782863035387856,0.258940364393128,
-2.46296526847593));
#52603=CARTESIAN_POINT('Ctrl Pts',(0.563981032058397,0.601539724346679,
-2.4471077579));
#52604=CARTESIAN_POINT('Ctrl Pts',(0.208000240125556,0.797910110599211,
-2.43125024732405));
#52605=CARTESIAN_POINT('Ctrl Pts',(-0.198543566039071,0.800315623284477,
-2.41539273674811));
#52606=CARTESIAN_POINT('Ctrl Pts',(-0.556823191598891,0.608171503596115,
-2.39953522617216));
#52607=CARTESIAN_POINT('Ctrl Pts',(-0.779744036109187,0.268186283468949,
-2.38367771559622));
#52608=CARTESIAN_POINT('Ctrl Pts',(-0.813116018699228,-0.136992644413672,
-2.36782020502028));
#52609=CARTESIAN_POINT('Ctrl Pts',(-0.648826706279392,-0.508869875024419,
-2.35196269444433));
#52610=CARTESIAN_POINT('Ctrl Pts',(-0.326813374099942,-0.757045350687886,
-2.33610518386839));
#52611=CARTESIAN_POINT('Ctrl Pts',(0.0746453917760193,-0.821189813609094,
-2.32024767329245));
#52612=CARTESIAN_POINT('Ctrl Pts',(0.457958524721799,-0.685710313560593,
-2.3043901627165));
#52613=CARTESIAN_POINT('Ctrl Pts',(0.729946000595748,-0.383540715834715,
-2.28853265214056));
#52614=CARTESIAN_POINT('Ctrl Pts',(0.824490075470356,0.0118642294153475,
-2.27267514156462));
#52615=CARTESIAN_POINT('Ctrl Pts',(0.718607922977105,0.404385085683513,
-2.25681763098867));
#52616=CARTESIAN_POINT('Ctrl Pts',(0.43803855562953,0.698603512924695,-2.24096012041273));
#52617=CARTESIAN_POINT('Ctrl Pts',(0.0509858990848059,0.822997620034983,
-2.22510260983679));
#52618=CARTESIAN_POINT('Ctrl Pts',(-0.348460977483367,0.747328302461555,
-2.20924509926084));
#52619=CARTESIAN_POINT('Ctrl Pts',(-0.663200079901485,0.48999010041775,
-2.1933875886849));
#52620=CARTESIAN_POINT('Ctrl Pts',(-0.816721122867659,0.11353964924432,
-2.17753007810895));
#52621=CARTESIAN_POINT('Ctrl Pts',(-0.771704501963684,-0.290511284010991,
-2.16167256753301));
#52622=CARTESIAN_POINT('Ctrl Pts',(-0.539093358611228,-0.623941499813884,
-2.14581505695707));
#52623=CARTESIAN_POINT('Ctrl Pts',(-0.175433399414776,-0.805697068915178,
-2.12995754638113));
#52624=CARTESIAN_POINT('Ctrl Pts',(0.230872863776256,-0.791594823922241,
-2.11410003580518));
#52625=CARTESIAN_POINT('Ctrl Pts',(0.581055980716084,-0.585062895561496,
-2.09824252522924));
#52626=CARTESIAN_POINT('Ctrl Pts',(0.789989540421377,-0.236307364492848,
-2.08238501465329));
#52627=CARTESIAN_POINT('Ctrl Pts',(0.806883646945381,0.169892391768596,
-2.06652750407735));
#52628=CARTESIAN_POINT('Ctrl Pts',(0.627631492776286,0.534792813867337,
-2.05066999350141));
#52629=CARTESIAN_POINT('Ctrl Pts',(0.295807687332132,0.769689844420431,
-2.03481248292547));
#52630=CARTESIAN_POINT('Ctrl Pts',(-0.107924344253576,0.817482097911734,
-2.01895497234952));
#52631=CARTESIAN_POINT('Ctrl Pts',(-0.485420924615018,0.666551701246522,
-2.00309746177358));
#52632=CARTESIAN_POINT('Ctrl Pts',(-0.74491598197389,0.353588495696068,
-1.98723995119764));
#52633=CARTESIAN_POINT('Ctrl Pts',(-0.823328568585157,-0.0453289382210672,
-1.97138244062169));
#52634=CARTESIAN_POINT('Ctrl Pts',(-0.701597279854368,-0.433227309145766,
-1.95552493004575));
#52635=CARTESIAN_POINT('Ctrl Pts',(-0.409313912795,-0.715811962236716,-1.93966741946981));
#52636=CARTESIAN_POINT('Ctrl Pts',(-0.0175299625371316,-0.824389073740172,
-1.92380990889386));
#52637=CARTESIAN_POINT('Ctrl Pts',(0.378515366191811,-0.732564510500893,
-1.90795239831792));
#52638=CARTESIAN_POINT('Ctrl Pts',(0.682546965339704,-0.462660009720198,
-1.89209488774197));
#52639=CARTESIAN_POINT('Ctrl Pts',(0.82065744871628,-0.0802869625482141,
-1.87623737716603));
#52640=CARTESIAN_POINT('Ctrl Pts',(0.759273382308613,0.321603133390165,
-1.86037986659009));
#52641=CARTESIAN_POINT('Ctrl Pts',(0.51331668842555,0.64531435895427,-1.84452235601415));
#52642=CARTESIAN_POINT('Ctrl Pts',(0.142577258683111,0.812155385252811,
-1.8286648454382));
#52643=CARTESIAN_POINT('Ctrl Pts',(-0.262821438546577,0.781568638015269,
-1.81280733486226));
#52644=CARTESIAN_POINT('Ctrl Pts',(-0.604330574256394,0.560989484311131,
-1.79694982428631));
#52645=CARTESIAN_POINT('Ctrl Pts',(-0.798932305395987,0.204038760737729,
-1.78109231371037));
#52646=CARTESIAN_POINT('Ctrl Pts',(-0.799320676476057,-0.202511976550994,
-1.76523480313443));
#52647=CARTESIAN_POINT('Ctrl Pts',(-0.605401277930371,-0.559833847823624,
-1.74937729255848));
#52648=CARTESIAN_POINT('Ctrl Pts',(-0.264314196244243,-0.781065074211162,
-1.73351978198254));
#52649=CARTESIAN_POINT('Ctrl Pts',(0.141025323123172,-0.812426306028269,
-1.7176622714066));
#52650=CARTESIAN_POINT('Ctrl Pts',(0.512082836778417,-0.646293905870776,
-1.70180476083066));
#52651=CARTESIAN_POINT('Ctrl Pts',(0.758657552970296,-0.32305318727704,
-1.68594725025471));
#52652=CARTESIAN_POINT('Ctrl Pts',(0.820809344338949,0.0787188969346039,
-1.67008973967877));
#52653=CARTESIAN_POINT('Ctrl Pts',(0.683429661444197,0.461355115227956,
-1.65423222910282));
#52654=CARTESIAN_POINT('Ctrl Pts',(0.379914287181169,0.731839995411811,
-1.63837471852688));
#52655=CARTESIAN_POINT('Ctrl Pts',(-0.0159548819525065,0.824421061248809,
-1.62251720795093));
#52656=CARTESIAN_POINT('Ctrl Pts',(-0.407945560740477,0.716592676463325,
-1.606659697375));
#52657=CARTESIAN_POINT('Ctrl Pts',(-0.700768290582505,0.434566965383708,
-1.59080218679905));
#52658=CARTESIAN_POINT('Ctrl Pts',(-0.823240462038068,0.0469018779163698,
-1.57494467622311));
#52659=CARTESIAN_POINT('Ctrl Pts',(-0.74559017607201,-0.352164640237547,
-1.55908716564716));
#52660=CARTESIAN_POINT('Ctrl Pts',(-0.486693528750542,-0.665623056662763,
-1.54322965507122));
#52661=CARTESIAN_POINT('Ctrl Pts',(-0.109485999644142,-0.817274409467625,
-1.52737214449527));
#52662=CARTESIAN_POINT('Ctrl Pts',(0.29433660526624,-0.770253599335362,
-1.51151463391933));
#52663=CARTESIAN_POINT('Ctrl Pts',(0.626608591042582,-0.535990968319769,
-1.49565712334339));
#52664=CARTESIAN_POINT('Ctrl Pts',(0.806557583886217,-0.171433685034062,
-1.47979961276745));
#52665=CARTESIAN_POINT('Ctrl Pts',(0.790439579075549,0.23479760714198,-1.4639421021915));
#52666=CARTESIAN_POINT('Ctrl Pts',(0.582172720676841,0.583951682751627,
-1.44808459161556));
#52667=CARTESIAN_POINT('Ctrl Pts',(0.23238483546022,0.791152281635374,-1.43222708103962));
#52668=CARTESIAN_POINT('Ctrl Pts',(-0.173893742918745,0.806030775257647,
-1.41636957046367));
#52669=CARTESIAN_POINT('Ctrl Pts',(-0.537900294146628,0.624970333732493,
-1.40051205988773));
#52670=CARTESIAN_POINT('Ctrl Pts',(-0.771148052924077,0.291985145101832,
-1.38465454931178));
#52671=CARTESIAN_POINT('Ctrl Pts',(-0.816936557081062,-0.111979043545092,
-1.36879703873584));
#52672=CARTESIAN_POINT('Ctrl Pts',(-0.664135027220673,-0.488722119519188,
-1.3529395281599));
#52673=CARTESIAN_POINT('Ctrl Pts',(-0.349888160504345,-0.746661181278108,
-1.33708201758396));
#52674=CARTESIAN_POINT('Ctrl Pts',(0.0494134159009503,-0.823093529811607,
-1.32122450700801));
#52675=CARTESIAN_POINT('Ctrl Pts',(0.436703029003066,-0.699439138845034,
-1.30536699643207));
#52676=CARTESIAN_POINT('Ctrl Pts',(0.71783400759006,-0.405757294495029,
-1.28950948585612));
#52677=CARTESIAN_POINT('Ctrl Pts',(0.824465903291734,-0.0134394493220526,
-1.27365197528018));
#52678=CARTESIAN_POINT('Ctrl Pts',(0.730677447667856,0.382145406826143,
-1.25779446470424));
#52679=CARTESIAN_POINT('Ctrl Pts',(0.459267782746466,0.684834102699244,
-1.2419369541283));
#52680=CARTESIAN_POINT('Ctrl Pts',(0.0762141917354068,0.821045699986822,
-1.22607944355235));
#52681=CARTESIAN_POINT('Ctrl Pts',(-0.325366393566878,0.757668367048548,
-1.21022193297641));
#52682=CARTESIAN_POINT('Ctrl Pts',(-0.647853293311223,0.510108571614448,
-1.19436442240046));
#52683=CARTESIAN_POINT('Ctrl Pts',(-0.812852801358185,0.138545905074395,
-1.17850691182452));
#52684=CARTESIAN_POINT('Ctrl Pts',(-0.780255000197183,-0.266696042632859,
-1.16264940124858));
#52685=CARTESIAN_POINT('Ctrl Pts',(-0.55798412627637,-0.607106546919343,
-1.14679189067263));
#52686=CARTESIAN_POINT('Ctrl Pts',(-0.200072258378857,-0.799934832293181,
-1.13093438009669));
#52687=CARTESIAN_POINT('Ctrl Pts',(0.206475401677787,-0.798306052207252,
-1.11507686952075));
#52688=CARTESIAN_POINT('Ctrl Pts',(0.562830722209987,-0.602616148659591,
-1.09921935894481));
#52689=CARTESIAN_POINT('Ctrl Pts',(0.782366884264238,-0.260435602204081,
-1.08336184836886));
#52690=CARTESIAN_POINT('Ctrl Pts',(0.811716593266069,0.145054530109405,
-1.06750433779292));
#52691=CARTESIAN_POINT('Ctrl Pts',(0.643745195173435,0.51528319221555,-1.05164682721697));
#52692=CARTESIAN_POINT('Ctrl Pts',(0.31928504761806,0.760251078826112,-1.03578931664103));
#52693=CARTESIAN_POINT('Ctrl Pts',(-0.0827904642126807,0.82040866860619,
-1.01993180606509));
#52694=CARTESIAN_POINT('Ctrl Pts',(-0.464740348218594,0.681132184841088,
-1.00407429548914));
#52695=CARTESIAN_POINT('Ctrl Pts',(-0.733715973988661,0.376278505900353,
-0.988216784913199));
#52696=CARTESIAN_POINT('Ctrl Pts',(-0.824331751652386,-0.0200451417167169,
-0.972359274337258));
#52697=CARTESIAN_POINT('Ctrl Pts',(-0.714559789064689,-0.411495993103893,
-0.956501763761311));
#52698=CARTESIAN_POINT('Ctrl Pts',(-0.431084677085769,-0.702915816915933,
-0.94064425318537));
#52699=CARTESIAN_POINT('Ctrl Pts',(-0.0428167021301743,-0.823463037729944,
-0.924786742609425));
#52700=CARTESIAN_POINT('Ctrl Pts',(0.355859633497782,-0.743833694945016,
-0.908929232033482));
#52701=CARTESIAN_POINT('Ctrl Pts',(0.668029647295509,-0.483384975793587,
-0.89307172145754));
#52702=CARTESIAN_POINT('Ctrl Pts',(0.817807576627052,-0.105429654747237,
-0.877214210881595));
#52703=CARTESIAN_POINT('Ctrl Pts',(0.768783734812105,0.298154680622465,
-0.861356700305653));
#52704=CARTESIAN_POINT('Ctrl Pts',(0.532875383147527,0.629260256590315,
-0.845499189729709));
#52705=CARTESIAN_POINT('Ctrl Pts',(0.16742975034523,0.807398243240637,-0.829641679153766));
#52706=CARTESIAN_POINT('Ctrl Pts',(-0.238716570323675,0.789264875400923,
-0.813784168577821));
#52707=CARTESIAN_POINT('Ctrl Pts',(-0.586833009222479,0.57926821402147,
-0.797926658001879));
#52708=CARTESIAN_POINT('Ctrl Pts',(-0.792295546476325,0.228456585640494,
-0.782069147425936));
#52709=CARTESIAN_POINT('Ctrl Pts',(-0.805158060922119,-0.177890813199751,
-0.766211636849992));
#52710=CARTESIAN_POINT('Ctrl Pts',(-0.622293789337913,-0.540994532541866,
-0.750354126274048));
#52711=CARTESIAN_POINT('Ctrl Pts',(-0.288155414860119,-0.772587277513375,
-0.734496615698105));
#52712=CARTESIAN_POINT('Ctrl Pts',(0.116030986166798,-0.816370905127008,
-0.718639105122162));
#52713=CARTESIAN_POINT('Ctrl Pts',(0.492011283194322,-0.661702003698199,
-0.702781594546217));
#52714=CARTESIAN_POINT('Ctrl Pts',(0.748387999479165,-0.346179211860426,
-0.686924083970274));
#52715=CARTESIAN_POINT('Ctrl Pts',(0.82283822834399,0.053496677134739,-0.671066573394332));
#52716=CARTESIAN_POINT('Ctrl Pts',(0.697263779231996,0.440167998223232,
-0.655209062818386));
#52717=CARTESIAN_POINT('Ctrl Pts',(0.402190687371641,0.719838381499804,
-0.639351552242445));
#52718=CARTESIAN_POINT('Ctrl Pts',(0.00934860525825762,0.824522436364503,
-0.623494041666501));
#52719=CARTESIAN_POINT('Ctrl Pts',(-0.385766039908107,0.728772397214898,
-0.607636531090558));
#52720=CARTESIAN_POINT('Ctrl Pts',(-0.687104380997915,0.455864249642597,
-0.591779020514614));
#52721=CARTESIAN_POINT('Ctrl Pts',(-0.821413738976212,0.0721395447022476,
-0.575921509938671));
#52722=CARTESIAN_POINT('Ctrl Pts',(-0.756044699713402,-0.329121643961638,
-0.560063999362728));
#52723=CARTESIAN_POINT('Ctrl Pts',(-0.506887897088375,-0.650376278990902,
-0.544206488786783));
#52724=CARTESIAN_POINT('Ctrl Pts',(-0.134511140780029,-0.813530206872971,
-0.528348978210842));
#52725=CARTESIAN_POINT('Ctrl Pts',(0.270564081268103,-0.778922154272384,
-0.512491467634896));
#52726=CARTESIAN_POINT('Ctrl Pts',(0.609867573997332,-0.554965031939134,
-0.496633957058954));
#52727=CARTESIAN_POINT('Ctrl Pts',(0.800917666611022,-0.196100830695248,
-0.480776446483009));
#52728=CARTESIAN_POINT('Ctrl Pts',(0.797271775455493,0.210433743849107,
-0.464918935907067));
#52729=CARTESIAN_POINT('Ctrl Pts',(0.599816184347909,0.565813740981475,
-0.449061425331122));
#52730=CARTESIAN_POINT('Ctrl Pts',(0.256550596829474,0.783649434221335,
-0.43320391475518));
#52731=CARTESIAN_POINT('Ctrl Pts',(-0.149080166180136,0.810986897883099,
-0.417346404179236));
#52732=CARTESIAN_POINT('Ctrl Pts',(-0.518470862554774,0.641180636932909,
-0.401488893603293));
#52733=CARTESIAN_POINT('Ctrl Pts',(-0.761825889017629,0.315509047882063,
-0.385631383027349));
#52734=CARTESIAN_POINT('Ctrl Pts',(-0.819987796291551,-0.0868599933696644,
-0.369773872451407));
#52735=CARTESIAN_POINT('Ctrl Pts',(-0.678817940276728,-0.468114140372212,
-0.353916361875461));
#52736=CARTESIAN_POINT('Ctrl Pts',(-0.372633461561838,-0.735573890114115,
-0.33805885129952));
#52737=CARTESIAN_POINT('Ctrl Pts',(0.0241349081417215,-0.824222148937965,
-0.322201340723576));
#52738=CARTESIAN_POINT('Ctrl Pts',(0.415036295122669,-0.712509310712441,
-0.306343830147633));
#52739=CARTESIAN_POINT('Ctrl Pts',(0.705046039541136,-0.427591776684167,
-0.290486319571689));
#52740=CARTESIAN_POINT('Ctrl Pts',(0.823665340687052,-0.0387304718595854,
-0.274628808995746));
#52741=CARTESIAN_POINT('Ctrl Pts',(0.742058904165613,0.35954586545316,-0.258771298419802));
#52742=CARTESIAN_POINT('Ctrl Pts',(0.480064519393053,0.670419794212498,
-0.242913787843858));
#52743=CARTESIAN_POINT('Ctrl Pts',(0.101370721449253,0.818320607982799,
-0.227056277267916));
#52744=CARTESIAN_POINT('Ctrl Pts',(-0.301965429834451,0.767294950903153,
-0.211198766691971));
#52745=CARTESIAN_POINT('Ctrl Pts',(-0.631896404326232,0.529746667439074,
-0.195341256116028));
#52746=CARTESIAN_POINT('Ctrl Pts',(-0.808219078736472,0.163421718047794,
-0.179483745540085));
#52747=CARTESIAN_POINT('Ctrl Pts',(-0.78807063935742,-0.242629703983174,
-0.163626234964142));
#52748=CARTESIAN_POINT('Ctrl Pts',(-0.576349647237178,-0.589699797120169,
-0.147768724388197));
#52749=CARTESIAN_POINT('Ctrl Pts',(-0.224522320795394,-0.793419486658044,
-0.131911213812255));
#52750=CARTESIAN_POINT('Ctrl Pts',(0.181882740561737,-0.804265174094747,
-0.116053703236311));
#52751=CARTESIAN_POINT('Ctrl Pts',(0.544076944580878,-0.619602611767352,
-0.100196192660367));
#52752=CARTESIAN_POINT('Ctrl Pts',(0.77400456870953,-0.284317250155574,
-0.0843386820844249));
#52753=CARTESIAN_POINT('Ctrl Pts',(0.815790850594378,0.120077451582211,
-0.0684811715084816));
#52754=CARTESIAN_POINT('Ctrl Pts',(0.659241540883417,0.495293473818102,
-0.0526236609325374));
#52755=CARTESIAN_POINT('Ctrl Pts',(0.342483797368491,0.750086144974063,
-0.0367661503565947));
#52756=CARTESIAN_POINT('Ctrl Pts',(-0.0576246440758148,0.822584922815185,
-0.0209086397806512));
#52757=CARTESIAN_POINT('Ctrl Pts',(-0.314875021606723,0.737530279563956,
-0.0103369660633551));
#52758=CARTESIAN_POINT('Ctrl Pts',(-0.42561232635123,0.666853325445629,
-0.00505112920470729));
#52759=CARTESIAN_POINT('Ctrl Pts',(-0.79104322765544,1.14479096649424E-5,
-0.173133150823705));
#52760=CARTESIAN_POINT('Ctrl Pts',(-0.791002750150416,-0.0787621090845962,
-0.169964178870517));
#52761=CARTESIAN_POINT('Ctrl Pts',(-0.779310325630016,-0.157547413537066,
-0.166795206917329));
#52762=CARTESIAN_POINT('Ctrl Pts',(-0.756141880567222,-0.232799482500845,
-0.163626234964141));
#52763=CARTESIAN_POINT('Ctrl Pts',(-0.717496975317341,-0.358319735028833,
-0.158340398105494));
#52764=CARTESIAN_POINT('Ctrl Pts',(-0.646923311277268,-0.47400976607449,
-0.153054561246846));
#52765=CARTESIAN_POINT('Ctrl Pts',(-0.552998591516937,-0.565808063186967,
-0.147768724388198));
#52766=CARTESIAN_POINT('Ctrl Pts',(-0.459073871756601,-0.657606360299449,
-0.14248288752955));
#52767=CARTESIAN_POINT('Ctrl Pts',(-0.341798096276011,-0.725512923478742,
-0.137197050670903));
#52768=CARTESIAN_POINT('Ctrl Pts',(-0.215426031642858,-0.761273819641176,
-0.131911213812255));
#52769=CARTESIAN_POINT('Ctrl Pts',(-0.0890539670096971,-0.797034715803612,
-0.126625376953607));
#52770=CARTESIAN_POINT('Ctrl Pts',(0.0464143867760402,-0.80064994494918,
-0.121339540094958));
#52771=CARTESIAN_POINT('Ctrl Pts',(0.174514264338762,-0.771680465800725,
-0.11605370323631));
#52772=CARTESIAN_POINT('Ctrl Pts',(0.302614141901469,-0.742710986652273,
-0.110767866377662));
#52773=CARTESIAN_POINT('Ctrl Pts',(0.423345543241174,-0.681156799209811,
-0.105482029519015));
#52774=CARTESIAN_POINT('Ctrl Pts',(0.522032514599136,-0.594498811886617,
-0.100196192660367));
#52775=CARTESIAN_POINT('Ctrl Pts',(0.620719485957098,-0.507840824563423,
-0.0949103558017196));
#52776=CARTESIAN_POINT('Ctrl Pts',(0.697362027333311,-0.396079037359503,
-0.0896245189430725));
#52777=CARTESIAN_POINT('Ctrl Pts',(0.74264767833556,-0.272799026801247,
-0.084338682084425));
#52778=CARTESIAN_POINT('Ctrl Pts',(0.780454516535908,-0.169878403836554,
-0.0799257880562837));
#52779=CARTESIAN_POINT('Ctrl Pts',(0.796406271019666,-0.0589298248892024,
-0.0755128940281423));
#52780=CARTESIAN_POINT('Ctrl Pts',(0.789514313045754,0.0505148300805575,
-0.0711000000000008));
#52781=CARTESIAN_POINT('',(-0.392914465807693,-0.550975791759097,-5.8089));
#52782=CARTESIAN_POINT('Ctrl Pts',(-0.392914465807689,-0.5509757917591,
-5.8089));
#52783=CARTESIAN_POINT('Ctrl Pts',(-0.408980926181822,-0.541406672716214,
-5.8089));
#52784=CARTESIAN_POINT('Ctrl Pts',(-0.424624980889038,-0.531181210689783,
-5.8089));
#52785=CARTESIAN_POINT('Ctrl Pts',(-0.439803506503688,-0.520323148404966,
-5.8089));
#52786=CARTESIAN_POINT('Ctrl Pts',(-0.463323139664173,-0.503498217693243,
-5.8089));
#52787=CARTESIAN_POINT('Ctrl Pts',(-0.485725932404054,-0.485155747624265,
-5.8089));
#52788=CARTESIAN_POINT('Ctrl Pts',(-0.50691755469692,-0.465448611131913,
-5.8089));
#52789=CARTESIAN_POINT('Ctrl Pts',(-0.514827455118625,-0.458092803959758,
-5.8089));
#52790=CARTESIAN_POINT('Ctrl Pts',(-0.522568471664888,-0.450546591655005,
-5.8089));
#52791=CARTESIAN_POINT('Ctrl Pts',(-0.530135111219165,-0.442816995778067,
-5.8089));
#52792=CARTESIAN_POINT('Ctrl Pts',(-0.53611345887652,-0.436709897498611,
-5.8089));
#52793=CARTESIAN_POINT('Ctrl Pts',(-0.541980440975214,-0.430490694480234,
-5.8089));
#52794=CARTESIAN_POINT('Ctrl Pts',(-0.547726899698063,-0.424170679860769,
-5.8089));
#52795=CARTESIAN_POINT('Ctrl Pts',(-0.570445604559277,-0.399184413747471,
-5.8089));
#52796=CARTESIAN_POINT('Ctrl Pts',(-0.591314828543991,-0.372593498230057,
-5.8089));
#52797=CARTESIAN_POINT('Ctrl Pts',(-0.610184365647462,-0.344628549984071,
-5.8089));
#52798=CARTESIAN_POINT('Ctrl Pts',(-0.617410130397325,-0.333919853943486,
-5.8089));
#52799=CARTESIAN_POINT('Ctrl Pts',(-0.624342346784469,-0.32300922386781,
-5.8089));
#52800=CARTESIAN_POINT('Ctrl Pts',(-0.630971222773021,-0.311908104829863,
-5.8089));
#52801=CARTESIAN_POINT('Ctrl Pts',(-0.63528392404581,-0.304685792889344,
-5.8089));
#52802=CARTESIAN_POINT('Ctrl Pts',(-0.639468933149375,-0.297381521670017,
-5.8089));
#52803=CARTESIAN_POINT('Ctrl Pts',(-0.64352110345146,-0.290002386427528,
-5.8089));
#52804=CARTESIAN_POINT('Ctrl Pts',(-0.649505567320399,-0.279104481119854,
-5.8089));
#52805=CARTESIAN_POINT('Ctrl Pts',(-0.655190978687311,-0.268060576369735,
-5.8089));
#52806=CARTESIAN_POINT('Ctrl Pts',(-0.660570869537721,-0.256882390369936,
-5.8089));
#52807=CARTESIAN_POINT('Ctrl Pts',(-0.675323401225404,-0.226229994669333,
-5.8089));
#52808=CARTESIAN_POINT('Ctrl Pts',(-0.687781723263565,-0.194570433662548,
-5.8089));
#52809=CARTESIAN_POINT('Ctrl Pts',(-0.697948790393408,-0.162181035562999,
-5.8089));
#52810=CARTESIAN_POINT('Ctrl Pts',(-0.708208146688207,-0.129497630306234,
-5.8089));
#52811=CARTESIAN_POINT('Ctrl Pts',(-0.716134890556743,-0.0960699249494282,
-5.8089));
#52812=CARTESIAN_POINT('Ctrl Pts',(-0.72168597652701,-0.0621561899810933,
-5.8089));
#52813=CARTESIAN_POINT('Ctrl Pts',(-0.723441122832596,-0.0514333211663941,
-5.8089));
#52814=CARTESIAN_POINT('Ctrl Pts',(-0.724958404602569,-0.0406617363995879,
-5.8089));
#52815=CARTESIAN_POINT('Ctrl Pts',(-0.726235405139263,-0.0298493434138636,
-5.8089));
#52816=CARTESIAN_POINT('Ctrl Pts',(-0.727115833463151,-0.0223947364970243,
-5.8089));
#52817=CARTESIAN_POINT('Ctrl Pts',(-0.727881038038328,-0.0149287234917137,
-5.8089));
#52818=CARTESIAN_POINT('Ctrl Pts',(-0.728530533992226,-0.00745907930554179,
-5.8089));
#52819=CARTESIAN_POINT('Ctrl Pts',(-0.731453588396324,0.0261580297840189,
-5.8089));
#52820=CARTESIAN_POINT('Ctrl Pts',(-0.732040069074509,0.0598791137304111,
-5.8089));
#52821=CARTESIAN_POINT('Ctrl Pts',(-0.730275016954016,0.0934581668363401,
-5.8089));
#52822=CARTESIAN_POINT('Ctrl Pts',(-0.728639353757938,0.124575673615201,
-5.8089));
#52823=CARTESIAN_POINT('Ctrl Pts',(-0.724984137270265,0.155572115372472,
-5.8089));
#52824=CARTESIAN_POINT('Ctrl Pts',(-0.719387035599625,0.186273529871663,
-5.8089));
#52825=CARTESIAN_POINT('Ctrl Pts',(-0.716174207421376,0.203896645444594,
-5.8089));
#52826=CARTESIAN_POINT('Ctrl Pts',(-0.712320910059993,0.221422620213725,
-5.8089));
#52827=CARTESIAN_POINT('Ctrl Pts',(-0.707836932295669,0.238818219202657,
-5.8089));
#52828=CARTESIAN_POINT('Ctrl Pts',(-0.705076172277217,0.249528592159403,
-5.8089));
#52829=CARTESIAN_POINT('Ctrl Pts',(-0.70207408761155,0.260195841798999,
-5.8089));
#52830=CARTESIAN_POINT('Ctrl Pts',(-0.698843635371611,0.270777419289408,
-5.8089));
#52831=CARTESIAN_POINT('Ctrl Pts',(-0.68835492234885,0.305133949391549,
-5.8089));
#52832=CARTESIAN_POINT('Ctrl Pts',(-0.675451834043792,0.338642319424662,
-5.8089));
#52833=CARTESIAN_POINT('Ctrl Pts',(-0.66026439737455,0.371047946919152,
-5.8089));
#52834=CARTESIAN_POINT('Ctrl Pts',(-0.648020670392897,0.397172543475675,
-5.8089));
#52835=CARTESIAN_POINT('Ctrl Pts',(-0.634291186315133,0.422580902638274,
-5.8089));
#52836=CARTESIAN_POINT('Ctrl Pts',(-0.619119721284794,0.447135948712967,
-5.8089));
#52837=CARTESIAN_POINT('Ctrl Pts',(-0.610224791501901,0.46153241011029,
-5.8089));
#52838=CARTESIAN_POINT('Ctrl Pts',(-0.600833791321736,0.475635447480755,
-5.8089));
#52839=CARTESIAN_POINT('Ctrl Pts',(-0.590967220284706,0.489427201169085,
-5.8089));
#52840=CARTESIAN_POINT('Ctrl Pts',(-0.585636455339572,0.496878685257906,
-5.8089));
#52841=CARTESIAN_POINT('Ctrl Pts',(-0.580166827791742,0.504239280109289,
-5.8089));
#52842=CARTESIAN_POINT('Ctrl Pts',(-0.57456130958788,0.511505986352523,
-5.8089));
#52843=CARTESIAN_POINT('Ctrl Pts',(-0.570041164021464,0.517365671186865,
-5.8089));
#52844=CARTESIAN_POINT('Ctrl Pts',(-0.565432977871958,0.523163672746738,
-5.8089));
#52845=CARTESIAN_POINT('Ctrl Pts',(-0.560747049034941,0.528888278685951,
-5.8089));
#52846=CARTESIAN_POINT('Ctrl Pts',(-0.537735453820515,0.55700059520144,
-5.8089));
#52847=CARTESIAN_POINT('Ctrl Pts',(-0.512802538579046,0.58341098831171,
-5.8089));
#52848=CARTESIAN_POINT('Ctrl Pts',(-0.48618644515188,0.607969808368677,
-5.8089));
#52849=CARTESIAN_POINT('Ctrl Pts',(-0.459352739467097,0.632729420487471,
-5.8089));
#52850=CARTESIAN_POINT('Ctrl Pts',(-0.430807455342091,0.655608007637476,
-5.8089));
#52851=CARTESIAN_POINT('Ctrl Pts',(-0.400750465327347,0.676424420620533,
-5.8089));
#52852=CARTESIAN_POINT('Ctrl Pts',(-0.381778290006706,0.689563881240766,
-5.8089));
#52853=CARTESIAN_POINT('Ctrl Pts',(-0.362202973049296,0.701881127216335,
-5.8089));
#52854=CARTESIAN_POINT('Ctrl Pts',(-0.342067962509752,0.713322310757506,
-5.8089));
#52855=CARTESIAN_POINT('Ctrl Pts',(-0.392914465807693,-0.550975791759097,
-5.8089));
#52856=CARTESIAN_POINT('Ctrl Pts',(-0.316486804163133,-0.605362341937418,
-5.80448710597186));
#52857=CARTESIAN_POINT('Ctrl Pts',(-0.123459254944096,-0.689898673908607,
-5.79478837508506));
#52858=CARTESIAN_POINT('Ctrl Pts',(0.204815806457288,-0.674943835808658,
-5.77980380733964));
#52859=CARTESIAN_POINT('Ctrl Pts',(0.502426729513632,-0.495039039708356,
-5.76394629676369));
#52860=CARTESIAN_POINT('Ctrl Pts',(0.677901792498161,-0.194797654574707,
-5.74808878618775));
#52861=CARTESIAN_POINT('Ctrl Pts',(0.688585132880224,0.152798855491627,
-5.7322312756118));
#52862=CARTESIAN_POINT('Ctrl Pts',(0.531879433776216,0.463250529001845,
-5.71637376503586));
#52863=CARTESIAN_POINT('Ctrl Pts',(0.245878610535506,0.661090510301056,
-5.70051625445991));
#52864=CARTESIAN_POINT('Ctrl Pts',(-0.0998931488246837,0.698225042897434,
-5.68465874388397));
#52865=CARTESIAN_POINT('Ctrl Pts',(-0.421381756118886,0.565627364000294,
-5.66880123330803));
#52866=CARTESIAN_POINT('Ctrl Pts',(-0.630785750431968,0.307429753987566,
-5.65364232588638));
#52867=CARTESIAN_POINT('Ctrl Pts',(-0.676646139866951,0.0974912420182623,
-5.64376925532336));
#52868=CARTESIAN_POINT('Ctrl Pts',(-0.676733793626987,-1.34876458775003E-5,
-5.639182021619));
#52869=CARTESIAN_POINT('Origin',(-1.87869726832665E-16,-4.25270154953079E-17,
-5.8089));
#52870=CARTESIAN_POINT('',(-0.7911,-9.68818082805472E-17,-5.8089));
#52871=CARTESIAN_POINT('Origin',(0.,0.,-5.8089));
#52872=CARTESIAN_POINT('Origin',(0.,0.,-5.8089));
#52873=CARTESIAN_POINT('',(0.392888236737269,-0.550964357679769,-5.8089));
#52874=CARTESIAN_POINT('Ctrl Pts',(0.342095882030763,0.713340734875808,
-5.8089));
#52875=CARTESIAN_POINT('Ctrl Pts',(0.360978708681145,0.702635258820052,
-5.8089));
#52876=CARTESIAN_POINT('Ctrl Pts',(0.379389322783699,0.69116424080316,-5.8089));
#52877=CARTESIAN_POINT('Ctrl Pts',(0.397274912114345,0.678942925746265,
-5.8089));
#52878=CARTESIAN_POINT('Ctrl Pts',(0.423819765578583,0.660804691029575,
-5.8089));
#52879=CARTESIAN_POINT('Ctrl Pts',(0.449209359364097,0.641014492048834,
-5.8089));
#52880=CARTESIAN_POINT('Ctrl Pts',(0.47331366889555,0.619707152111731,-5.8089));
#52881=CARTESIAN_POINT('Ctrl Pts',(0.482766815899108,0.611350911232175,
-5.8089));
#52882=CARTESIAN_POINT('Ctrl Pts',(0.492022026358695,0.602761124068153,
-5.8089));
#52883=CARTESIAN_POINT('Ctrl Pts',(0.501070383515418,0.593945229113476,
-5.8089));
#52884=CARTESIAN_POINT('Ctrl Pts',(0.507461516366784,0.587718291462461,
-5.8089));
#52885=CARTESIAN_POINT('Ctrl Pts',(0.513748498043816,0.581379258677312,
-5.8089));
#52886=CARTESIAN_POINT('Ctrl Pts',(0.519919868452944,0.574939912035177,
-5.8089));
#52887=CARTESIAN_POINT('Ctrl Pts',(0.545883770341496,0.547848593031625,
-5.8089));
#52888=CARTESIAN_POINT('Ctrl Pts',(0.569847963303607,0.518943292978646,
-5.8089));
#52889=CARTESIAN_POINT('Ctrl Pts',(0.59159745395337,0.488437514575107,-5.8089));
#52890=CARTESIAN_POINT('Ctrl Pts',(0.604843734393337,0.469858316455947,
-5.8089));
#52891=CARTESIAN_POINT('Ctrl Pts',(0.617267589027075,0.450684778561505,
-5.8089));
#52892=CARTESIAN_POINT('Ctrl Pts',(0.628810161645074,0.430960931745118,
-5.8089));
#52893=CARTESIAN_POINT('Ctrl Pts',(0.6331957498372,0.423466877121077,-5.8089));
#52894=CARTESIAN_POINT('Ctrl Pts',(0.637450247091553,0.415899644987057,
-5.8089));
#52895=CARTESIAN_POINT('Ctrl Pts',(0.641567501202037,0.408268535811919,
-5.8089));
#52896=CARTESIAN_POINT('Ctrl Pts',(0.644406436656658,0.403006721550756,
-5.8089));
#52897=CARTESIAN_POINT('Ctrl Pts',(0.647180685228449,0.3977135715039,-5.8089));
#52898=CARTESIAN_POINT('Ctrl Pts',(0.649889438922888,0.39238997845085,-5.8089));
#52899=CARTESIAN_POINT('Ctrl Pts',(0.666049099676394,0.360630923390353,
-5.8089));
#52900=CARTESIAN_POINT('Ctrl Pts',(0.679881889293971,0.327789779259877,
-5.8089));
#52901=CARTESIAN_POINT('Ctrl Pts',(0.69133700537052,0.294133909535164,-5.8089));
#52902=CARTESIAN_POINT('Ctrl Pts',(0.702691657190659,0.260773210274299,
-5.8089));
#52903=CARTESIAN_POINT('Ctrl Pts',(0.711710261928255,0.226610762787482,
-5.8089));
#52904=CARTESIAN_POINT('Ctrl Pts',(0.718293067787738,0.19190153845702,-5.8089));
#52905=CARTESIAN_POINT('Ctrl Pts',(0.720274770820946,0.181452593644697,
-5.8089));
#52906=CARTESIAN_POINT('Ctrl Pts',(0.722035372085814,0.170954128586943,
-5.8089));
#52907=CARTESIAN_POINT('Ctrl Pts',(0.723571223099844,0.160413260727799,
-5.8089));
#52908=CARTESIAN_POINT('Ctrl Pts',(0.724609888773418,0.153284680211231,
-5.8089));
#52909=CARTESIAN_POINT('Ctrl Pts',(0.725545495635983,0.146137630688022,
-5.8089));
#52910=CARTESIAN_POINT('Ctrl Pts',(0.726375786214834,0.138987023116276,
-5.8089));
#52911=CARTESIAN_POINT('Ctrl Pts',(0.730471171823078,0.103716846523315,
-5.8089));
#52912=CARTESIAN_POINT('Ctrl Pts',(0.732021347863029,0.0682782853423011,
-5.8089));
#52913=CARTESIAN_POINT('Ctrl Pts',(0.730953058964537,0.032934252799972,
-5.8089));
#52914=CARTESIAN_POINT('Ctrl Pts',(0.730050923290943,0.00308735216280863,
-5.8089));
#52915=CARTESIAN_POINT('Ctrl Pts',(0.727280342640496,-0.0266927166244539,
-5.8089));
#52916=CARTESIAN_POINT('Ctrl Pts',(0.722676929026824,-0.0562354887167472,
-5.8089));
#52917=CARTESIAN_POINT('Ctrl Pts',(0.720230454191575,-0.0719359350708675,
-5.8089));
#52918=CARTESIAN_POINT('Ctrl Pts',(0.717265866279696,-0.0875692069311204,
-5.8089));
#52919=CARTESIAN_POINT('Ctrl Pts',(0.713785605356316,-0.103108175325424,
-5.8089));
#52920=CARTESIAN_POINT('Ctrl Pts',(0.712112783672321,-0.110577133501022,
-5.8089));
#52921=CARTESIAN_POINT('Ctrl Pts',(0.710320795535734,-0.11802428479304,
-5.8089));
#52922=CARTESIAN_POINT('Ctrl Pts',(0.708409758051769,-0.125446495005051,
-5.8089));
#52923=CARTESIAN_POINT('Ctrl Pts',(0.706492764579635,-0.132891837466731,
-5.8089));
#52924=CARTESIAN_POINT('Ctrl Pts',(0.704458175001798,-0.140303361495487,
-5.8089));
#52925=CARTESIAN_POINT('Ctrl Pts',(0.702308221058893,-0.147673812311276,
-5.8089));
#52926=CARTESIAN_POINT('Ctrl Pts',(0.692801581982461,-0.1802643782476,-5.8089));
#52927=CARTESIAN_POINT('Ctrl Pts',(0.681035781348705,-0.212081758477362,
-5.8089));
#52928=CARTESIAN_POINT('Ctrl Pts',(0.667074534284358,-0.242877043678588,
-5.8089));
#52929=CARTESIAN_POINT('Ctrl Pts',(0.656923567387669,-0.265267731216093,
-5.8089));
#52930=CARTESIAN_POINT('Ctrl Pts',(0.645610925501866,-0.287117873412337,
-5.8089));
#52931=CARTESIAN_POINT('Ctrl Pts',(0.633146702390696,-0.308322081618923,
-5.8089));
#52932=CARTESIAN_POINT('Ctrl Pts',(0.625027380935961,-0.322134718081451,
-5.8089));
#52933=CARTESIAN_POINT('Ctrl Pts',(0.616419131041242,-0.335673062825433,
-5.8089));
#52934=CARTESIAN_POINT('Ctrl Pts',(0.607339031883614,-0.348913919627164,
-5.8089));
#52935=CARTESIAN_POINT('Ctrl Pts',(0.602580680409358,-0.355852682011713,
-5.8089));
#52936=CARTESIAN_POINT('Ctrl Pts',(0.597692725339706,-0.362709713037344,
-5.8089));
#52937=CARTESIAN_POINT('Ctrl Pts',(0.592677481645101,-0.369481424925529,
-5.8089));
#52938=CARTESIAN_POINT('Ctrl Pts',(0.588934360991923,-0.374535483346122,
-5.8089));
#52939=CARTESIAN_POINT('Ctrl Pts',(0.585121098221576,-0.379540835606088,
-5.8089));
#52940=CARTESIAN_POINT('Ctrl Pts',(0.581244810866683,-0.384488631805347,
-5.8089));
#52941=CARTESIAN_POINT('Ctrl Pts',(0.56068130673256,-0.410736434995127,
-5.8089));
#52942=CARTESIAN_POINT('Ctrl Pts',(0.53830293915685,-0.435427816819282,
-5.8089));
#52943=CARTESIAN_POINT('Ctrl Pts',(0.514295529224174,-0.45838419708911,
-5.8089));
#52944=CARTESIAN_POINT('Ctrl Pts',(0.490732143299865,-0.480915992448961,
-5.8089));
#52945=CARTESIAN_POINT('Ctrl Pts',(0.465598395457484,-0.501777006704631,
-5.8089));
#52946=CARTESIAN_POINT('Ctrl Pts',(0.439043415987534,-0.52075707530173,
-5.8089));
#52947=CARTESIAN_POINT('Ctrl Pts',(0.424100596267082,-0.531437397749323,
-5.8089));
#52948=CARTESIAN_POINT('Ctrl Pts',(0.408707354130667,-0.541521326150454,
-5.8089));
#52949=CARTESIAN_POINT('Ctrl Pts',(0.392888236737257,-0.550964357679777,
-5.8089));
#52950=CARTESIAN_POINT('Origin',(0.,0.,-5.8089));
#52951=CARTESIAN_POINT('Origin',(0.,0.,-6.17861797838101));
#52952=CARTESIAN_POINT('Ctrl Pts',(0.392888236737257,-0.550964357679777,
-5.8089));
#52953=CARTESIAN_POINT('Ctrl Pts',(0.484381081792765,-0.485721548291323,
-5.80361416314135));
#52954=CARTESIAN_POINT('Ctrl Pts',(0.634146933675295,-0.308844853941977,
-5.79304248942406));
#52955=CARTESIAN_POINT('Ctrl Pts',(0.70461890056211,0.0317634872067408,
-5.77718497884811));
#52956=CARTESIAN_POINT('Ctrl Pts',(0.603809517943593,0.364559903875637,
-5.76132746827217));
#52957=CARTESIAN_POINT('Ctrl Pts',(0.356217202446025,0.608779534529828,
-5.74546995769622));
#52958=CARTESIAN_POINT('Ctrl Pts',(0.0220327184609351,0.704987657002684,
-5.72961244712028));
#52959=CARTESIAN_POINT('Ctrl Pts',(-0.317508269912238,0.629831081602948,
-5.71375493654434));
#52960=CARTESIAN_POINT('Ctrl Pts',(-0.5798655339509,0.401562243999013,-5.6978974259684));
#52961=CARTESIAN_POINT('Ctrl Pts',(-0.669529242576081,0.160866553025884,
-5.68618510658062));
#52962=CARTESIAN_POINT('Ctrl Pts',(-0.676730232498528,0.024265518019747,
-5.67975862405149));
#52963=CARTESIAN_POINT('Ctrl Pts',(-0.676705286336412,1.73782512660377E-5,
-5.678617978381));
#52964=CARTESIAN_POINT('Ctrl Pts',(0.459308237155092,-0.644108029201221,
-5.87494887079529));
#52965=CARTESIAN_POINT('Ctrl Pts',(0.566268470232396,-0.567835550248648,
-5.86966303393665));
#52966=CARTESIAN_POINT('Ctrl Pts',(0.741353094769514,-0.361056840480996,
-5.85909136021935));
#52967=CARTESIAN_POINT('Ctrl Pts',(0.823738750162087,0.0371332861375223,
-5.8432338496434));
#52968=CARTESIAN_POINT('Ctrl Pts',(0.705886965634953,0.426190837824773,
-5.82737633906747));
#52969=CARTESIAN_POINT('Ctrl Pts',(0.416437755068778,0.711697191911558,
-5.81151882849151));
#52970=CARTESIAN_POINT('Ctrl Pts',(0.0257574753575252,0.824169846985109,
-5.79566131791559));
#52971=CARTESIAN_POINT('Ctrl Pts',(-0.371184856402511,0.736307623254158,
-5.77980380733962));
#52972=CARTESIAN_POINT('Ctrl Pts',(-0.677895114391254,0.469448634886378,
-5.7639462967637));
#52973=CARTESIAN_POINT('Ctrl Pts',(-0.819815247198737,0.0884743817256807,
-5.74808878618774));
#52974=CARTESIAN_POINT('Ctrl Pts',(-0.762445476544219,-0.314009019036856,
-5.73223127561181));
#52975=CARTESIAN_POINT('Ctrl Pts',(-0.519732014137197,-0.640158685018968,
-5.71637376503586));
#52976=CARTESIAN_POINT('Ctrl Pts',(-0.150676284699232,-0.810691924431145,
-5.70051625445991));
#52977=CARTESIAN_POINT('Ctrl Pts',(0.255007502195102,-0.78415290202513,
-5.68465874388398));
#52978=CARTESIAN_POINT('Ctrl Pts',(0.598701232077407,-0.566993385664642,
-5.66880123330802));
#52979=CARTESIAN_POINT('Ctrl Pts',(0.796855997564115,-0.212002740690496,
-5.65294372273209));
#52980=CARTESIAN_POINT('Ctrl Pts',(0.801302136551466,0.194523858387913,
-5.63708621215614));
#52981=CARTESIAN_POINT('Ctrl Pts',(0.610958829750896,0.553763448800768,
-5.6212287015802));
#52982=CARTESIAN_POINT('Ctrl Pts',(0.272096848637962,0.778388045989811,
-5.60537119100425));
#52983=CARTESIAN_POINT('Ctrl Pts',(-0.132909464157486,0.813793414795239,
-5.58951368042832));
#52984=CARTESIAN_POINT('Ctrl Pts',(-0.505606664494294,0.651372817373753,
-5.57365616985236));
#52985=CARTESIAN_POINT('Ctrl Pts',(-0.755395367485779,0.330609264301904,
-5.55779865927643));
#52986=CARTESIAN_POINT('Ctrl Pts',(-0.821554153994998,-0.0705224703046039,
-5.54194114870049));
#52987=CARTESIAN_POINT('Ctrl Pts',(-0.688000409631081,-0.454510817337334,
-5.52608363812453));
#52988=CARTESIAN_POINT('Ctrl Pts',(-0.387199865531956,-0.728011614548961,
-5.5102261275486));
#52989=CARTESIAN_POINT('Ctrl Pts',(0.00772553293681073,-0.824539242780456,
-5.49436861697264));
#52990=CARTESIAN_POINT('Ctrl Pts',(0.400772922845576,-0.720628691547045,
-5.47851110639671));
#52991=CARTESIAN_POINT('Ctrl Pts',(0.696395968486637,-0.441539694515675,
-5.46265359582076));
#52992=CARTESIAN_POINT('Ctrl Pts',(0.822731328477964,-0.05511631247575,
-5.44679608524482));
#52993=CARTESIAN_POINT('Ctrl Pts',(0.74906799690187,0.344705356467844,-5.43093857466887));
#52994=CARTESIAN_POINT('Ctrl Pts',(0.493312876561327,0.660732209429935,
-5.41508106409294));
#52995=CARTESIAN_POINT('Ctrl Pts',(0.117637769670523,0.816140920372838,
-5.39922355351699));
#52996=CARTESIAN_POINT('Ctrl Pts',(-0.286634036043552,0.773153009527251,
-5.38336604294105));
#52997=CARTESIAN_POINT('Ctrl Pts',(-0.621227648910197,0.542218456887407,
-5.3675085323651));
#52998=CARTESIAN_POINT('Ctrl Pts',(-0.804806328168754,0.179475404719749,
-5.35165102178917));
#52999=CARTESIAN_POINT('Ctrl Pts',(-0.792743724511181,-0.226896527095366,
-5.33579351121321));
#53000=CARTESIAN_POINT('Ctrl Pts',(-0.587972149938848,-0.578111924852009,
-5.31993600063728));
#53001=CARTESIAN_POINT('Ctrl Pts',(-0.240269758713106,-0.788793439252471,
-5.30407849006133));
#53002=CARTESIAN_POINT('Ctrl Pts',(0.165840080609549,-0.807726262061115,
-5.28822097948539));
#53003=CARTESIAN_POINT('Ctrl Pts',(0.531635666684229,-0.630307991912695,
-5.27236346890943));
#53004=CARTESIAN_POINT('Ctrl Pts',(0.76819533570202,-0.299667437279164,
-5.25650595833351));
#53005=CARTESIAN_POINT('Ctrl Pts',(0.818013529477059,0.103819614487269,
-5.24064844775755));
#53006=CARTESIAN_POINT('Ctrl Pts',(0.668979886793761,0.482069038442842,
-5.22479093718162));
#53007=CARTESIAN_POINT('Ctrl Pts',(0.357323164847127,0.743131753206276,
-5.20893342660566));
#53008=CARTESIAN_POINT('Ctrl Pts',(-0.041195650425007,0.823545727416433,
-5.19307591602973));
#53009=CARTESIAN_POINT('Ctrl Pts',(-0.429700168321956,0.703763036897992,
-5.17721840545378));
#53010=CARTESIAN_POINT('Ctrl Pts',(-0.713748385047573,0.412901791715392,
-5.16136089487784));
#53011=CARTESIAN_POINT('Ctrl Pts',(-0.824290697504572,0.0216677817790976,
-5.1455033843019));
#53012=CARTESIAN_POINT('Ctrl Pts',(-0.734455249609499,-0.37483347379983,
-5.12964587372595));
#53013=CARTESIAN_POINT('Ctrl Pts',(-0.466080242259121,-0.68021603519432,
-5.11378836315001));
#53014=CARTESIAN_POINT('Ctrl Pts',(-0.0844052603112262,-0.82024410926967,
-5.09793085257406));
#53015=CARTESIAN_POINT('Ctrl Pts',(0.317787892076171,-0.760878112715554,
-5.08207334199813));
#53016=CARTESIAN_POINT('Ctrl Pts',(0.642729625426568,-0.516549392951754,
-5.06621583142217));
#53017=CARTESIAN_POINT('Ctrl Pts',(0.811429485315579,-0.146652095519609,
-5.05035832084624));
#53018=CARTESIAN_POINT('Ctrl Pts',(0.782878031507377,0.258895026106984,
-5.03450081027029));
#53019=CARTESIAN_POINT('Ctrl Pts',(0.564015869283808,0.601507062265964,
-5.01864329969435));
#53020=CARTESIAN_POINT('Ctrl Pts',(0.208046449836234,0.797898064586159,
-5.0027857891184));
#53021=CARTESIAN_POINT('Ctrl Pts',(-0.198497217014094,0.800327121618067,
-4.98692827854246));
#53022=CARTESIAN_POINT('Ctrl Pts',(-0.556787970296653,0.608203751133396,
-4.97107076796652));
#53023=CARTESIAN_POINT('Ctrl Pts',(-0.779728504515992,0.26823144111952,
-4.95521325739057));
#53024=CARTESIAN_POINT('Ctrl Pts',(-0.813123952407679,-0.136945554074297,
-4.93935574681463));
#53025=CARTESIAN_POINT('Ctrl Pts',(-0.648856176675305,-0.508832299240237,
-4.92349823623868));
#53026=CARTESIAN_POINT('Ctrl Pts',(-0.326857217191358,-0.75702642379888,
-4.90764072566275));
#53027=CARTESIAN_POINT('Ctrl Pts',(0.0745978338559104,-0.821194136574177,
-4.8917832150868));
#53028=CARTESIAN_POINT('Ctrl Pts',(0.45791881288172,-0.68573683550528,-4.87592570451086));
#53029=CARTESIAN_POINT('Ctrl Pts',(0.729923788431936,-0.383582989509403,
-4.86006819393491));
#53030=CARTESIAN_POINT('Ctrl Pts',(0.824490762562902,0.0118164803661736,
-4.84421068335898));
#53031=CARTESIAN_POINT('Ctrl Pts',(0.718631342299906,0.404343468630367,
-4.82835317278302));
#53032=CARTESIAN_POINT('Ctrl Pts',(0.438079014152841,0.698578144604221,
-4.81249566220709));
#53033=CARTESIAN_POINT('Ctrl Pts',(0.0510335617003136,0.822994667260962,
-4.79663815163113));
#53034=CARTESIAN_POINT('Ctrl Pts',(-0.348417697134908,0.747348483027167,
-4.7807806410552));
#53035=CARTESIAN_POINT('Ctrl Pts',(-0.663171702889056,0.490028508606418,
-4.76492313047925));
#53036=CARTESIAN_POINT('Ctrl Pts',(-0.816714547391389,0.113586948365908,
-4.74906561990331));
#53037=CARTESIAN_POINT('Ctrl Pts',(-0.771721326463556,-0.290466591953583,
-4.73320810932737));
#53038=CARTESIAN_POINT('Ctrl Pts',(-0.539129493200493,-0.623910279063567,
-4.71735059875143));
#53039=CARTESIAN_POINT('Ctrl Pts',(-0.175480060095158,-0.805686908959553,
-4.70149308817548));
#53040=CARTESIAN_POINT('Ctrl Pts',(0.230827019802462,-0.791608194556446,
-4.68563557759954));
#53041=CARTESIAN_POINT('Ctrl Pts',(0.581022097712454,-0.585096546502899,
-4.66977806702359));
#53042=CARTESIAN_POINT('Ctrl Pts',(0.789975855045685,-0.236353115495945,
-4.65392055644765));
#53043=CARTESIAN_POINT('Ctrl Pts',(0.806893485991124,0.169845662367026,
-4.63806304587171));
#53044=CARTESIAN_POINT('Ctrl Pts',(0.627662464458674,0.53475646557051,-4.62220553529576));
#53045=CARTESIAN_POINT('Ctrl Pts',(0.295852262709778,0.769672713177038,
-4.60634802471982));
#53046=CARTESIAN_POINT('Ctrl Pts',(-0.107877001059769,0.81748834817516,
-4.59049051414388));
#53047=CARTESIAN_POINT('Ctrl Pts',(-0.485382322315716,0.666579813633147,
-4.57463300356793));
#53048=CARTESIAN_POINT('Ctrl Pts',(-0.744895504445808,0.353631636333951,
-4.558775492992));
#53049=CARTESIAN_POINT('Ctrl Pts',(-0.823331193733816,-0.0452812564385095,
-4.54291798241604));
#53050=CARTESIAN_POINT('Ctrl Pts',(-0.701622369529403,-0.433186677237131,
-4.5270604718401));
#53051=CARTESIAN_POINT('Ctrl Pts',(-0.409355367918847,-0.715788257458745,
-4.51120296126416));
#53052=CARTESIAN_POINT('Ctrl Pts',(-0.0175777057367246,-0.824388058514212,
-4.49534545068821));
#53053=CARTESIAN_POINT('Ctrl Pts',(0.378472940864992,-0.732586431619373,
-4.47948794011228));
#53054=CARTESIAN_POINT('Ctrl Pts',(0.682520171106463,-0.462699538353568,
-4.46363042953632));
#53055=CARTESIAN_POINT('Ctrl Pts',(0.820652799017158,-0.0803344896361682,
-4.44777291896039));
#53056=CARTESIAN_POINT('Ctrl Pts',(0.759292007444244,0.321559161261329,
-4.43191540838444));
#53057=CARTESIAN_POINT('Ctrl Pts',(0.513354060790599,0.645284631019212,
-4.4160578978085));
#53058=CARTESIAN_POINT('Ctrl Pts',(0.142624293386979,0.812147128108981,
-4.40020038723255));
#53059=CARTESIAN_POINT('Ctrl Pts',(-0.262776175223388,0.781583858901121,
-4.38434287665661));
#53060=CARTESIAN_POINT('Ctrl Pts',(-0.604298085426446,0.561024483164266,
-4.36848536608067));
#53061=CARTESIAN_POINT('Ctrl Pts',(-0.798920488805789,0.204085029647251,
-4.35262785550472));
#53062=CARTESIAN_POINT('Ctrl Pts',(-0.799332404633924,-0.202465685146767,
-4.33677034492878));
#53063=CARTESIAN_POINT('Ctrl Pts',(-0.605433699825102,-0.559798786954642,
-4.32091283435284));
#53064=CARTESIAN_POINT('Ctrl Pts',(-0.264359430400681,-0.781049766863819,
-4.3050553237769));
#53065=CARTESIAN_POINT('Ctrl Pts',(0.140978272727411,-0.812434473282982,
-4.28919781320095));
#53066=CARTESIAN_POINT('Ctrl Pts',(0.512045407677382,-0.646323562340337,
-4.27334030262501));
#53067=CARTESIAN_POINT('Ctrl Pts',(0.758638843846605,-0.323097123736636,
-4.25748279204906));
#53068=CARTESIAN_POINT('Ctrl Pts',(0.820813903214692,0.0786713610487585,
-4.24162528147312));
#53069=CARTESIAN_POINT('Ctrl Pts',(0.683456380097103,0.461315535468256,
-4.22576777089718));
#53070=CARTESIAN_POINT('Ctrl Pts',(0.379956670543603,0.731817993266919,
-4.20991026032123));
#53071=CARTESIAN_POINT('Ctrl Pts',(-0.0159071369001762,0.824421985245081,
-4.19405274974529));
#53072=CARTESIAN_POINT('Ctrl Pts',(-0.407904060397163,0.716616301985455,
-4.17819523916935));
#53073=CARTESIAN_POINT('Ctrl Pts',(-0.700743123313723,0.434607549276735,
-4.1623377285934));
#53074=CARTESIAN_POINT('Ctrl Pts',(-0.823237745783721,0.0469495545957191,
-4.14648021801746));
#53075=CARTESIAN_POINT('Ctrl Pts',(-0.745610571129455,-0.352121460549918,
-4.13062270744151));
#53076=CARTESIAN_POINT('Ctrl Pts',(-0.486732077262139,-0.665594870566085,
-4.11476519686557));
#53077=CARTESIAN_POINT('Ctrl Pts',(-0.109533330808494,-0.817268068752106,
-4.09890768628963));
#53078=CARTESIAN_POINT('Ctrl Pts',(0.294291997235545,-0.770270645372725,
-4.08305017571368));
#53079=CARTESIAN_POINT('Ctrl Pts',(0.62657754996231,-0.536027257369465,
-4.06719266513774));
#53080=CARTESIAN_POINT('Ctrl Pts',(0.806547655567773,-0.171480395549841,
-4.05133515456181));
#53081=CARTESIAN_POINT('Ctrl Pts',(0.790453177005112,0.234751830072363,
-4.03547764398585));
#53082=CARTESIAN_POINT('Ctrl Pts',(0.582206539318293,0.583917967127932,
-4.01962013340992));
#53083=CARTESIAN_POINT('Ctrl Pts',(0.232430653801666,0.791138823426793,
-4.00376262283397));
#53084=CARTESIAN_POINT('Ctrl Pts',(-0.173847062909884,0.806040846035366,
-3.98790511225803));
#53085=CARTESIAN_POINT('Ctrl Pts',(-0.537864099966638,0.625001485379737,
-3.97204760168208));
#53086=CARTESIAN_POINT('Ctrl Pts',(-0.771131143057216,0.292029804929349,
-3.95619009110614));
#53087=CARTESIAN_POINT('Ctrl Pts',(-0.816943042166037,-0.111931731945415,
-3.94033258053019));
#53088=CARTESIAN_POINT('Ctrl Pts',(-0.664163330790826,-0.488683657177766,
-3.92447506995425));
#53089=CARTESIAN_POINT('Ctrl Pts',(-0.349931402212712,-0.746640918049129,
-3.90861755937831));
#53090=CARTESIAN_POINT('Ctrl Pts',(0.0493657477302857,-0.823096391506383,
-3.89276004880236));
#53091=CARTESIAN_POINT('Ctrl Pts',(0.436662522079763,-0.699464429810938,
-3.87690253822642));
#53092=CARTESIAN_POINT('Ctrl Pts',(0.71781050878804,-0.405798866722488,
-3.86104502765048));
#53093=CARTESIAN_POINT('Ctrl Pts',(0.824465124961427,-0.0134871969711484,
-3.84518751707454));
#53094=CARTESIAN_POINT('Ctrl Pts',(0.730699579014463,0.382103090785572,
-3.82933000649859));
#53095=CARTESIAN_POINT('Ctrl Pts',(0.459307443835841,0.684807504921484,
-3.81347249592265));
#53096=CARTESIAN_POINT('Ctrl Pts',(0.0762617413083615,0.821041286155828,
-3.7976149853467));
#53097=CARTESIAN_POINT('Ctrl Pts',(-0.325322514389958,0.757687210127501,
-3.78175747477077));
#53098=CARTESIAN_POINT('Ctrl Pts',(-0.647823751169212,0.510146091017909,
-3.76589996419481));
#53099=CARTESIAN_POINT('Ctrl Pts',(-0.812844777683873,0.138592980168027,
-3.75004245361888));
#53100=CARTESIAN_POINT('Ctrl Pts',(-0.780270445474654,-0.266650855386938,
-3.73418494304293));
#53101=CARTESIAN_POINT('Ctrl Pts',(-0.558019285895612,-0.607074232139984,
-3.71832743246699));
#53102=CARTESIAN_POINT('Ctrl Pts',(-0.200118585348163,-0.799923245416739,
-3.70246992189104));
#53103=CARTESIAN_POINT('Ctrl Pts',(0.206429169033917,-0.798318009900671,
-3.6866124113151));
#53104=CARTESIAN_POINT('Ctrl Pts',(0.56279582263738,-0.602648744113612,
-3.67075490073916));
#53105=CARTESIAN_POINT('Ctrl Pts',(0.782351801539573,-0.26048091175283,
-3.65489739016321));
#53106=CARTESIAN_POINT('Ctrl Pts',(0.811724993865988,0.145007520815514,
-3.63903987958727));
#53107=CARTESIAN_POINT('Ctrl Pts',(0.64377503698658,0.515245910719075,-3.62318236901133));
#53108=CARTESIAN_POINT('Ctrl Pts',(0.319329076364232,0.760232587928305,
-3.60732485843538));
#53109=CARTESIAN_POINT('Ctrl Pts',(-0.0827429515313146,0.820413463280368,
-3.59146734785944));
#53110=CARTESIAN_POINT('Ctrl Pts',(-0.464700901513617,0.681159099544468,
-3.57560983728349));
#53111=CARTESIAN_POINT('Ctrl Pts',(-0.733694182404323,0.376320997907176,
-3.55975232670756));
#53112=CARTESIAN_POINT('Ctrl Pts',(-0.824332912529633,-0.0199974018365713,
-3.54389481613161));
#53113=CARTESIAN_POINT('Ctrl Pts',(-0.714583620204558,-0.411454610492029,
-3.52803730555567));
#53114=CARTESIAN_POINT('Ctrl Pts',(-0.431125385349447,-0.702890851318391,
-3.51217979497972));
#53115=CARTESIAN_POINT('Ctrl Pts',(-0.0428643916996818,-0.823460558062143,
-3.49632228440378));
#53116=CARTESIAN_POINT('Ctrl Pts',(0.35581655553398,-0.743854303992209,
-3.48046477382783));
#53117=CARTESIAN_POINT('Ctrl Pts',(0.66800165280848,-0.483423663679116,
-3.4646072632519));
#53118=CARTESIAN_POINT('Ctrl Pts',(0.817801470828383,-0.105477016789133,
-3.44874975267595));
#53119=CARTESIAN_POINT('Ctrl Pts',(0.768801001967315,0.29811015771666,-3.43289224210001));
#53120=CARTESIAN_POINT('Ctrl Pts',(0.532911825764281,0.629229395944262,
-3.41703473152406));
#53121=CARTESIAN_POINT('Ctrl Pts',(0.167476509546501,0.807388546803781,
-3.40117722094812));
#53122=CARTESIAN_POINT('Ctrl Pts',(-0.238670861285152,0.789278700291097,
-3.38531971037218));
#53123=CARTESIAN_POINT('Ctrl Pts',(-0.586799461808706,0.579302199530446,
-3.36946219979623));
#53124=CARTESIAN_POINT('Ctrl Pts',(-0.792282315766162,0.228502470192357,
-3.35360468922029));
#53125=CARTESIAN_POINT('Ctrl Pts',(-0.805168363183897,-0.177844183732743,
-3.33774717864434));
#53126=CARTESIAN_POINT('Ctrl Pts',(-0.622325120183137,-0.540958493369726,
-3.3218896680684));
#53127=CARTESIAN_POINT('Ctrl Pts',(-0.288200158038096,-0.772570589439319,
-3.30603215749246));
#53128=CARTESIAN_POINT('Ctrl Pts',(0.115983707325935,-0.816377624873889,
-3.29017464691651));
#53129=CARTESIAN_POINT('Ctrl Pts',(0.491972961757609,-0.661730497755124,
-3.27431713634057));
#53130=CARTESIAN_POINT('Ctrl Pts',(0.748367951048111,-0.346222553574797,
-3.25845962576463));
#53131=CARTESIAN_POINT('Ctrl Pts',(0.822841326514434,0.0534490237494227,
-3.24260211518868));
#53132=CARTESIAN_POINT('Ctrl Pts',(0.697289270866175,0.440127617282441,
-3.22674460461274));
#53133=CARTESIAN_POINT('Ctrl Pts',(0.402232375679288,0.71981508925223,-3.2108870940368));
#53134=CARTESIAN_POINT('Ctrl Pts',(0.00939635618139049,0.824521894949015,
-3.19502958346085));
#53135=CARTESIAN_POINT('Ctrl Pts',(-0.385723834195541,0.72879473824479,
-3.17917207288491));
#53136=CARTESIAN_POINT('Ctrl Pts',(-0.687077980330429,0.455904042211581,
-3.16331456230897));
#53137=CARTESIAN_POINT('Ctrl Pts',(-0.821409561122009,0.0721871155896124,
-3.14745705173302));
#53138=CARTESIAN_POINT('Ctrl Pts',(-0.75606376027179,-0.329077858816847,
-3.13159954115708));
#53139=CARTESIAN_POINT('Ctrl Pts',(-0.506925562606628,-0.650346923369176,
-3.11574203058114));
#53140=CARTESIAN_POINT('Ctrl Pts',(-0.134558255104558,-0.813522416865705,
-3.09988452000519));
#53141=CARTESIAN_POINT('Ctrl Pts',(0.270518971211785,-0.778937823561237,
-3.08402700942925));
#53142=CARTESIAN_POINT('Ctrl Pts',(0.609835434064138,-0.555000351458992,
-3.06816949885331));
#53143=CARTESIAN_POINT('Ctrl Pts',(0.800906309733423,-0.196147214583821,
-3.05231198827736));
#53144=CARTESIAN_POINT('Ctrl Pts',(0.797283962390398,0.210387571103583,
-3.03645447770142));
#53145=CARTESIAN_POINT('Ctrl Pts',(0.599848952558207,0.565779003564664,
-3.02059696712548));
#53146=CARTESIAN_POINT('Ctrl Pts',(0.256595980656287,0.783634576490111,
-3.00473945654953));
#53147=CARTESIAN_POINT('Ctrl Pts',(-0.149033199147652,0.810995531622473,
-2.98888194597359));
#53148=CARTESIAN_POINT('Ctrl Pts',(-0.51843372957618,0.641210663352952,
-2.97302443539765));
#53149=CARTESIAN_POINT('Ctrl Pts',(-0.761807616809609,0.315553167834938,
-2.9571669248217));
#53150=CARTESIAN_POINT('Ctrl Pts',(-0.819992826629131,-0.0868125050702396,
-2.94130941424576));
#53151=CARTESIAN_POINT('Ctrl Pts',(-0.678845050401212,-0.468074827677772,
-2.92545190366981));
#53152=CARTESIAN_POINT('Ctrl Pts',(-0.372676061102124,-0.735552309656633,
-2.90959439309387));
#53153=CARTESIAN_POINT('Ctrl Pts',(0.0240871744823412,-0.824223546609326,
-2.89373688251793));
#53154=CARTESIAN_POINT('Ctrl Pts',(0.414995031508496,-0.71253334699722,
-2.87787937194199));
#53155=CARTESIAN_POINT('Ctrl Pts',(0.705021275746043,-0.427632608093937,
-2.86202186136604));
#53156=CARTESIAN_POINT('Ctrl Pts',(0.823663098611094,-0.0387781735796382,
-2.8461643507901));
#53157=CARTESIAN_POINT('Ctrl Pts',(0.742079724850744,0.359502891122233,
-2.83030684021416));
#53158=CARTESIAN_POINT('Ctrl Pts',(0.480103349303,0.670391990366713,-2.81444932963821));
#53159=CARTESIAN_POINT('Ctrl Pts',(0.101418106165091,0.818314740489066,
-2.79859181906227));
#53160=CARTESIAN_POINT('Ctrl Pts',(-0.301920979402475,0.767312432426616,
-2.78273430848632));
#53161=CARTESIAN_POINT('Ctrl Pts',(-0.631865751727002,0.529783275079793,
-2.76687679791039));
#53162=CARTESIAN_POINT('Ctrl Pts',(-0.80820956196675,0.163468500651699,
-2.75101928733443));
#53163=CARTESIAN_POINT('Ctrl Pts',(-0.788084793327346,-0.242584016963188,
-2.7351617767585));
#53164=CARTESIAN_POINT('Ctrl Pts',(-0.57638359863761,-0.589666510818917,
-2.71930426618255));
#53165=CARTESIAN_POINT('Ctrl Pts',(-0.224568661370999,-0.793406303913598,
-2.70344675560661));
#53166=CARTESIAN_POINT('Ctrl Pts',(0.181836926435539,-0.804276058915269,
-2.68758924503066));
#53167=CARTESIAN_POINT('Ctrl Pts',(0.544039569602812,-0.619633434754925,
-2.67173173445472));
#53168=CARTESIAN_POINT('Ctrl Pts',(0.773991016887443,-0.284363416313251,
-2.65587422387878));
#53169=CARTESIAN_POINT('Ctrl Pts',(0.815792110218004,0.12003282745089,-2.64001671330283));
#53170=CARTESIAN_POINT('Ctrl Pts',(0.659281374416868,0.495250155080043,
-2.62415920272689));
#53171=CARTESIAN_POINT('Ctrl Pts',(0.342505181723618,0.75007656092713,-2.60830169215095));
#53172=CARTESIAN_POINT('Ctrl Pts',(-0.0575309839749372,0.822566005037088,
-2.592444181575));
#53173=CARTESIAN_POINT('Ctrl Pts',(-0.443581877542379,0.695096946242594,
-2.57658667099907));
#53174=CARTESIAN_POINT('Ctrl Pts',(-0.721801949503084,0.398655982588181,
-2.56072916042311));
#53175=CARTESIAN_POINT('Ctrl Pts',(-0.824558367079424,0.00530528407468725,
-2.54487164984718));
#53176=CARTESIAN_POINT('Ctrl Pts',(-0.72687195620322,-0.389335081960394,
-2.52901413927123));
#53177=CARTESIAN_POINT('Ctrl Pts',(-0.452489417264832,-0.689331541439337,
-2.51315662869529));
#53178=CARTESIAN_POINT('Ctrl Pts',(-0.0681107127879656,-0.821757614849608,
-2.49729911811934));
#53179=CARTESIAN_POINT('Ctrl Pts',(0.332825102093949,-0.75442169784276,
-2.4814416075434));
#53180=CARTESIAN_POINT('Ctrl Pts',(0.652854085504351,-0.503692554838839,
-2.46558409696745));
#53181=CARTESIAN_POINT('Ctrl Pts',(0.814180028972541,-0.130520217522318,
-2.44972658639152));
#53182=CARTESIAN_POINT('Ctrl Pts',(0.777586025966992,0.274380427473716,
-2.43386907581557));
#53183=CARTESIAN_POINT('Ctrl Pts',(0.551967754173711,0.61258162322439,-2.41801156523963));
#53184=CARTESIAN_POINT('Ctrl Pts',(0.192171015120368,0.801869657555022,
-2.40215405466368));
#53185=CARTESIAN_POINT('Ctrl Pts',(-0.214340793908872,0.796230287559016,
-2.38629654408774));
#53186=CARTESIAN_POINT('Ctrl Pts',(-0.568748256297336,0.597034394083407,
-2.3704390335118));
#53187=CARTESIAN_POINT('Ctrl Pts',(-0.784898060136431,0.252704732749246,
-2.35458152293585));
#53188=CARTESIAN_POINT('Ctrl Pts',(-0.810246104510137,-0.153055208620778,
-2.33872401235991));
#53189=CARTESIAN_POINT('Ctrl Pts',(-0.638630504568503,-0.521608785771845,
-2.32286650178397));
#53190=CARTESIAN_POINT('Ctrl Pts',(-0.311769491103034,-0.763363891716889,
-2.30700899120802));
#53191=CARTESIAN_POINT('Ctrl Pts',(0.0908799214823766,-0.819552003616096,
-2.29115148063208));
#53192=CARTESIAN_POINT('Ctrl Pts',(0.471437230902318,-0.67651428963397,
-2.27529397005613));
#53193=CARTESIAN_POINT('Ctrl Pts',(0.737392329280969,-0.369021949858524,
-2.2594364594802));
#53194=CARTESIAN_POINT('Ctrl Pts',(0.824093890176505,0.0281763541565548,
-2.24357894890425));
#53195=CARTESIAN_POINT('Ctrl Pts',(0.710465532836513,0.418525236289438,
-2.22772143832831));
#53196=CARTESIAN_POINT('Ctrl Pts',(0.424129303494443,0.707134344150474,
-2.21186392775236));
#53197=CARTESIAN_POINT('Ctrl Pts',(0.0346910008289892,0.823845362444482,
-2.19600641717642));
#53198=CARTESIAN_POINT('Ctrl Pts',(-0.363180376565469,0.740286877391164,
-2.18014890660048));
#53199=CARTESIAN_POINT('Ctrl Pts',(-0.672765824396101,0.476771215872387,
-2.16429139602453));
#53200=CARTESIAN_POINT('Ctrl Pts',(-0.818807865098622,0.0973566988575322,
-2.14843388544859));
#53201=CARTESIAN_POINT('Ctrl Pts',(-0.765804973395835,-0.305724368479202,
-2.13257637487265));
#53202=CARTESIAN_POINT('Ctrl Pts',(-0.52664168233383,-0.634486552409421,
-2.1167188642967));
#53203=CARTESIAN_POINT('Ctrl Pts',(-0.15945646753355,-0.809010680845144,
-2.10086135372076));
#53204=CARTESIAN_POINT('Ctrl Pts',(0.246491200773431,-0.786871485505144,
-2.08500384314482));
#53205=CARTESIAN_POINT('Ctrl Pts',(0.592519043578318,-0.57345080848913,
-2.06914633256887));
#53206=CARTESIAN_POINT('Ctrl Pts',(0.794510760199069,-0.220629324179034,
-2.05328882199293));
#53207=CARTESIAN_POINT('Ctrl Pts',(0.803363955195986,0.185825192726024,
-2.03743131141698));
#53208=CARTESIAN_POINT('Ctrl Pts',(0.616926495358278,0.547107252816805,
-2.02157380084104));
#53209=CARTESIAN_POINT('Ctrl Pts',(0.280519674206675,0.775392390433891,
-2.0057162902651));
#53210=CARTESIAN_POINT('Ctrl Pts',(-0.124078992640135,0.815186512612425,
-1.98985877968915));
#53211=CARTESIAN_POINT('Ctrl Pts',(-0.498515156467999,0.656816021067916,
-1.97400126911321));
#53212=CARTESIAN_POINT('Ctrl Pts',(-0.751766705624085,0.338779378172446,
-1.95814375853727));
#53213=CARTESIAN_POINT('Ctrl Pts',(-0.822270433852137,-0.0616115279182409,
-1.94228624796132));
#53214=CARTESIAN_POINT('Ctrl Pts',(-0.692887509910239,-0.447025217823546,
-1.92642873738538));
#53215=CARTESIAN_POINT('Ctrl Pts',(-0.39506977549183,-0.723771040628618,
-1.91057122680944));
#53216=CARTESIAN_POINT('Ctrl Pts',(-0.00121408136393792,-0.824574540454796,
-1.89471371623349));
#53217=CARTESIAN_POINT('Ctrl Pts',(0.392936745179409,-0.72493128022428,
-1.87885620565755));
#53218=CARTESIAN_POINT('Ctrl Pts',(0.691568132770651,-0.449063653055908,
-1.86299869508161));
#53219=CARTESIAN_POINT('Ctrl Pts',(0.822085438770328,-0.0640326332552135,
-1.84714118450567));
#53220=CARTESIAN_POINT('Ctrl Pts',(0.752761063264271,0.336564151972617,
-1.83128367392972));
#53221=CARTESIAN_POINT('Ctrl Pts',(0.500447147303881,0.655345175854074,
-1.81542616335378));
#53222=CARTESIAN_POINT('Ctrl Pts',(0.126478966828661,0.814817597815459,
-1.79956865277783));
#53223=CARTESIAN_POINT('Ctrl Pts',(-0.278235129112421,0.776215085970115,
-1.78371114220189));
#53224=CARTESIAN_POINT('Ctrl Pts',(-0.615312732015794,0.54892156869544,
-1.76785363162595));
#53225=CARTESIAN_POINT('Ctrl Pts',(-0.802813265166102,0.1881900848428,-1.75199612105));
#53226=CARTESIAN_POINT('Ctrl Pts',(-0.795157011345605,-0.218288740130424,
-1.73613861047406));
#53227=CARTESIAN_POINT('Ctrl Pts',(-0.594205137977248,-0.571703507739143,
-1.72028109989812));
#53228=CARTESIAN_POINT('Ctrl Pts',(-0.248807263825392,-0.786142221374429,
-1.70442358932217));
#53229=CARTESIAN_POINT('Ctrl Pts',(0.157073450222133,-0.809476730978177,
-1.68856607874623));
#53230=CARTESIAN_POINT('Ctrl Pts',(0.52477100114339,-0.636034624150891,
-1.67270856817029));
#53231=CARTESIAN_POINT('Ctrl Pts',(0.76490137433819,-0.307978139314054,
-1.65685105759434));
#53232=CARTESIAN_POINT('Ctrl Pts',(0.819091005093328,0.0949451006371796,
-1.6409935470184));
#53233=CARTESIAN_POINT('Ctrl Pts',(0.674166874620773,0.474788028412531,
-1.62513603644245));
#53234=CARTESIAN_POINT('Ctrl Pts',(0.365358754132285,0.739214195980236,
-1.60927852586651));
#53235=CARTESIAN_POINT('Ctrl Pts',(-0.0322648401929043,0.823943946423011,
-1.59342101529057));
#53236=CARTESIAN_POINT('Ctrl Pts',(-0.422045137929226,0.708380228627325,
-1.57756350471462));
#53237=CARTESIAN_POINT('Ctrl Pts',(-0.709230004512728,0.420615557794379,
-1.56170599413868));
#53238=CARTESIAN_POINT('Ctrl Pts',(-0.824007345075392,0.030602974064658,
-1.54584848356274));
#53239=CARTESIAN_POINT('Ctrl Pts',(-0.738475805749304,-0.366848921332357,
-1.52999097298679));
#53240=CARTESIAN_POINT('Ctrl Pts',(-0.473427345416823,-0.675123096458254,
-1.51413346241085));
#53241=CARTESIAN_POINT('Ctrl Pts',(-0.0932928948490484,-0.819280832517449,
-1.49827595183491));
#53242=CARTESIAN_POINT('Ctrl Pts',(0.309520231316071,-0.764278661985173,
-1.48241844125897));
#53243=CARTESIAN_POINT('Ctrl Pts',(0.637091733473383,-0.523487124865244,
-1.46656093068302));
#53244=CARTESIAN_POINT('Ctrl Pts',(0.809791883717243,-0.155440508959154,
-1.45070342010708));
#53245=CARTESIAN_POINT('Ctrl Pts',(0.785638806693365,0.250392316529934,
-1.43484590953113));
#53246=CARTESIAN_POINT('Ctrl Pts',(0.57050390128361,0.595356989864048,-1.41898839895519));
#53247=CARTESIAN_POINT('Ctrl Pts',(0.216684555593979,0.795595657433373,
-1.40313088837925));
#53248=CARTESIAN_POINT('Ctrl Pts',(-0.189808884422145,0.802432074479965,
-1.3872733778033));
#53249=CARTESIAN_POINT('Ctrl Pts',(-0.55016146749232,0.61420436863189,-1.37141586722736));
#53250=CARTESIAN_POINT('Ctrl Pts',(-0.776774675580029,0.276669026342562,
-1.35555835665142));
#53251=CARTESIAN_POINT('Ctrl Pts',(-0.81456084696559,-0.128122103286285,
-1.33970084607547));
#53252=CARTESIAN_POINT('Ctrl Pts',(-0.654334498399659,-0.501767885544569,
-1.32384333549953));
#53253=CARTESIAN_POINT('Ctrl Pts',(-0.335045234642093,-0.753438343531457,
-1.30798582492359));
#53254=CARTESIAN_POINT('Ctrl Pts',(0.0656905551256053,-0.821954620235868,
-1.29212831434764));
#53255=CARTESIAN_POINT('Ctrl Pts',(0.450457553358707,-0.690661016260428,
-1.2762708037717));
#53256=CARTESIAN_POINT('Ctrl Pts',(0.72572231415428,-0.391473842674518,
-1.26041329319576));
#53257=CARTESIAN_POINT('Ctrl Pts',(0.824570414676984,0.00287715123474536,
-1.24455578261981));
#53258=CARTESIAN_POINT('Ctrl Pts',(0.722972758082991,0.396528735187848,
-1.22869827204387));
#53259=CARTESIAN_POINT('Ctrl Pts',(0.445626833919317,0.693787699264584,
-1.21284076146793));
#53260=CARTESIAN_POINT('Ctrl Pts',(0.0599529773843778,0.822393024813896,
-1.19698325089198));
#53261=CARTESIAN_POINT('Ctrl Pts',(-0.340294916405972,0.751081897417354,
-1.18112574031604));
#53262=CARTESIAN_POINT('Ctrl Pts',(-0.657820133093386,0.497189419896282,
-1.1652682297401));
#53263=CARTESIAN_POINT('Ctrl Pts',(-0.815435107698969,0.122434602509957,
-1.14941071916415));
#53264=CARTESIAN_POINT('Ctrl Pts',(-0.774825037320025,-0.282082981233933,
-1.13355320858821));
#53265=CARTESIAN_POINT('Ctrl Pts',(-0.545861870014327,-0.618028693204662,
-1.11769569801227));
#53266=CARTESIAN_POINT('Ctrl Pts',(-0.184204521752573,-0.803737109337193,
-1.10183818743632));
#53267=CARTESIAN_POINT('Ctrl Pts',(0.222231312578776,-0.794064160171781,
-1.08598067686038));
#53268=CARTESIAN_POINT('Ctrl Pts',(0.574644685138513,-0.591361253889582,
-1.07012316628444));
#53269=CARTESIAN_POINT('Ctrl Pts',(0.787367029575686,-0.24490366983155,
-1.05426565570849));
#53270=CARTESIAN_POINT('Ctrl Pts',(0.80868742996682,0.161087825031754,-1.03840814513255));
#53271=CARTESIAN_POINT('Ctrl Pts',(0.63342308600479,0.527920297844257,-1.02255063455661));
#53272=CARTESIAN_POINT('Ctrl Pts',(0.30417920580247,0.766420026824182,-1.00669312398066));
#53273=CARTESIAN_POINT('Ctrl Pts',(-0.0990079424591542,0.818609842409561,
-0.990835613404719));
#53274=CARTESIAN_POINT('Ctrl Pts',(-0.478127137719371,0.671802863149659,
-0.974978102828773));
#53275=CARTESIAN_POINT('Ctrl Pts',(-0.741017864904195,0.361686564102989,
-0.959120592252833));
#53276=CARTESIAN_POINT('Ctrl Pts',(-0.823773719040125,-0.0363525319421145,
-0.943263081676887));
#53277=CARTESIAN_POINT('Ctrl Pts',(-0.706277485705126,-0.42555464977585,
-0.927405571100945));
#53278=CARTESIAN_POINT('Ctrl Pts',(-0.41709145749421,-0.711308205242394,
-0.911548060525001));
#53279=CARTESIAN_POINT('Ctrl Pts',(-0.0265141939245934,-0.824149042516177,
-0.895690549949058));
#53280=CARTESIAN_POINT('Ctrl Pts',(0.37050843511164,-0.736646554509639,
-0.879833039373114));
#53281=CARTESIAN_POINT('Ctrl Pts',(0.677463748522479,-0.470071820254814,
-0.863975528797172));
#53282=CARTESIAN_POINT('Ctrl Pts',(0.819733631102158,-0.0892267941812924,
-0.848118018221227));
#53283=CARTESIAN_POINT('Ctrl Pts',(0.762733535768966,0.313308474467536,
-0.832260507645284));
#53284=CARTESIAN_POINT('Ctrl Pts',(0.520319680332095,0.63968123078523,-0.81640299706934));
#53285=CARTESIAN_POINT('Ctrl Pts',(0.151420723792317,0.810553151351601,
-0.800545486493398));
#53286=CARTESIAN_POINT('Ctrl Pts',(-0.254287268196057,0.784386787237767,
-0.784687975917453));
#53287=CARTESIAN_POINT('Ctrl Pts',(-0.598180279812305,0.567542949567232,
-0.768830465341511));
#53288=CARTESIAN_POINT('Ctrl Pts',(-0.796660968908797,0.212734452727095,
-0.752972954765567));
#53289=CARTESIAN_POINT('Ctrl Pts',(-0.801480439708001,-0.193787903454448,
-0.737115444189623));
#53290=CARTESIAN_POINT('Ctrl Pts',(-0.611467121588348,-0.553202138441512,
-0.72125793361368));
#53291=CARTESIAN_POINT('Ctrl Pts',(-0.272811567515137,-0.77813783829713,
-0.705400423037737));
#53292=CARTESIAN_POINT('Ctrl Pts',(0.132162059857106,-0.813915128679966,
-0.689542912461794));
#53293=CARTESIAN_POINT('Ctrl Pts',(0.505008262234922,-0.651836867501574,
-0.67368540188585));
#53294=CARTESIAN_POINT('Ctrl Pts',(0.755091433497301,-0.331302843058724,
-0.657827891309907));
#53295=CARTESIAN_POINT('Ctrl Pts',(0.821618571962899,0.0697679651806149,
-0.641970380733963));
#53296=CARTESIAN_POINT('Ctrl Pts',(0.688417520104387,0.453878799651551,
-0.62611287015802));
#53297=CARTESIAN_POINT('Ctrl Pts',(0.387868272659935,0.727655722044151,
-0.610255359582077));
#53298=CARTESIAN_POINT('Ctrl Pts',(-0.00696831300448354,0.824545989847542,
-0.594397849006133));
#53299=CARTESIAN_POINT('Ctrl Pts',(-0.400110963559091,0.720996437993744,
-0.578540338430189));
#53300=CARTESIAN_POINT('Ctrl Pts',(-0.695990186280356,0.442179044461741,
-0.562682827854247));
#53301=CARTESIAN_POINT('Ctrl Pts',(-0.822680365408402,0.0558718456073918,
-0.546825317278302));
#53302=CARTESIAN_POINT('Ctrl Pts',(-0.749384241638951,-0.344017303551129,
-0.530967806702359));
#53303=CARTESIAN_POINT('Ctrl Pts',(-0.493919452814545,-0.660278896294274,
-0.515110296126415));
#53304=CARTESIAN_POINT('Ctrl Pts',(-0.118387224128064,-0.816032543421702,
-0.499252785550473));
#53305=CARTESIAN_POINT('Ctrl Pts',(0.285923889110438,-0.773415914235931,
-0.483395274974528));
#53306=CARTESIAN_POINT('Ctrl Pts',(0.620729439934895,-0.542788733454466,
-0.467537764398586));
#53307=CARTESIAN_POINT('Ctrl Pts',(0.804641167316146,-0.180214423962784,
-0.451680253822641));
#53308=CARTESIAN_POINT('Ctrl Pts',(0.79295176095903,0.226168414191993,-0.435822743246698));
#53309=CARTESIAN_POINT('Ctrl Pts',(0.588502811795286,0.577571716099595,
-0.419965232670754));
#53310=CARTESIAN_POINT('Ctrl Pts',(0.240994046933947,0.788572454570089,
-0.404107722094812));
#53311=CARTESIAN_POINT('Ctrl Pts',(-0.165098234358834,0.80787822094225,
-0.388250211518868));
#53312=CARTESIAN_POINT('Ctrl Pts',(-0.531056598084034,0.630795954351229,
-0.372392700942924));
#53313=CARTESIAN_POINT('Ctrl Pts',(-0.767919812300705,0.300372784224499,
-0.356535190366982));
#53314=CARTESIAN_POINT('Ctrl Pts',(-0.818108526410274,-0.10306834719425,
-0.340677679791037));
#53315=CARTESIAN_POINT('Ctrl Pts',(-0.669422315370429,-0.481454476105894,
-0.324820169215095));
#53316=CARTESIAN_POINT('Ctrl Pts',(-0.358005466355305,-0.742803292658146,
-0.308962658639151));
#53317=CARTESIAN_POINT('Ctrl Pts',(0.0404393213179984,-0.823583210249897,
-0.293105148063208));
#53318=CARTESIAN_POINT('Ctrl Pts',(0.42905370000224,-0.704157359680949,
-0.277247637487263));
#53319=CARTESIAN_POINT('Ctrl Pts',(0.713368866712798,-0.413557081834078,
-0.261390126911321));
#53320=CARTESIAN_POINT('Ctrl Pts',(0.824270506897614,-0.022424775748895,
-0.245532616335377));
#53321=CARTESIAN_POINT('Ctrl Pts',(0.734799060031862,0.374158856504314,
-0.229675105759433));
#53322=CARTESIAN_POINT('Ctrl Pts',(0.466704935323213,0.679787666910914,
-0.213817595183491));
#53323=CARTESIAN_POINT('Ctrl Pts',(0.0851580820844976,0.820166359232661,
-0.197960084607547));
#53324=CARTESIAN_POINT('Ctrl Pts',(-0.317088194075989,0.761169418782602,
-0.182102574031603));
#53325=CARTESIAN_POINT('Ctrl Pts',(-0.642256564426576,0.517139844854084,
-0.16624506345566));
#53326=CARTESIAN_POINT('Ctrl Pts',(-0.811291370158351,0.147396393859673,
-0.150387552879717));
#53327=CARTESIAN_POINT('Ctrl Pts',(-0.783121507604153,-0.258174361913263,
-0.134530042303774));
#53328=CARTESIAN_POINT('Ctrl Pts',(-0.564556177128614,-0.600991981115412,
-0.11867253172783));
#53329=CARTESIAN_POINT('Ctrl Pts',(-0.208802571875496,-0.797700379488531,
-0.102815021151887));
#53330=CARTESIAN_POINT('Ctrl Pts',(0.197811256787455,-0.800523053928257,
-0.0869575105759431));
#53331=CARTESIAN_POINT('Ctrl Pts',(0.436668678781749,-0.672619994853352,
-0.0763858368586473));
#53332=CARTESIAN_POINT('Ctrl Pts',(0.533647856309019,-0.584002718706676,
-0.0710999999999995));
#53333=CARTESIAN_POINT('Ctrl Pts',(0.437168237015814,-0.613060138694073,
-5.8529325805302));
#53334=CARTESIAN_POINT('Ctrl Pts',(0.538972674085852,-0.540464216262873,
-5.84764674367155));
#53335=CARTESIAN_POINT('Ctrl Pts',(0.705617707738108,-0.34365284496799,
-5.83707506995425));
#53336=CARTESIAN_POINT('Ctrl Pts',(0.78403213362876,0.035343353160595,-5.82121755937831));
#53337=CARTESIAN_POINT('Ctrl Pts',(0.671861149737833,0.405647193175061,
-5.80536004880237));
#53338=CARTESIAN_POINT('Ctrl Pts',(0.39636423752786,0.677391306117648,-5.78950253822642));
#53339=CARTESIAN_POINT('Ctrl Pts',(0.0245158897253287,0.784442450324301,
-5.77364502765049));
#53340=CARTESIAN_POINT('Ctrl Pts',(-0.353292660905754,0.700815442703755,
-5.75778751707453));
#53341=CARTESIAN_POINT('Ctrl Pts',(-0.645218587577802,0.446819837923923,
-5.74193000649859));
#53342=CARTESIAN_POINT('Ctrl Pts',(-0.780297754981346,0.0842096578098633,
-5.72607249592265));
#53343=CARTESIAN_POINT('Ctrl Pts',(-0.725693375032965,-0.298872866094613,
-5.71021498534671));
#53344=CARTESIAN_POINT('Ctrl Pts',(-0.494679411256276,-0.609301164450066,
-5.69435747477076));
#53345=CARTESIAN_POINT('Ctrl Pts',(-0.143413247169386,-0.771614203049557,
-5.67849996419482));
#53346=CARTESIAN_POINT('Ctrl Pts',(0.242715394896773,-0.746354439128878,
-5.66264245361887));
#53347=CARTESIAN_POINT('Ctrl Pts',(0.569842081970103,-0.539662646474474,
-5.64678494304293));
#53348=CARTESIAN_POINT('Ctrl Pts',(0.758445208316514,-0.201783588651147,
-5.63092743246699));
#53349=CARTESIAN_POINT('Ctrl Pts',(0.762677030403281,0.185147239587262,
-5.61506992189104));
#53350=CARTESIAN_POINT('Ctrl Pts',(0.581508827592089,0.527070431254392,
-5.5992124113151));
#53351=CARTESIAN_POINT('Ctrl Pts',(0.258980984868453,0.740867466012043,
-5.58335490073916));
#53352=CARTESIAN_POINT('Ctrl Pts',(-0.126502839331452,0.774566192508729,
-5.56749739016321));
#53353=CARTESIAN_POINT('Ctrl Pts',(-0.481234944771481,0.619974742833006,
-5.55163987958727));
#53354=CARTESIAN_POINT('Ctrl Pts',(-0.718983101847058,0.314672930995483,
-5.53578236901132));
#53355=CARTESIAN_POINT('Ctrl Pts',(-0.781952841385118,-0.0671230810142253,
-5.51992485843539));
#53356=CARTESIAN_POINT('Ctrl Pts',(-0.654836778037186,-0.432602066861879,
-5.50406734785944));
#53357=CARTESIAN_POINT('Ctrl Pts',(-0.368535699764102,-0.692919325877319,
-5.4882098372835));
#53358=CARTESIAN_POINT('Ctrl Pts',(0.00735313965826202,-0.784794040162126,
-5.47235232670755));
#53359=CARTESIAN_POINT('Ctrl Pts',(0.381454496024887,-0.685892281353231,
-5.45649481613161));
#53360=CARTESIAN_POINT('Ctrl Pts',(0.662827646405622,-0.420256190090367,
-5.44063730555566));
#53361=CARTESIAN_POINT('Ctrl Pts',(0.783073272615713,-0.052459545043391,
-5.42477979497973));
#53362=CARTESIAN_POINT('Ctrl Pts',(0.712960729027783,0.328089550299248,
-5.40892228440377));
#53363=CARTESIAN_POINT('Ctrl Pts',(0.469533753366363,0.628882984823358,
-5.39306477382785));
#53364=CARTESIAN_POINT('Ctrl Pts',(0.111967285176232,0.776800541452915,
-5.37720726325188));
#53365=CARTESIAN_POINT('Ctrl Pts',(-0.272817437331468,0.735884773615265,
-5.36134975267595));
#53366=CARTESIAN_POINT('Ctrl Pts',(-0.591282659639843,0.516081941711108,
-5.34549224210001));
#53367=CARTESIAN_POINT('Ctrl Pts',(-0.766012309737663,0.170824165390574,
-5.32963473152406));
#53368=CARTESIAN_POINT('Ctrl Pts',(-0.754531158849833,-0.21595945099891,
-5.31377722094812));
#53369=CARTESIAN_POINT('Ctrl Pts',(-0.559630172964593,-0.550245239560189,
-5.29791971037218));
#53370=CARTESIAN_POINT('Ctrl Pts',(-0.2286880537467,-0.750771288892008,
-5.28206219979623));
#53371=CARTESIAN_POINT('Ctrl Pts',(0.157846103774871,-0.768791494277949,
-5.2662046892203));
#53372=CARTESIAN_POINT('Ctrl Pts',(0.506009272941894,-0.5999253035569,-5.25034717864434));
#53373=CARTESIAN_POINT('Ctrl Pts',(0.73116607416563,-0.28522259051528,-5.2344896680684));
#53374=CARTESIAN_POINT('Ctrl Pts',(0.778582885322433,0.0988152054798314,
-5.21863215749246));
#53375=CARTESIAN_POINT('Ctrl Pts',(0.636733100020407,0.458831901124396,
-5.20277464691652));
#53376=CARTESIAN_POINT('Ctrl Pts',(0.340099143417682,0.707310629637068,
-5.18691713634057));
#53377=CARTESIAN_POINT('Ctrl Pts',(-0.039209899610264,0.783848415143884,
-5.17105962576463));
#53378=CARTESIAN_POINT('Ctrl Pts',(-0.408987363680301,0.669839600576782,
-5.15520211518868));
#53379=CARTESIAN_POINT('Ctrl Pts',(-0.679343625746411,0.392998717947966,
-5.13934460461275));
#53380=CARTESIAN_POINT('Ctrl Pts',(-0.784557475495335,0.0206233313364565,
-5.12348709403679));
#53381=CARTESIAN_POINT('Ctrl Pts',(-0.699052358885477,-0.35676540427524,
-5.10762958346086));
#53382=CARTESIAN_POINT('Ctrl Pts',(-0.443613811671148,-0.647427633211327,
-5.09177207288491));
#53383=CARTESIAN_POINT('Ctrl Pts',(-0.0803366799465044,-0.780705944646382,
-5.07591456230896));
#53384=CARTESIAN_POINT('Ctrl Pts',(0.30246958640326,-0.724201562724126,
-5.06005705173303));
#53385=CARTESIAN_POINT('Ctrl Pts',(0.611748178012079,-0.491650201718588,
-5.04419954115708));
#53386=CARTESIAN_POINT('Ctrl Pts',(0.772316211342588,-0.139583035675748,
-5.02834203058114));
#53387=CARTESIAN_POINT('Ctrl Pts',(0.745141021098056,0.24641552878821,-5.0124845200052));
#53388=CARTESIAN_POINT('Ctrl Pts',(0.536828655090044,0.572512662938769,
-4.99662700942925));
#53389=CARTESIAN_POINT('Ctrl Pts',(0.19801800258504,0.759437044660883,-4.98076949885331));
#53390=CARTESIAN_POINT('Ctrl Pts',(-0.188929070708771,0.761749014040809,
-4.96491198827737));
#53391=CARTESIAN_POINT('Ctrl Pts',(-0.529949161969875,0.578886551820349,
-4.94905447770142));
#53392=CARTESIAN_POINT('Ctrl Pts',(-0.742143310517495,0.255301901295619,
-4.93319696712548));
#53393=CARTESIAN_POINT('Ctrl Pts',(-0.77392900016589,-0.130344377911946,
-4.91733945654953));
#53394=CARTESIAN_POINT('Ctrl Pts',(-0.617579411575381,-0.484305094490272,
-4.90148194597358));
#53395=CARTESIAN_POINT('Ctrl Pts',(-0.311101743527395,-0.720535536476336,
-4.88562443539765));
#53396=CARTESIAN_POINT('Ctrl Pts',(0.0710020001251872,-0.781610177856742,
-4.8697669248217));
#53397=CARTESIAN_POINT('Ctrl Pts',(0.43584578705537,-0.652682314803389,
-4.85390941424576));
#53398=CARTESIAN_POINT('Ctrl Pts',(0.69473932738756,-0.365093167742298,
-4.83805190366982));
#53399=CARTESIAN_POINT('Ctrl Pts',(0.784747896832823,0.0112468914587877,
-4.82219439309387));
#53400=CARTESIAN_POINT('Ctrl Pts',(0.68399121018045,0.384852931061866,-4.80633688251793));
#53401=CARTESIAN_POINT('Ctrl Pts',(0.416962324640737,0.664904635253221,
-4.79047937194199));
#53402=CARTESIAN_POINT('Ctrl Pts',(0.048573594794104,0.783323917699316,
-4.77462186136604));
#53403=CARTESIAN_POINT('Ctrl Pts',(-0.331622945290539,0.71132410075004,
-4.75876435079011));
#53404=CARTESIAN_POINT('Ctrl Pts',(-0.631204887564187,0.466407701551024,
-4.74290684021414));
#53405=CARTESIAN_POINT('Ctrl Pts',(-0.777346517971772,0.108111725303905,
-4.72704932963822));
#53406=CARTESIAN_POINT('Ctrl Pts',(-0.734522101861767,-0.276465252839481,
-4.71119181906226));
#53407=CARTESIAN_POINT('Ctrl Pts',(-0.513141875106644,-0.593835979175278,
-4.69533430848633));
#53408=CARTESIAN_POINT('Ctrl Pts',(-0.167021408060069,-0.766850443959353,
-4.67947679791038));
#53409=CARTESIAN_POINT('Ctrl Pts',(0.219700482463985,-0.753450364759431,
-4.66361928733444));
#53410=CARTESIAN_POINT('Ctrl Pts',(0.553015133578838,-0.556893182023092,
-4.64776177675849));
#53411=CARTESIAN_POINT('Ctrl Pts',(0.751896708786371,-0.224960204185648,
-4.63190426618255));
#53412=CARTESIAN_POINT('Ctrl Pts',(0.767998860449733,0.161658604778522,
-4.61604675560661));
#53413=CARTESIAN_POINT('Ctrl Pts',(0.59740729826221,0.508979640196021,-4.60018924503066));
#53414=CARTESIAN_POINT('Ctrl Pts',(0.281591318516465,0.732572237726208,
-4.58433173445472));
#53415=CARTESIAN_POINT('Ctrl Pts',(-0.102677014154933,0.778083019295018,
-4.56847422387877));
#53416=CARTESIAN_POINT('Ctrl Pts',(-0.461985475025898,0.634448717404426,
-4.55261671330284));
#53417=CARTESIAN_POINT('Ctrl Pts',(-0.708989362909296,0.336585557373601,
-4.53675920272689));
#53418=CARTESIAN_POINT('Ctrl Pts',(-0.783644222612109,-0.0430985674667928,
-4.52090169215095));
#53419=CARTESIAN_POINT('Ctrl Pts',(-0.667802119635095,-0.412305812670522,
-4.50504418157501));
#53420=CARTESIAN_POINT('Ctrl Pts',(-0.389623242148861,-0.681285170342373,
-4.48918667099906));
#53421=CARTESIAN_POINT('Ctrl Pts',(-0.0167304089195194,-0.784650143419608,
-4.47332916042312));
#53422=CARTESIAN_POINT('Ctrl Pts',(0.360229438385337,-0.697273623387268,
-4.45747164984717));
#53423=CARTESIAN_POINT('Ctrl Pts',(0.649620703034755,-0.440396067579693,
-4.44161413927123));
#53424=CARTESIAN_POINT('Ctrl Pts',(0.78109493435295,-0.0764621323217238,
-4.42575662869529));
#53425=CARTESIAN_POINT('Ctrl Pts',(0.72269191236498,0.306059069385753,-4.40989911811935));
#53426=CARTESIAN_POINT('Ctrl Pts',(0.488608893911385,0.614180024863817,
-4.39404160754339));
#53427=CARTESIAN_POINT('Ctrl Pts',(0.135749385384003,0.772999261654816,
-4.37818409696746));
#53428=CARTESIAN_POINT('Ctrl Pts',(-0.250109595167953,0.74390923139584,
-4.36232658639151));
#53429=CARTESIAN_POINT('Ctrl Pts',(-0.57516915062141,0.53398146252887,-4.34646907581558));
#53430=CARTESIAN_POINT('Ctrl Pts',(-0.760410185043356,0.194247534433146,
-4.33061156523962));
#53431=CARTESIAN_POINT('Ctrl Pts',(-0.760802245324052,-0.192706247072863,
-4.31475405466368));
#53432=CARTESIAN_POINT('Ctrl Pts',(-0.576250025085295,-0.532814848460723,
-4.29889654408774));
#53433=CARTESIAN_POINT('Ctrl Pts',(-0.251616532815955,-0.743400884156524,
-4.28303903351179));
#53434=CARTESIAN_POINT('Ctrl Pts',(0.13418270773351,-0.773272755951178,
-4.26718152293586));
#53435=CARTESIAN_POINT('Ctrl Pts',(0.487363321704981,-0.615168876657226,
-4.25132401235991));
#53436=CARTESIAN_POINT('Ctrl Pts',(0.722070233162724,-0.30752289757245,
-4.23546650178397));
#53437=CARTESIAN_POINT('Ctrl Pts',(0.781248272857062,0.0748791713955384,
-4.21960899120802));
#53438=CARTESIAN_POINT('Ctrl Pts',(0.65051178401439,0.439078777680545,-4.20375148063208));
#53439=CARTESIAN_POINT('Ctrl Pts',(0.361641647954727,0.696542226010465,
-4.18789397005614));
#53440=CARTESIAN_POINT('Ctrl Pts',(-0.0151403663859606,0.78468243478284,
-4.17203645948019));
#53441=CARTESIAN_POINT('Ctrl Pts',(-0.388241891893626,0.682073300701532,
-4.15617894890425));
#53442=CARTESIAN_POINT('Ctrl Pts',(-0.666965255658098,0.413658194522911,
-4.14032143832831));
#53443=CARTESIAN_POINT('Ctrl Pts',(-0.783555279126468,0.0446864487743974,
-4.12446392775236));
#53444=CARTESIAN_POINT('Ctrl Pts',(-0.709669961287797,-0.335148176478406,
-4.10860641717643));
#53445=CARTESIAN_POINT('Ctrl Pts',(-0.463270167836958,-0.63351125147336,
-4.09274890660047));
#53446=CARTESIAN_POINT('Ctrl Pts',(-0.104253503966341,-0.777873357984297,
-4.07689139602453));
#53447=CARTESIAN_POINT('Ctrl Pts',(0.280106262400609,-0.733141347841593,
-4.06103388544859));
#53448=CARTESIAN_POINT('Ctrl Pts',(0.596374679817071,-0.510189176114225,
-4.04517637487265));
#53449=CARTESIAN_POINT('Ctrl Pts',(0.767669700064063,-0.163214539041649,
-4.0293188642967));
#53450=CARTESIAN_POINT('Ctrl Pts',(0.752351022431571,0.223436105401952,
-4.01346135372076));
#53451=CARTESIAN_POINT('Ctrl Pts',(0.554142481635739,0.555771413620393,
-3.99760384314482));
#53452=CARTESIAN_POINT('Ctrl Pts',(0.22122681661509,0.75300361869076,-3.98174633256887));
#53453=CARTESIAN_POINT('Ctrl Pts',(-0.165467126114326,0.76718732023313,
-3.96588882199293));
#53454=CARTESIAN_POINT('Ctrl Pts',(-0.511937477526917,0.59487458615611,
-3.95003131141698));
#53455=CARTESIAN_POINT('Ctrl Pts',(-0.733960367021422,0.277953114378677,
-3.93417380084104));
#53456=CARTESIAN_POINT('Ctrl Pts',(-0.77756399863012,-0.106536295155054,
-3.9183162902651));
#53457=CARTESIAN_POINT('Ctrl Pts',(-0.632148716101378,-0.465127675893839,
-3.90245877968915));
#53458=CARTESIAN_POINT('Ctrl Pts',(-0.333063685357226,-0.710650642473002,
-3.88660126911321));
#53459=CARTESIAN_POINT('Ctrl Pts',(0.0469861743344437,-0.783420738538645,
-3.87074375853727));
#53460=CARTESIAN_POINT('Ctrl Pts',(0.415614111627677,-0.665748198921305,
-3.85488624796133));
#53461=CARTESIAN_POINT('Ctrl Pts',(0.683209943244133,-0.386238174710081,
-3.83902873738538));
#53462=CARTESIAN_POINT('Ctrl Pts',(0.784723495038708,-0.0128370746379034,
-3.82317122680944));
#53463=CARTESIAN_POINT('Ctrl Pts',(0.695477722595448,0.363684604464468,
-3.8073137162335));
#53464=CARTESIAN_POINT('Ctrl Pts',(0.437167481936875,0.651797780671273,
-3.79145620565755));
#53465=CARTESIAN_POINT('Ctrl Pts',(0.0725857023728426,0.781464695275524,
-3.77559869508161));
#53466=CARTESIAN_POINT('Ctrl Pts',(-0.309641017888792,0.721164470971649,
-3.75974118450566));
#53467=CARTESIAN_POINT('Ctrl Pts',(-0.616596751997694,0.485555557662479,
-3.74388367392972));
#53468=CARTESIAN_POINT('Ctrl Pts',(-0.773663282480133,0.131912393250565,
-3.72802616335378));
#53469=CARTESIAN_POINT('Ctrl Pts',(-0.74265912833721,-0.253797504417287,
-3.71216865277783));
#53470=CARTESIAN_POINT('Ctrl Pts',(-0.531121124556358,-0.577811478945351,
-3.69631114220189));
#53471=CARTESIAN_POINT('Ctrl Pts',(-0.190472284347944,-0.761364605853399,
-3.68045363162595));
#53472=CARTESIAN_POINT('Ctrl Pts',(0.196478679446638,-0.759836747383233,
-3.66459612105));
#53473=CARTESIAN_POINT('Ctrl Pts',(0.535667418259626,-0.573599312382862,
-3.64873861047406));
#53474=CARTESIAN_POINT('Ctrl Pts',(0.744640156953499,-0.247924970108488,
-3.63288109989812));
#53475=CARTESIAN_POINT('Ctrl Pts',(0.772597475516741,0.138017734281446,
-3.61702358932217));
#53476=CARTESIAN_POINT('Ctrl Pts',(0.612743197677913,0.490409551141159,
-3.60116607874623));
#53477=CARTESIAN_POINT('Ctrl Pts',(0.303936481101913,0.723587154119262,
-3.58530856817028));
#53478=CARTESIAN_POINT('Ctrl Pts',(-0.0787544993106969,0.78086713529854,
-3.56945105759435));
#53479=CARTESIAN_POINT('Ctrl Pts',(-0.442300959183037,0.648325239102095,
-3.55359354701839));
#53480=CARTESIAN_POINT('Ctrl Pts',(-0.698327977345097,0.358181225370803,
-3.53773603644246));
#53481=CARTESIAN_POINT('Ctrl Pts',(-0.784597655632743,-0.0190334685916752,
-3.52187852586651));
#53482=CARTESIAN_POINT('Ctrl Pts',(-0.680138600126441,-0.391621295091407,
-3.50602101529057));
#53483=CARTESIAN_POINT('Ctrl Pts',(-0.410343881079456,-0.669009456892558,
-3.49016350471463));
#53484=CARTESIAN_POINT('Ctrl Pts',(-0.0407982026757765,-0.783767351201523,
-3.47430599413868));
#53485=CARTESIAN_POINT('Ctrl Pts',(0.338665157079046,-0.707998351362241,
-3.45844848356274));
#53486=CARTESIAN_POINT('Ctrl Pts',(0.635802019773763,-0.460121229463095,
-3.4425909729868));
#53487=CARTESIAN_POINT('Ctrl Pts',(0.778381048520723,-0.10039271614418,
-3.42673346241085));
#53488=CARTESIAN_POINT('Ctrl Pts',(0.731742545545852,0.283740376381475,
-3.41087595183491));
#53489=CARTESIAN_POINT('Ctrl Pts',(0.507223917422551,0.59889869906817,-3.39501844125896));
#53490=CARTESIAN_POINT('Ctrl Pts',(0.159403652051826,0.768470057883562,
-3.37916093068303));
#53491=CARTESIAN_POINT('Ctrl Pts',(-0.227166227850259,0.751233158929577,
-3.36330342010708));
#53492=CARTESIAN_POINT('Ctrl Pts',(-0.558514011831493,0.551378139518531,
-3.34744590953114));
#53493=CARTESIAN_POINT('Ctrl Pts',(-0.754091991355572,0.217487982942537,
-3.33158839895519));
#53494=CARTESIAN_POINT('Ctrl Pts',(-0.766356893606415,-0.169271574025148,
-3.31573088837925));
#53495=CARTESIAN_POINT('Ctrl Pts',(-0.592327229588209,-0.514882712119356,
-3.2998733778033));
#53496=CARTESIAN_POINT('Ctrl Pts',(-0.274308067666229,-0.735330427878682,
-3.28401586722736));
#53497=CARTESIAN_POINT('Ctrl Pts',(0.110392953473453,-0.777025836104844,
-3.26815835665142));
#53498=CARTESIAN_POINT('Ctrl Pts',(0.468258426374354,-0.629833152732085,
-3.25230084607548));
#53499=CARTESIAN_POINT('Ctrl Pts',(0.712294427431246,-0.329533614069066,
-3.23644333549953));
#53500=CARTESIAN_POINT('Ctrl Pts',(0.78317796842517,0.050872624509148,-3.22058582492359));
#53501=CARTESIAN_POINT('Ctrl Pts',(0.663677888998276,0.418912179108962,
-3.20472831434765));
#53502=CARTESIAN_POINT('Ctrl Pts',(0.382843598964291,0.685117897068157,
-3.1888708037717));
#53503=CARTESIAN_POINT('Ctrl Pts',(0.00894342433664182,0.784777528546888,
-3.17301329319576));
#53504=CARTESIAN_POINT('Ctrl Pts',(-0.367130817454304,0.693664700721004,
-3.15715578261982));
#53505=CARTESIAN_POINT('Ctrl Pts',(-0.653958812526187,0.433928134223127,
-3.14129827204387));
#53506=CARTESIAN_POINT('Ctrl Pts',(-0.781815218311425,0.0687074855287506,
-3.12544076146793));
#53507=CARTESIAN_POINT('Ctrl Pts',(-0.719619276146273,-0.313215343732932,
-3.10958325089198));
#53508=CARTESIAN_POINT('Ctrl Pts',(-0.482490268138086,-0.618998299919365,
-3.09372574031604));
#53509=CARTESIAN_POINT('Ctrl Pts',(-0.128072153733491,-0.774308257471849,
-3.07786822974009));
#53510=CARTESIAN_POINT('Ctrl Pts',(0.257479165748238,-0.74139074269687,
-3.06201071916415));
#53511=CARTESIAN_POINT('Ctrl Pts',(0.58043958286246,-0.528247711587546,
-3.04615320858821));
#53512=CARTESIAN_POINT('Ctrl Pts',(0.762300283595343,-0.186692345267518,
-3.03029569801227));
#53513=CARTESIAN_POINT('Ctrl Pts',(0.758852543986716,0.200246274961393,
-3.01443818743632));
#53514=CARTESIAN_POINT('Ctrl Pts',(0.570934478967572,0.538506801142803,
-2.99858067686038));
#53515=CARTESIAN_POINT('Ctrl Pts',(0.244227304051109,0.745861098400332,
-2.98272316628443));
#53516=CARTESIAN_POINT('Ctrl Pts',(-0.141849363146094,0.771903175486456,
-2.96686565570849));
#53517=CARTESIAN_POINT('Ctrl Pts',(-0.493443707807536,0.610302434352163,
-2.95100814513255));
#53518=CARTESIAN_POINT('Ctrl Pts',(-0.72508626200279,0.300342582405237,
-2.93515063455661));
#53519=CARTESIAN_POINT('Ctrl Pts',(-0.780466774563917,-0.0826278884688641,
-2.91929312398066));
#53520=CARTESIAN_POINT('Ctrl Pts',(-0.646122733894283,-0.445512252240051,
-2.90343561340472));
#53521=CARTESIAN_POINT('Ctrl Pts',(-0.354711985178273,-0.700096537430314,
-2.88757810282877));
#53522=CARTESIAN_POINT('Ctrl Pts',(0.0229261022366121,-0.784493561469602,
-2.87172059225283));
#53523=CARTESIAN_POINT('Ctrl Pts',(0.394991057461987,-0.678187156083102,
-2.85586308167689));
#53524=CARTESIAN_POINT('Ctrl Pts',(0.671037188633014,-0.407019465901235,
-2.84000557110095));
#53525=CARTESIAN_POINT('Ctrl Pts',(0.783960128703746,-0.0369089522180315,
-2.824148060525));
#53526=CARTESIAN_POINT('Ctrl Pts',(0.706309312124615,0.342173800512369,
-2.80829054994906));
#53527=CARTESIAN_POINT('Ctrl Pts',(0.456960963949165,0.638077136071867,
-2.79243303937312));
#53528=CARTESIAN_POINT('Ctrl Pts',(0.0965294568812757,0.778869577082859,
-2.77657552879717));
#53529=CARTESIAN_POINT('Ctrl Pts',(-0.287367505318435,0.730325729409888,
-2.76071801822123));
#53530=CARTESIAN_POINT('Ctrl Pts',(-0.601407974792955,0.504246172029558,
-2.74486050764528));
#53531=CARTESIAN_POINT('Ctrl Pts',(-0.769251497714866,0.155588840905967,
-2.72900299706934));
#53532=CARTESIAN_POINT('Ctrl Pts',(-0.750096801772698,-0.230890757981771,
-2.7131454864934));
#53533=CARTESIAN_POINT('Ctrl Pts',(-0.548600223723299,-0.561242860695591,
-2.69728797591745));
#53534=CARTESIAN_POINT('Ctrl Pts',(-0.213743795209606,-0.755161799987539,
-2.68143046534151));
#53535=CARTESIAN_POINT('Ctrl Pts',(0.173071854854098,-0.76550760101281,
-2.66557295476557));
#53536=CARTESIAN_POINT('Ctrl Pts',(0.51781527146833,-0.589765291268659,
-2.64971544418963));
#53537=CARTESIAN_POINT('Ctrl Pts',(0.736682386570194,-0.270656268111916,
-2.63385793361368));
#53538=CARTESIAN_POINT('Ctrl Pts',(0.776468544967536,0.114246894167955,
-2.61800042303774));
#53539=CARTESIAN_POINT('Ctrl Pts',(0.627502084300454,0.471377649395485,
-2.60214291246179));
#53540=CARTESIAN_POINT('Ctrl Pts',(0.325995430411447,0.713920677317781,
-2.58628540188585));
#53541=CARTESIAN_POINT('Ctrl Pts',(-0.0547578223153314,0.782915918248127,
-2.57042789130991));
#53542=CARTESIAN_POINT('Ctrl Pts',(-0.422199933923428,0.661591240832344,
-2.55457038073396));
#53543=CARTESIAN_POINT('Ctrl Pts',(-0.687008984844947,0.379439598478257,
-2.53871287015802));
#53544=CARTESIAN_POINT('Ctrl Pts',(-0.784812242613961,0.00504955386858817,
-2.52285535958208));
#53545=CARTESIAN_POINT('Ctrl Pts',(-0.691834602396433,-0.370567992516886,
-2.50699784900614));
#53546=CARTESIAN_POINT('Ctrl Pts',(-0.430678104183853,-0.656103745399787,
-2.49114033843019));
#53547=CARTESIAN_POINT('Ctrl Pts',(-0.0648275772623532,-0.782146494831576,
-2.47528282785425));
#53548=CARTESIAN_POINT('Ctrl Pts',(0.316781958926394,-0.718056365928039,
-2.4594253172783));
#53549=CARTESIAN_POINT('Ctrl Pts',(0.621384609508185,-0.479413100798661,
-2.44356780670236));
#53550=CARTESIAN_POINT('Ctrl Pts',(0.774934170752148,-0.124228761370738,
-2.42771029612641));
#53551=CARTESIAN_POINT('Ctrl Pts',(0.740104105699592,0.261154488526679,
-2.41185278555047));
#53552=CARTESIAN_POINT('Ctrl Pts',(0.525361294359332,0.583053397674786,
-2.39599527497453));
#53553=CARTESIAN_POINT('Ctrl Pts',(0.1829078102454,0.763217195234921,-2.38013776439859));
#53554=CARTESIAN_POINT('Ctrl Pts',(-0.20400894086746,0.757849659363361,
-2.36428025382264));
#53555=CARTESIAN_POINT('Ctrl Pts',(-0.541332927211076,0.568255590441586,
-2.3484227432467));
#53556=CARTESIAN_POINT('Ctrl Pts',(-0.747063678440222,0.240523625671967,
-2.33256523267075));
#53557=CARTESIAN_POINT('Ctrl Pts',(-0.771189872952408,-0.14567750000146,
-2.31670772209481));
#53558=CARTESIAN_POINT('Ctrl Pts',(-0.607846646766021,-0.496465717010077,
-2.30085021151887));
#53559=CARTESIAN_POINT('Ctrl Pts',(-0.296741289956032,-0.726567519908682,
-2.28499270094293));
#53560=CARTESIAN_POINT('Ctrl Pts',(0.0864992435160036,-0.780047200509165,
-2.26913519036698));
#53561=CARTESIAN_POINT('Ctrl Pts',(0.448712577796839,-0.64390432261163,
-2.25327767979104));
#53562=CARTESIAN_POINT('Ctrl Pts',(0.701847862728175,-0.351234012781961,
-2.23742016921509));
#53563=CARTESIAN_POINT('Ctrl Pts',(0.784370154855984,0.0268181714929559,
-2.22156265863915));
#53564=CARTESIAN_POINT('Ctrl Pts',(0.67621901661164,0.398351096049469,-2.2057051480632));
#53565=CARTESIAN_POINT('Ctrl Pts',(0.403685030827794,0.67304840096132,-2.18984763748727));
#53566=CARTESIAN_POINT('Ctrl Pts',(0.0330187931456675,0.78413360688739,
-2.17399012691132));
#53567=CARTESIAN_POINT('Ctrl Pts',(-0.345674020403545,0.704602885155229,
-2.15813261633538));
#53568=CARTESIAN_POINT('Ctrl Pts',(-0.640336544359476,0.453789449093728,
-2.14227510575943));
#53569=CARTESIAN_POINT('Ctrl Pts',(-0.779338931644242,0.092663821282302,
-2.12641759518349));
#53570=CARTESIAN_POINT('Ctrl Pts',(-0.728890934312499,-0.290987559919799,
-2.11056008460755));
#53571=CARTESIAN_POINT('Ctrl Pts',(-0.501256013240592,-0.60390244521874,
-2.0947025740316));
#53572=CARTESIAN_POINT('Ctrl Pts',(-0.151770199516093,-0.77001400032069,
-2.07884506345566));
#53573=CARTESIAN_POINT('Ctrl Pts',(0.23460960410698,-0.748941978935479,
-2.06298755287972));
#53574=CARTESIAN_POINT('Ctrl Pts',(0.563957893034617,-0.545808802636034,
-2.04713004230377));
#53575=CARTESIAN_POINT('Ctrl Pts',(0.7562130182504,-0.209994345589698,-2.03127253172783));
#53576=CARTESIAN_POINT('Ctrl Pts',(0.764639463359969,0.176867875046899,
-2.01541502115189));
#53577=CARTESIAN_POINT('Ctrl Pts',(0.587188834266557,0.520735083380895,
-1.99955751057594));
#53578=CARTESIAN_POINT('Ctrl Pts',(0.266997805614742,0.738016209813808,
-1.9837));
#53579=CARTESIAN_POINT('Ctrl Pts',(-0.118098022363289,0.775892138937434,
-1.96784248942406));
#53580=CARTESIAN_POINT('Ctrl Pts',(-0.474485268169029,0.625155568192103,
-1.95198497884811));
#53581=CARTESIAN_POINT('Ctrl Pts',(-0.715529352098025,0.322449221486431,
-1.93612746827217));
#53582=CARTESIAN_POINT('Ctrl Pts',(-0.782634594458599,-0.0586416721082485,
-1.92026995769623));
#53583=CARTESIAN_POINT('Ctrl Pts',(-0.659488305792038,-0.425477295134033,
-1.90441244712028));
#53584=CARTESIAN_POINT('Ctrl Pts',(-0.376026257050732,-0.688883160020217,
-1.88855493654434));
#53585=CARTESIAN_POINT('Ctrl Pts',(-0.00115555909198516,-0.784827636385346,
-1.8726974259684));
#53586=CARTESIAN_POINT('Ctrl Pts',(0.373996045036767,-0.6899874726746,-1.85683991539245));
#53587=CARTESIAN_POINT('Ctrl Pts',(0.658232526488693,-0.427417471827413,
-1.84098240481651));
#53588=CARTESIAN_POINT('Ctrl Pts',(0.782458516680696,-0.0609460730881939,
-1.82512489424057));
#53589=CARTESIAN_POINT('Ctrl Pts',(0.716475778792257,0.320340775667187,
-1.80926738366462));
#53590=CARTESIAN_POINT('Ctrl Pts',(0.476324131397102,0.623755622018608,
-1.79340987308868));
#53591=CARTESIAN_POINT('Ctrl Pts',(0.120382310777934,0.77554100691246,-1.77755236251274));
#53592=CARTESIAN_POINT('Ctrl Pts',(-0.264823382274487,0.738799249019466,
-1.76169485193679));
#53593=CARTESIAN_POINT('Ctrl Pts',(-0.585652859036139,0.522461943928764,
-1.74583734136085));
#53594=CARTESIAN_POINT('Ctrl Pts',(-0.764115318199852,0.179118772448241,
-1.72997983078491));
#53595=CARTESIAN_POINT('Ctrl Pts',(-0.756828118201908,-0.207766584536555,
-1.71412232020896));
#53596=CARTESIAN_POINT('Ctrl Pts',(-0.565562712753049,-0.544145726891646,
-1.69826480963302));
#53597=CARTESIAN_POINT('Ctrl Pts',(-0.236814026147216,-0.748247867468375,
-1.68240729905707));
#53598=CARTESIAN_POINT('Ctrl Pts',(0.149502050607495,-0.77045758547449,
-1.66654978848113));
#53599=CARTESIAN_POINT('Ctrl Pts',(0.499475504353768,-0.605375895375407,
-1.65069227790519));
#53600=CARTESIAN_POINT('Ctrl Pts',(0.728030891371734,-0.293132692409946,
-1.63483476732925));
#53601=CARTESIAN_POINT('Ctrl Pts',(0.779608423463245,0.0903684691481552,
-1.6189772567533));
#53602=CARTESIAN_POINT('Ctrl Pts',(0.641670059866376,0.451901857068663,
-1.60311974617736));
#53603=CARTESIAN_POINT('Ctrl Pts',(0.347747393801637,0.703581910125037,
-1.58726223560141));
#53604=CARTESIAN_POINT('Ctrl Pts',(-0.0307095805468093,0.784227438829875,
-1.57140472502547));
#53605=CARTESIAN_POINT('Ctrl Pts',(-0.401701328137329,0.674234230163178,
-1.55554721444953));
#53606=CARTESIAN_POINT('Ctrl Pts',(-0.675043044365986,0.400340657945363,
-1.53968970387359));
#53607=CARTESIAN_POINT('Ctrl Pts',(-0.78428778148182,0.0291278212255782,
-1.52383219329764));
#53608=CARTESIAN_POINT('Ctrl Pts',(-0.702879112462439,-0.349165730585115,
-1.5079746827217));
#53609=CARTESIAN_POINT('Ctrl Pts',(-0.450606762972262,-0.642580189015103,
-1.49211717214575));
#53610=CARTESIAN_POINT('Ctrl Pts',(-0.0887959045103961,-0.779789100650431,
-1.47625966156981));
#53611=CARTESIAN_POINT('Ctrl Pts',(0.294600451068075,-0.727438195575069,
-1.46040215099386));
#53612=CARTESIAN_POINT('Ctrl Pts',(0.606382048937353,-0.498253514666544,
-1.44454464041793));
#53613=CARTESIAN_POINT('Ctrl Pts',(0.770757546929961,-0.147947821888442,
-1.42868712984198));
#53614=CARTESIAN_POINT('Ctrl Pts',(0.747768718847025,0.238322674676382,
-1.41282961926604));
#53615=CARTESIAN_POINT('Ctrl Pts',(0.543003944975163,0.566659042010658,
-1.39697210869009));
#53616=CARTESIAN_POINT('Ctrl Pts',(0.206239726385727,0.757245620265555,
-1.38111459811415));
#53617=CARTESIAN_POINT('Ctrl Pts',(-0.180659541154162,0.763752502019466,
-1.3652570875382));
#53618=CARTESIAN_POINT('Ctrl Pts',(-0.52364207597792,0.584597922008419,
-1.34939957696226));
#53619=CARTESIAN_POINT('Ctrl Pts',(-0.739331864773827,0.263332770237737,
-1.33354206638632));
#53620=CARTESIAN_POINT('Ctrl Pts',(-0.775296632204346,-0.121946243253436,
-1.31768455581038));
#53621=CARTESIAN_POINT('Ctrl Pts',(-0.622793662172921,-0.477581206192484,
-1.30182704523443));
#53622=CARTESIAN_POINT('Ctrl Pts',(-0.318895074593618,-0.71712041217006,
-1.28596953465849));
#53623=CARTESIAN_POINT('Ctrl Pts',(0.062524078276333,-0.782334003982136,
-1.27011202408255));
#53624=CARTESIAN_POINT('Ctrl Pts',(0.428744182059569,-0.657369135646856,
-1.2542545135066));
#53625=CARTESIAN_POINT('Ctrl Pts',(0.690740376456031,-0.372603658710436,
-1.23839700293066));
#53626=CARTESIAN_POINT('Ctrl Pts',(0.784823709482088,0.00273846413186627,
-1.22253949235471));
#53627=CARTESIAN_POINT('Ctrl Pts',(0.688123357027629,0.377414890623108,
-1.20668198177877));
#53628=CARTESIAN_POINT('Ctrl Pts',(0.424146317423146,0.660345103387168,
-1.19082447120283));
#53629=CARTESIAN_POINT('Ctrl Pts',(0.0570630685600556,0.78275127617752,
-1.17496696062689));
#53630=CARTESIAN_POINT('Ctrl Pts',(-0.32389170634536,0.714877553649376,
-1.15910945005094));
#53631=CARTESIAN_POINT('Ctrl Pts',(-0.626111279081718,0.473223435976791,
-1.143251939475));
#53632=CARTESIAN_POINT('Ctrl Pts',(-0.776128751013863,0.116532896645915,
-1.12739442889905));
#53633=CARTESIAN_POINT('Ctrl Pts',(-0.737476204779087,-0.268485756671859,
-1.11153691832311));
#53634=CARTESIAN_POINT('Ctrl Pts',(-0.519549731671247,-0.588237902953695,
-1.09567940774717));
#53635=CARTESIAN_POINT('Ctrl Pts',(-0.17532532515354,-0.764994630380392,
-1.07982189717122));
#53636=CARTESIAN_POINT('Ctrl Pts',(0.211519113464033,-0.755787945650376,
-1.06396438659528));
#53637=CARTESIAN_POINT('Ctrl Pts',(0.546945130939781,-0.562855912194491,
-1.04810687601934));
#53638=CARTESIAN_POINT('Ctrl Pts',(0.74941363633275,-0.233098596798759,
-1.03224936544339));
#53639=CARTESIAN_POINT('Ctrl Pts',(0.769706331079953,0.153322920812463,
-1.01639185486745));
#53640=CARTESIAN_POINT('Ctrl Pts',(0.602890241004603,0.502472995744484,
-1.00053434429151));
#53641=CARTESIAN_POINT('Ctrl Pts',(0.289516878602456,0.729476340367059,
-0.984676833715564));
#53642=CARTESIAN_POINT('Ctrl Pts',(-0.0942354701137554,0.77915045422785,
-0.96881932313962));
#53643=CARTESIAN_POINT('Ctrl Pts',(-0.455080011542695,0.639420000661008,
-0.952961812563677));
#53644=CARTESIAN_POINT('Ctrl Pts',(-0.705298636932576,0.344252214069966,
-0.937104301987735));
#53645=CARTESIAN_POINT('Ctrl Pts',(-0.784065416904622,-0.0346002336004862,
-0.92124679141179));
#53646=CARTESIAN_POINT('Ctrl Pts',(-0.672232845598666,-0.405041671250436,
-0.905389280835848));
#53647=CARTESIAN_POINT('Ctrl Pts',(-0.39698642958483,-0.677021069743413,
-0.889531770259904));
#53648=CARTESIAN_POINT('Ctrl Pts',(-0.0252361322446689,-0.784422648691607,
-0.87367425968396));
#53649=CARTESIAN_POINT('Ctrl Pts',(0.352648845099092,-0.70113803648162,
-0.857816749108016));
#53650=CARTESIAN_POINT('Ctrl Pts',(0.644808014805302,-0.447412983935282,
-0.841959238532074));
#53651=CARTESIAN_POINT('Ctrl Pts',(0.780220073019283,-0.0849258017849115,
-0.82610172795613));
#53652=CARTESIAN_POINT('Ctrl Pts',(0.725967548960737,0.298206089822066,
-0.810244217380186));
#53653=CARTESIAN_POINT('Ctrl Pts',(0.495238750222128,0.608846724906565,
-0.794386706804243));
#53654=CARTESIAN_POINT('Ctrl Pts',(0.144121802121297,0.771482119238247,
-0.778529196228299));
#53655=CARTESIAN_POINT('Ctrl Pts',(-0.242029878282588,0.746577050390341,
-0.762671685652355));
#53656=CARTESIAN_POINT('Ctrl Pts',(-0.569346241127547,0.540185719789925,
-0.746814175076413));
#53657=CARTESIAN_POINT('Ctrl Pts',(-0.758259580612683,0.202480030027912,
-0.730956664500469));
#53658=CARTESIAN_POINT('Ctrl Pts',(-0.762846738826278,-0.184446759833668,
-0.715099153924525));
#53659=CARTESIAN_POINT('Ctrl Pts',(-0.58199261827663,-0.526536177695834,
-0.699241643348582));
#53660=CARTESIAN_POINT('Ctrl Pts',(-0.259661252205769,-0.740629319061807,
-0.683384132772639));
#53661=CARTESIAN_POINT('Ctrl Pts',(0.12579146210391,-0.774682039428296,
-0.667526622196696));
#53662=CARTESIAN_POINT('Ctrl Pts',(0.480665387250857,-0.620416424387693,
-0.651669111620751));
#53663=CARTESIAN_POINT('Ctrl Pts',(0.718693818365588,-0.315333077228062,
-0.63581160104481));
#53664=CARTESIAN_POINT('Ctrl Pts',(0.782014154218595,0.0664049452435352,
-0.619954090468865));
#53665=CARTESIAN_POINT('Ctrl Pts',(0.655233782565965,0.432000514276696,
-0.604096579892922));
#53666=CARTESIAN_POINT('Ctrl Pts',(0.369171887713958,0.692580588431942,
-0.588239069316979));
#53667=CARTESIAN_POINT('Ctrl Pts',(-0.00663241994093424,0.784800462000848,
-0.572381558741035));
#53668=CARTESIAN_POINT('Ctrl Pts',(-0.380824445111711,0.686242301345836,
-0.556524048165091));
#53669=CARTESIAN_POINT('Ctrl Pts',(-0.66244142408827,0.420864721499445,
-0.540666537589149));
#53670=CARTESIAN_POINT('Ctrl Pts',(-0.78302476611513,0.0531786592687593,
-0.524809027013205));
#53671=CARTESIAN_POINT('Ctrl Pts',(-0.713261729843775,-0.327434663545121,
-0.508951516437261));
#53672=CARTESIAN_POINT('Ctrl Pts',(-0.470111090870426,-0.628451522706413,
-0.493094005861318));
#53673=CARTESIAN_POINT('Ctrl Pts',(-0.112680613737367,-0.776697388587739,
-0.477236495285375));
#53674=CARTESIAN_POINT('Ctrl Pts',(0.27214152155714,-0.736135005548202,
-0.46137898470943));
#53675=CARTESIAN_POINT('Ctrl Pts',(0.590808465794012,-0.516624729280032,
-0.445521474133488));
#53676=CARTESIAN_POINT('Ctrl Pts',(0.765855110121114,-0.171527561745056,
-0.429663963557544));
#53677=CARTESIAN_POINT('Ctrl Pts',(0.754729167332557,0.215266435266626,
-0.4138064529816));
#53678=CARTESIAN_POINT('Ctrl Pts',(0.560135255367789,0.549731070449319,
-0.397948942405656));
#53679=CARTESIAN_POINT('Ctrl Pts',(0.229377429157334,0.750560956317521,
-0.382091431829714));
#53680=CARTESIAN_POINT('Ctrl Pts',(-0.157140016682746,0.768936128296654,
-0.36623392125377));
#53681=CARTESIAN_POINT('Ctrl Pts',(-0.505458117141541,0.600389744778999,
-0.350376410677827));
#53682=CARTESIAN_POINT('Ctrl Pts',(-0.730903831797943,0.285893937675275,
-0.334518900101885));
#53683=CARTESIAN_POINT('Ctrl Pts',(-0.778673303125677,-0.0981001514671905,
-0.31866138952594));
#53684=CARTESIAN_POINT('Ctrl Pts',(-0.637154202245931,-0.45824696248919,
-0.302803878949997));
#53685=CARTESIAN_POINT('Ctrl Pts',(-0.34074855599798,-0.706998001847843,
-0.286946368374054));
#53686=CARTESIAN_POINT('Ctrl Pts',(0.0384900277778693,-0.783884091195167,
-0.27108885779811));
#53687=CARTESIAN_POINT('Ctrl Pts',(0.408372057023997,-0.670214915848524,
-0.255231347222166));
#53688=CARTESIAN_POINT('Ctrl Pts',(0.678982401305158,-0.393622421166732,
-0.239373836646223));
#53689=CARTESIAN_POINT('Ctrl Pts',(0.784538258134674,-0.0213438359833095,
-0.223516326070279));
#53690=CARTESIAN_POINT('Ctrl Pts',(0.69937959664011,0.356123305506083,-0.207658815494336));
#53691=CARTESIAN_POINT('Ctrl Pts',(0.444208392702825,0.647019913531816,
-0.191801304918393));
#53692=CARTESIAN_POINT('Ctrl Pts',(0.0810532135089025,0.780631942388513,
-0.17594379434245));
#53693=CARTESIAN_POINT('Ctrl Pts',(-0.301803615892741,0.724478826986905,
-0.160086283766505));
#53694=CARTESIAN_POINT('Ctrl Pts',(-0.611297919935612,0.492212192112627,
-0.144228773190563));
#53695=CARTESIAN_POINT('Ctrl Pts',(-0.772184753739812,0.140291456659345,
-0.128371262614619));
#53696=CARTESIAN_POINT('Ctrl Pts',(-0.745372760934995,-0.24572960271599,
-0.112513752038676));
#53697=CARTESIAN_POINT('Ctrl Pts',(-0.537342918516762,-0.572022410205874,
-0.0966562414627321));
#53698=CARTESIAN_POINT('Ctrl Pts',(-0.19873767733096,-0.75924888856303,
-0.0807987308867897));
#53699=CARTESIAN_POINT('Ctrl Pts',(0.188276175770941,-0.761935501840704,
-0.0649412203108454));
#53700=CARTESIAN_POINT('Ctrl Pts',(0.415619971558626,-0.640197744227128,
-0.0543695465935496));
#53701=CARTESIAN_POINT('Ctrl Pts',(0.507924469142728,-0.555852079925216,
-0.0490837097349018));
#53702=CARTESIAN_POINT('Ctrl Pts',(0.415028236876536,-0.582012248186925,
-5.8309162902651));
#53703=CARTESIAN_POINT('Ctrl Pts',(0.511676877939308,-0.513092882277098,
-5.82563045340645));
#53704=CARTESIAN_POINT('Ctrl Pts',(0.669882320706702,-0.326248849454983,
-5.81505877968916));
#53705=CARTESIAN_POINT('Ctrl Pts',(0.744325517095435,0.0335534201836676,
-5.79920126911321));
#53706=CARTESIAN_POINT('Ctrl Pts',(0.637835333840713,0.385103548525349,
-5.78334375853727));
#53707=CARTESIAN_POINT('Ctrl Pts',(0.376290719986943,0.643085420323738,
-5.76748624796132));
#53708=CARTESIAN_POINT('Ctrl Pts',(0.0232743040931315,0.744715053663492,
-5.75162873738539));
#53709=CARTESIAN_POINT('Ctrl Pts',(-0.335400465408995,0.665323262153351,
-5.73577122680943));
#53710=CARTESIAN_POINT('Ctrl Pts',(-0.612542060764352,0.424191040961468,
-5.7199137162335));
#53711=CARTESIAN_POINT('Ctrl Pts',(-0.740780262763952,0.0799449338940462,
-5.70405620565754));
#53712=CARTESIAN_POINT('Ctrl Pts',(-0.688941273521715,-0.283736713152371,
-5.68819869508162));
#53713=CARTESIAN_POINT('Ctrl Pts',(-0.469626808375355,-0.578443643881164,
-5.67234118450566));
#53714=CARTESIAN_POINT('Ctrl Pts',(-0.136150209639541,-0.732536481667968,
-5.65648367392972));
#53715=CARTESIAN_POINT('Ctrl Pts',(0.230423287598442,-0.708555976232628,
-5.64062616335378));
#53716=CARTESIAN_POINT('Ctrl Pts',(0.540982931862801,-0.512331907284304,
-5.62476865277783));
#53717=CARTESIAN_POINT('Ctrl Pts',(0.72003441906891,-0.1915644366118,-5.60891114220189));
#53718=CARTESIAN_POINT('Ctrl Pts',(0.724051924255098,0.175770620786611,
-5.59305363162594));
#53719=CARTESIAN_POINT('Ctrl Pts',(0.552058825433282,0.500377413708016,
-5.57719612105001));
#53720=CARTESIAN_POINT('Ctrl Pts',(0.245865121098944,0.703346886034275,
-5.56133861047405));
#53721=CARTESIAN_POINT('Ctrl Pts',(-0.120096214505419,0.73533897022222,
-5.54548109989812));
#53722=CARTESIAN_POINT('Ctrl Pts',(-0.456863225048667,0.588576668292261,
-5.52962358932217));
#53723=CARTESIAN_POINT('Ctrl Pts',(-0.682570836208337,0.298736597689061,
-5.51376607874623));
#53724=CARTESIAN_POINT('Ctrl Pts',(-0.742351528775239,-0.0637236917238471,
-5.49790856817029));
#53725=CARTESIAN_POINT('Ctrl Pts',(-0.621673146443291,-0.410693316386423,
-5.48205105759435));
#53726=CARTESIAN_POINT('Ctrl Pts',(-0.349871533996248,-0.657827037205679,
-5.4661935470184));
#53727=CARTESIAN_POINT('Ctrl Pts',(0.00698074637971318,-0.745048837543795,
-5.45033603644245));
#53728=CARTESIAN_POINT('Ctrl Pts',(0.362136069204197,-0.651155871159418,
-5.43447852586652));
#53729=CARTESIAN_POINT('Ctrl Pts',(0.629259324324606,-0.398972685665058,
-5.41862101529057));
#53730=CARTESIAN_POINT('Ctrl Pts',(0.743415216753462,-0.049802777611032,
-5.40276350471463));
#53731=CARTESIAN_POINT('Ctrl Pts',(0.676853461153697,0.311473744130651,
-5.38690599413868));
#53732=CARTESIAN_POINT('Ctrl Pts',(0.445754630171398,0.597033760216781,
-5.37104848356274));
#53733=CARTESIAN_POINT('Ctrl Pts',(0.106296800681942,0.737460162532991,
-5.3551909729868));
#53734=CARTESIAN_POINT('Ctrl Pts',(-0.259000838619383,0.69861653770328,
-5.33933346241085));
#53735=CARTESIAN_POINT('Ctrl Pts',(-0.561337670369488,0.489945426534807,
-5.32347595183491));
#53736=CARTESIAN_POINT('Ctrl Pts',(-0.727218291306573,0.1621729260614,-5.30761844125897));
#53737=CARTESIAN_POINT('Ctrl Pts',(-0.716318593188485,-0.205022374902455,
-5.29176093068302));
#53738=CARTESIAN_POINT('Ctrl Pts',(-0.53128819599034,-0.522378554268369,
-5.27590342010708));
#53739=CARTESIAN_POINT('Ctrl Pts',(-0.217106348780294,-0.712749138531546,
-5.26004590953113));
#53740=CARTESIAN_POINT('Ctrl Pts',(0.149852126940193,-0.729856726494781,
-5.24418839895519));
#53741=CARTESIAN_POINT('Ctrl Pts',(0.48038287919956,-0.569542615201107,
-5.22833088837924));
#53742=CARTESIAN_POINT('Ctrl Pts',(0.69413681262924,-0.270777743751394,
-5.21247337780331));
#53743=CARTESIAN_POINT('Ctrl Pts',(0.739152241167806,0.093810796472393,
-5.19661586722736));
#53744=CARTESIAN_POINT('Ctrl Pts',(0.604486313247053,0.43559476380595,-5.18075835665142));
#53745=CARTESIAN_POINT('Ctrl Pts',(0.322875121988236,0.671489506067859,
-5.16490084607547));
#53746=CARTESIAN_POINT('Ctrl Pts',(-0.0372241487955211,0.744151102871337,
-5.14904333549953));
#53747=CARTESIAN_POINT('Ctrl Pts',(-0.388274559038646,0.635916164255573,
-5.13318582492358));
#53748=CARTESIAN_POINT('Ctrl Pts',(-0.64493886644525,0.37309564418054,-5.11732831434765));
#53749=CARTESIAN_POINT('Ctrl Pts',(-0.744824253486097,0.0195788808938151,
-5.1014708037717));
#53750=CARTESIAN_POINT('Ctrl Pts',(-0.663649468161454,-0.338697334750651,
-5.08561329319576));
#53751=CARTESIAN_POINT('Ctrl Pts',(-0.421147381083175,-0.614639231228336,
-5.06975578261981));
#53752=CARTESIAN_POINT('Ctrl Pts',(-0.0762680995817819,-0.741167780023092,
-5.05389827204387));
#53753=CARTESIAN_POINT('Ctrl Pts',(0.287151280730348,-0.687525012732699,
-5.03804076146793));
#53754=CARTESIAN_POINT('Ctrl Pts',(0.58076673059759,-0.46675101048542,-5.02218325089198));
#53755=CARTESIAN_POINT('Ctrl Pts',(0.733202937369596,-0.132513975831888,
-5.00632574031604));
#53756=CARTESIAN_POINT('Ctrl Pts',(0.707404010688734,0.233936031469435,
-4.9904682297401));
#53757=CARTESIAN_POINT('Ctrl Pts',(0.50964144089628,0.543518263611574,-4.97461071916415));
#53758=CARTESIAN_POINT('Ctrl Pts',(0.187989555333847,0.720976024735606,
-4.95875320858821));
#53759=CARTESIAN_POINT('Ctrl Pts',(-0.17936092440345,0.723170906463552,
-4.94289569801227));
#53760=CARTESIAN_POINT('Ctrl Pts',(-0.503110353643096,0.549569352507302,
-4.92703818743633));
#53761=CARTESIAN_POINT('Ctrl Pts',(-0.704558116518999,0.242372361471718,
-4.91118067686037));
#53762=CARTESIAN_POINT('Ctrl Pts',(-0.734734047924101,-0.123743201749595,
-4.89532316628444));
#53763=CARTESIAN_POINT('Ctrl Pts',(-0.586302646475458,-0.459777889740308,
-4.87946565570849));
#53764=CARTESIAN_POINT('Ctrl Pts',(-0.295346269863432,-0.684044649153792,
-4.86360814513255));
#53765=CARTESIAN_POINT('Ctrl Pts',(0.0674061663944642,-0.742026219139309,
-4.84775063455661));
#53766=CARTESIAN_POINT('Ctrl Pts',(0.413772761229021,-0.619627794101497,
-4.83189312398067));
#53767=CARTESIAN_POINT('Ctrl Pts',(0.659554866343183,-0.346603345975194,
-4.81603561340471));
#53768=CARTESIAN_POINT('Ctrl Pts',(0.745005031102745,0.0106773025514018,
-4.80017810282878));
#53769=CARTESIAN_POINT('Ctrl Pts',(0.649351078060994,0.365362393493366,
-4.78432059225283));
#53770=CARTESIAN_POINT('Ctrl Pts',(0.395845635128632,0.631231125902221,
-4.76846308167689));
#53771=CARTESIAN_POINT('Ctrl Pts',(0.0461136278878946,0.743653168137669,
-4.75260557110094));
#53772=CARTESIAN_POINT('Ctrl Pts',(-0.31482819344617,0.675299718472914,
-4.736748060525));
#53773=CARTESIAN_POINT('Ctrl Pts',(-0.599238072239317,0.44278689449563,
-4.72089054994906));
#53774=CARTESIAN_POINT('Ctrl Pts',(-0.737978488552156,0.102636502241902,
-4.70503303937312));
#53775=CARTESIAN_POINT('Ctrl Pts',(-0.697322877259977,-0.26246391372538,
-4.68917552879717));
#53776=CARTESIAN_POINT('Ctrl Pts',(-0.487154257012797,-0.563761679286988,
-4.67331801822123));
#53777=CARTESIAN_POINT('Ctrl Pts',(-0.15856275602498,-0.728013978959154,
-4.65746050764529));
#53778=CARTESIAN_POINT('Ctrl Pts',(0.208573945125506,-0.715292534962416,
-4.64160299706934));
#53779=CARTESIAN_POINT('Ctrl Pts',(0.525008169445223,-0.528689817543286,
-4.6257454864934));
#53780=CARTESIAN_POINT('Ctrl Pts',(0.713817562527057,-0.213567292875351,
-4.60988797591745));
#53781=CARTESIAN_POINT('Ctrl Pts',(0.729104234908342,0.153471547190018,
-4.59403046534152));
#53782=CARTESIAN_POINT('Ctrl Pts',(0.567152132065747,0.483202814821534,
-4.57817295476556));
#53783=CARTESIAN_POINT('Ctrl Pts',(0.267330374323152,0.695471762275377,
-4.56231544418963));
#53784=CARTESIAN_POINT('Ctrl Pts',(-0.0974770272500981,0.738677690414879,
-4.54645793361368));
#53785=CARTESIAN_POINT('Ctrl Pts',(-0.43858862773608,0.602317621175703,
-4.53060042303774));
#53786=CARTESIAN_POINT('Ctrl Pts',(-0.673083221372783,0.319539478413253,
-4.5147429124618));
#53787=CARTESIAN_POINT('Ctrl Pts',(-0.743957251490401,-0.0409158784950773,
-4.49888540188585));
#53788=CARTESIAN_POINT('Ctrl Pts',(-0.633981869740789,-0.391424948103911,
-4.48302789130991));
#53789=CARTESIAN_POINT('Ctrl Pts',(-0.369891116378875,-0.646782083226002,
-4.46717038073397));
#53790=CARTESIAN_POINT('Ctrl Pts',(-0.0158831121023146,-0.744912228325002,
-4.45131287015802));
#53791=CARTESIAN_POINT('Ctrl Pts',(0.341985935905684,-0.661960815155165,
-4.43545535958208));
#53792=CARTESIAN_POINT('Ctrl Pts',(0.616721234963047,-0.418092596805816,
-4.41959784900613));
#53793=CARTESIAN_POINT('Ctrl Pts',(0.741537069688743,-0.0725897750072806,
-4.40374033843019));
#53794=CARTESIAN_POINT('Ctrl Pts',(0.686091817285715,0.290558977510177,
-4.38788282785425));
#53795=CARTESIAN_POINT('Ctrl Pts',(0.463863727032172,0.58307541870842,-4.3720253172783));
#53796=CARTESIAN_POINT('Ctrl Pts',(0.128874477381027,0.733851395200652,
-4.35616780670236));
#53797=CARTESIAN_POINT('Ctrl Pts',(-0.237443015112518,0.706234603890558,
-4.34031029612642));
#53798=CARTESIAN_POINT('Ctrl Pts',(-0.546040215816375,0.506938441893474,
-4.32445278555047));
#53799=CARTESIAN_POINT('Ctrl Pts',(-0.721899881280921,0.18441003921904,
-4.30859527497453));
#53800=CARTESIAN_POINT('Ctrl Pts',(-0.72227208601418,-0.182946808998957,
-4.29273776439859));
#53801=CARTESIAN_POINT('Ctrl Pts',(-0.547066350345486,-0.505830909966805,
-4.27688025382264));
#53802=CARTESIAN_POINT('Ctrl Pts',(-0.23887363523123,-0.705752001449229,
-4.2610227432467));
#53803=CARTESIAN_POINT('Ctrl Pts',(0.127387142739609,-0.734111038619373,
-4.24516523267076));
#53804=CARTESIAN_POINT('Ctrl Pts',(0.46268123573258,-0.584014190974114,
-4.22930772209481));
#53805=CARTESIAN_POINT('Ctrl Pts',(0.685501622478843,-0.291948671408264,
-4.21345021151887));
#53806=CARTESIAN_POINT('Ctrl Pts',(0.741682642499434,0.0710869817423186,
-4.19759270094293));
#53807=CARTESIAN_POINT('Ctrl Pts',(0.617567187931678,0.416842019892833,
-4.18173519036698));
#53808=CARTESIAN_POINT('Ctrl Pts',(0.34332662536585,0.661266458754013,-4.16587767979104));
#53809=CARTESIAN_POINT('Ctrl Pts',(-0.014373595871744,0.744942884320598,
-4.15002016921509));
#53810=CARTESIAN_POINT('Ctrl Pts',(-0.36857972339009,0.647530299417611,
-4.13416265863915));
#53811=CARTESIAN_POINT('Ctrl Pts',(-0.633187388002473,0.392708839769087,
-4.11830514806321));
#53812=CARTESIAN_POINT('Ctrl Pts',(-0.743872812469215,0.0424233429530765,
-4.10244763748726));
#53813=CARTESIAN_POINT('Ctrl Pts',(-0.67372935144614,-0.318174892406895,
-4.08659012691132));
#53814=CARTESIAN_POINT('Ctrl Pts',(-0.439808258411777,-0.601427632380634,
-4.07073261633538));
#53815=CARTESIAN_POINT('Ctrl Pts',(-0.0989736771241871,-0.738478647216488,
-4.05487510575944));
#53816=CARTESIAN_POINT('Ctrl Pts',(0.265920527565673,-0.69601205031046,
-4.03901759518349));
#53817=CARTESIAN_POINT('Ctrl Pts',(0.566171809671833,-0.484351094858986,
-4.02316008460755));
#53818=CARTESIAN_POINT('Ctrl Pts',(0.728791744560353,-0.154948682533456,
-4.00730257403161));
#53819=CARTESIAN_POINT('Ctrl Pts',(0.714248867858033,0.212120380731541,
-3.99144506345566));
#53820=CARTESIAN_POINT('Ctrl Pts',(0.526078423953184,0.527624860112855,
-3.97558755287972));
#53821=CARTESIAN_POINT('Ctrl Pts',(0.210022979428513,0.714868413954726,
-3.95973004230377));
#53822=CARTESIAN_POINT('Ctrl Pts',(-0.157087189318767,0.728333794430896,
-3.94387253172783));
#53823=CARTESIAN_POINT('Ctrl Pts',(-0.486010855087196,0.564747686932481,
-3.92801502115189));
#53824=CARTESIAN_POINT('Ctrl Pts',(-0.696789590985629,0.263876423828005,
-3.91215751057594));
#53825=CARTESIAN_POINT('Ctrl Pts',(-0.738184955094202,-0.101140858364692,
-3.8963));
#53826=CARTESIAN_POINT('Ctrl Pts',(-0.600134101411932,-0.441571694609913,
-3.88044248942406));
#53827=CARTESIAN_POINT('Ctrl Pts',(-0.316195968501739,-0.674660366896873,
-3.86458497884811));
#53828=CARTESIAN_POINT('Ctrl Pts',(0.0446066009386007,-0.743745085570909,
-3.84872746827217));
#53829=CARTESIAN_POINT('Ctrl Pts',(0.394565701175593,-0.632031968031671,
-3.83286995769623));
#53830=CARTESIAN_POINT('Ctrl Pts',(0.648609377700225,-0.366677482697674,
-3.81701244712028));
#53831=CARTESIAN_POINT('Ctrl Pts',(0.744981865115991,-0.0121869523046585,
-3.80115493654434));
#53832=CARTESIAN_POINT('Ctrl Pts',(0.660255866176431,0.345266118143364,
-3.7852974259684));
#53833=CARTESIAN_POINT('Ctrl Pts',(0.415027520037911,0.618788056421063,
-3.76943991539245));
#53834=CARTESIAN_POINT('Ctrl Pts',(0.0689096634373234,0.741888104395219,
-3.75358240481651));
#53835=CARTESIAN_POINT('Ctrl Pts',(-0.293959521387625,0.684641731815797,
-3.73772489424057));
#53836=CARTESIAN_POINT('Ctrl Pts',(-0.585369752826176,0.460965024307049,
-3.72186738366462));
#53837=CARTESIAN_POINT('Ctrl Pts',(-0.734481787276393,0.125231806333102,
-3.70600987308868));
#53838=CARTESIAN_POINT('Ctrl Pts',(-0.705047811199764,-0.240944153447636,
-3.69015236251273));
#53839=CARTESIAN_POINT('Ctrl Pts',(-0.504222963217104,-0.548548725750719,
-3.67429485193679));
#53840=CARTESIAN_POINT('Ctrl Pts',(-0.180825983347723,-0.722805966290058,
-3.65843734136085));
#53841=CARTESIAN_POINT('Ctrl Pts',(0.186528189859359,-0.721355484865796,
-3.64257983078491));
#53842=CARTESIAN_POINT('Ctrl Pts',(0.508539013881873,-0.544549880652111,
-3.62672232020896));
#53843=CARTESIAN_POINT('Ctrl Pts',(0.706928512367425,-0.235369028464147,
-3.61086480963302));
#53844=CARTESIAN_POINT('Ctrl Pts',(0.733469957167495,0.131027947747378,
-3.59500729905708));
#53845=CARTESIAN_POINT('Ctrl Pts',(0.581711358369246,0.465573191563243,
-3.57914978848113));
#53846=CARTESIAN_POINT('Ctrl Pts',(0.288543885839595,0.686941720310219,
-3.56329227790519));
#53847=CARTESIAN_POINT('Ctrl Pts',(-0.0747660470900795,0.741320807316712,
-3.54743476732925));
#53848=CARTESIAN_POINT('Ctrl Pts',(-0.419901016852458,0.615491378659723,
-3.5315772567533));
#53849=CARTESIAN_POINT('Ctrl Pts',(-0.662961772285872,0.340041452834431,
-3.51571974617736));
#53850=CARTESIAN_POINT('Ctrl Pts',(-0.744862398735852,-0.0180695353467789,
-3.49986223560141));
#53851=CARTESIAN_POINT('Ctrl Pts',(-0.645693580048323,-0.371787979690786,
-3.48400472502547));
#53852=CARTESIAN_POINT('Ctrl Pts',(-0.389562376809465,-0.635128062466725,
-3.46814721444952));
#53853=CARTESIAN_POINT('Ctrl Pts',(-0.0387320136518709,-0.744074144340904,
-3.45228970387359));
#53854=CARTESIAN_POINT('Ctrl Pts',(0.321513758624112,-0.672142398732272,
-3.43643219329764));
#53855=CARTESIAN_POINT('Ctrl Pts',(0.603602386739046,-0.436818795247073,
-3.4205746827217));
#53856=CARTESIAN_POINT('Ctrl Pts',(0.738960626213063,-0.0953084154992266,
-3.40471717214575));
#53857=CARTESIAN_POINT('Ctrl Pts',(0.69468408912439,0.26937059504629,-3.38885966156981));
#53858=CARTESIAN_POINT('Ctrl Pts',(0.481536009080821,0.568568002192077,
-3.37300215099387));
#53859=CARTESIAN_POINT('Ctrl Pts',(0.151330794557152,0.729551568963344,
-3.35714464041793));
#53860=CARTESIAN_POINT('Ctrl Pts',(-0.215661594415367,0.713187617568055,
-3.34128712984198));
#53861=CARTESIAN_POINT('Ctrl Pts',(-0.530228561854279,0.523454079506617,
-3.32542961926604));
#53862=CARTESIAN_POINT('Ctrl Pts',(-0.715901666944983,0.206473495692717,
-3.30957210869009));
#53863=CARTESIAN_POINT('Ctrl Pts',(-0.727545424028934,-0.160698964317554,
-3.29371459811415));
#53864=CARTESIAN_POINT('Ctrl Pts',(-0.56232933899328,-0.488806930868986,
-3.27785708753821));
#53865=CARTESIAN_POINT('Ctrl Pts',(-0.260415977294363,-0.698090266318044,
-3.26199957696227));
#53866=CARTESIAN_POINT('Ctrl Pts',(0.104802199620971,-0.737674047335801,
-3.24614206638632));
#53867=CARTESIAN_POINT('Ctrl Pts',(0.4445438909911,-0.597935807709044,-3.23028455581038));
#53868=CARTESIAN_POINT('Ctrl Pts',(0.67622090381438,-0.312844674563337,
-3.21442704523443));
#53869=CARTESIAN_POINT('Ctrl Pts',(0.743514610335906,0.0482962252688744,
-3.19856953465849));
#53870=CARTESIAN_POINT('Ctrl Pts',(0.630066507130376,0.397696740935482,
-3.18271202408254));
#53871=CARTESIAN_POINT('Ctrl Pts',(0.363454822249294,0.650420704884086,
-3.16685451350661));
#53872=CARTESIAN_POINT('Ctrl Pts',(0.00849049249189266,0.745033162144761,
-3.15099700293066));
#53873=CARTESIAN_POINT('Ctrl Pts',(-0.348537800713067,0.65853466319722,
-3.13513949235472));
#53874=CARTESIAN_POINT('Ctrl Pts',(-0.620839644721946,0.411952226234673,
-3.11928198177877));
#53875=CARTESIAN_POINT('Ctrl Pts',(-0.742220875500842,0.0652278554678893,
-3.10342447120283));
#53876=CARTESIAN_POINT('Ctrl Pts',(-0.683174792020755,-0.297352828649017,
-3.08756696062688));
#53877=CARTESIAN_POINT('Ctrl Pts',(-0.458054973669544,-0.587649676469553,
-3.07170945005094));
#53878=CARTESIAN_POINT('Ctrl Pts',(-0.121586052362424,-0.735094098077993,
-3.055851939475));
#53879=CARTESIAN_POINT('Ctrl Pts',(0.244439360284691,-0.703843661832503,
-3.03999442889905));
#53880=CARTESIAN_POINT('Ctrl Pts',(0.551043731660782,-0.5014950717161,-3.02413691832311));
#53881=CARTESIAN_POINT('Ctrl Pts',(0.723694257457264,-0.177237475951216,
-3.00827940774717));
#53882=CARTESIAN_POINT('Ctrl Pts',(0.720421125583033,0.190104978819204,
-2.99242189717122));
#53883=CARTESIAN_POINT('Ctrl Pts',(0.542020005376938,0.511234598720941,
-2.97656438659528));
#53884=CARTESIAN_POINT('Ctrl Pts',(0.23185862744593,0.708087620310554,-2.96070687601934));
#53885=CARTESIAN_POINT('Ctrl Pts',(-0.134665527144535,0.732810819350438,
-2.9448493654434));
#53886=CARTESIAN_POINT('Ctrl Pts',(-0.468453686038892,0.579394205351375,
-2.92899185486745));
#53887=CARTESIAN_POINT('Ctrl Pts',(-0.688364907195973,0.285131996975536,
-2.91313434429151));
#53888=CARTESIAN_POINT('Ctrl Pts',(-0.740940722498702,-0.0784432718674888,
-2.89727683371556));
#53889=CARTESIAN_POINT('Ctrl Pts',(-0.613400417387355,-0.42294967680233,
-2.88141932313962));
#53890=CARTESIAN_POINT('Ctrl Pts',(-0.336747909254422,-0.664640765203995,
-2.86556181256368));
#53891=CARTESIAN_POINT('Ctrl Pts',(0.0217650299908832,-0.744763576329879,
-2.84970430198774));
#53892=CARTESIAN_POINT('Ctrl Pts',(0.374987083415478,-0.643840965168983,
-2.83384679141179));
#53893=CARTESIAN_POINT('Ctrl Pts',(0.637053101519986,-0.386406323708533,
-2.81798928083585));
#53894=CARTESIAN_POINT('Ctrl Pts',(0.744257158796397,-0.0350397308564244,
-2.80213177025991));
#53895=CARTESIAN_POINT('Ctrl Pts',(0.670538899398487,0.324844709902505,
-2.78627425968396));
#53896=CARTESIAN_POINT('Ctrl Pts',(0.43381857859533,0.605762281777021,-2.77041674910802));
#53897=CARTESIAN_POINT('Ctrl Pts',(0.0916408075974612,0.739424413676653,
-2.75455923853207));
#53898=CARTESIAN_POINT('Ctrl Pts',(-0.272814031234396,0.693339026393159,
-2.73870172795613));
#53899=CARTESIAN_POINT('Ctrl Pts',(-0.570950197858908,0.478709068979323,
-2.72284421738019));
#53900=CARTESIAN_POINT('Ctrl Pts',(-0.730293433462981,0.147709181160235,
-2.70698670680424));
#53901=CARTESIAN_POINT('Ctrl Pts',(-0.71210881021805,-0.219197499000354,
-2.6911291962283));
#53902=CARTESIAN_POINT('Ctrl Pts',(-0.520816848808986,-0.532819210572265,
-2.67527168565235));
#53903=CARTESIAN_POINT('Ctrl Pts',(-0.202918929048214,-0.716917296061479,
-2.65941417507642));
#53904=CARTESIAN_POINT('Ctrl Pts',(0.164306783272657,-0.726739143110351,
-2.64355666450047));
#53905=CARTESIAN_POINT('Ctrl Pts',(0.491590973333846,-0.559897147782392,
-2.62769915392453));
#53906=CARTESIAN_POINT('Ctrl Pts',(0.699373756252946,-0.256949119910581,
-2.61184164334858));
#53907=CARTESIAN_POINT('Ctrl Pts',(0.737144979717066,0.10846096088502,-2.59598413277264));
#53908=CARTESIAN_POINT('Ctrl Pts',(0.595722794184041,0.447505143710925,
-2.5801266221967));
#53909=CARTESIAN_POINT('Ctrl Pts',(0.309485679099278,0.677764793708433,
-2.56426911162075));
#53910=CARTESIAN_POINT('Ctrl Pts',(-0.0519846606557266,0.743265831459165,
-2.54841160104481));
#53911=CARTESIAN_POINT('Ctrl Pts',(-0.400817990304477,0.628085535422093,
-2.53255409046887));
#53912=CARTESIAN_POINT('Ctrl Pts',(-0.65221602018681,0.360223214368335,
-2.51669657989292));
#53913=CARTESIAN_POINT('Ctrl Pts',(-0.745066118148496,0.00479382366248841,
-2.50083906931698));
#53914=CARTESIAN_POINT('Ctrl Pts',(-0.656797248589648,-0.351800903073378,
-2.48498155874103));
#53915=CARTESIAN_POINT('Ctrl Pts',(-0.408866791102873,-0.622875949360237,
-2.4691240481651));
#53916=CARTESIAN_POINT('Ctrl Pts',(-0.0615444417367415,-0.742535374813543,
-2.45326653758914));
#53917=CARTESIAN_POINT('Ctrl Pts',(0.30073881575884,-0.681691034013317,
-2.43740902701321));
#53918=CARTESIAN_POINT('Ctrl Pts',(0.589915133512018,-0.455133646758482,
-2.42155151643726));
#53919=CARTESIAN_POINT('Ctrl Pts',(0.735688312531754,-0.117937305219158,
-2.40569400586132));
#53920=CARTESIAN_POINT('Ctrl Pts',(0.702622185432192,0.247928549579643,
-2.38983649528537));
#53921=CARTESIAN_POINT('Ctrl Pts',(0.498754834544953,0.553525172125181,
-2.37397898470943));
#53922=CARTESIAN_POINT('Ctrl Pts',(0.173644605370432,0.72456473291482,-2.35812147413349));
#53923=CARTESIAN_POINT('Ctrl Pts',(-0.193677087826048,0.719469031167705,
-2.34226396355754));
#53924=CARTESIAN_POINT('Ctrl Pts',(-0.513917598124815,0.539476786799764,
-2.3264064529816));
#53925=CARTESIAN_POINT('Ctrl Pts',(-0.709229296744016,0.228342518594689,
-2.31054894240566));
#53926=CARTESIAN_POINT('Ctrl Pts',(-0.732133641394678,-0.138299791382143,
-2.29469143182972));
#53927=CARTESIAN_POINT('Ctrl Pts',(-0.577062788963539,-0.471322648248307,
-2.27883392125377));
#53928=CARTESIAN_POINT('Ctrl Pts',(-0.28171308880903,-0.689771148100477,
-2.26297641067783));
#53929=CARTESIAN_POINT('Ctrl Pts',(0.0821185655496305,-0.740542397402233,
-2.24711890010188));
#53930=CARTESIAN_POINT('Ctrl Pts',(0.425987924691361,-0.611294355589289,
-2.23126138952594));
#53931=CARTESIAN_POINT('Ctrl Pts',(0.66630339617538,-0.333446075705398,
-2.21540387895));
#53932=CARTESIAN_POINT('Ctrl Pts',(0.744646419535463,0.025459988829357,
-2.19954636837405));
#53933=CARTESIAN_POINT('Ctrl Pts',(0.641972500386766,0.3781769558095,-2.18368885779811));
#53934=CARTESIAN_POINT('Ctrl Pts',(0.383240758161146,0.638962457772165,
-2.16783134722217));
#53935=CARTESIAN_POINT('Ctrl Pts',(0.0313465854623456,0.744421851330298,
-2.15197383664622));
#53936=CARTESIAN_POINT('Ctrl Pts',(-0.328167664241619,0.668918892919293,
-2.13611632607028));
#53937=CARTESIAN_POINT('Ctrl Pts',(-0.607907264322853,0.430807682315068,
-2.12025881549434));
#53938=CARTESIAN_POINT('Ctrl Pts',(-0.739869998189859,0.0879709437070718,
-2.10440130491839));
#53939=CARTESIAN_POINT('Ctrl Pts',(-0.691976895229164,-0.276250751360397,
-2.08854379434245));
#53940=CARTESIAN_POINT('Ctrl Pts',(-0.475870344147353,-0.573318338028059,
-2.0726862837665));
#53941=CARTESIAN_POINT('Ctrl Pts',(-0.144083931498636,-0.731017319796236,
-2.05682877319056));
#53942=CARTESIAN_POINT('Ctrl Pts',(0.222728007440529,-0.711012472365815,
-2.04097126261462));
#53943=CARTESIAN_POINT('Ctrl Pts',(0.535396742490916,-0.51816679678294,
-2.02511375203868));
#53944=CARTESIAN_POINT('Ctrl Pts',(0.717915276301731,-0.199359367000361,
-2.00925624146273));
#53945=CARTESIAN_POINT('Ctrl Pts',(0.725914971523952,0.167910557367775,
-1.99339873088679));
#53946=CARTESIAN_POINT('Ctrl Pts',(0.557451173174836,0.494362913944983,
-1.97754122031085));
#53947=CARTESIAN_POINT('Ctrl Pts',(0.253475937022809,0.700640029193726,
-1.9616837097349));
#53948=CARTESIAN_POINT('Ctrl Pts',(-0.112117052086442,0.736597765262441,
-1.94582619915896));
#53949=CARTESIAN_POINT('Ctrl Pts',(-0.450455379870058,0.593495115316291,
-1.92996868858302));
#53950=CARTESIAN_POINT('Ctrl Pts',(-0.679291998571966,0.306119064800417,
-1.91411117800707));
#53951=CARTESIAN_POINT('Ctrl Pts',(-0.74299875506506,-0.0556718162982561,
-1.89825366743113));
#53952=CARTESIAN_POINT('Ctrl Pts',(-0.626089101673838,-0.40392937244452,
-1.88239615685519));
#53953=CARTESIAN_POINT('Ctrl Pts',(-0.356982738609634,-0.653995279411816,
-1.86653864627924));
#53954=CARTESIAN_POINT('Ctrl Pts',(-0.00109703682003259,-0.745080732315894,
-1.8506811357033));
#53955=CARTESIAN_POINT('Ctrl Pts',(0.355055344894126,-0.655043665124921,
-1.83482362512736));
#53956=CARTESIAN_POINT('Ctrl Pts',(0.624896920206737,-0.405771290598917,
-1.81896611455141));
#53957=CARTESIAN_POINT('Ctrl Pts',(0.742831594591062,-0.0578595129211745,
-1.80310860397547));
#53958=CARTESIAN_POINT('Ctrl Pts',(0.680190494320244,0.304117399361759,
-1.78725109339952));
#53959=CARTESIAN_POINT('Ctrl Pts',(0.452201115490324,0.592166068183142,
-1.77139358282358));
#53960=CARTESIAN_POINT('Ctrl Pts',(0.114285654727207,0.73626441600946,-1.75553607224764));
#53961=CARTESIAN_POINT('Ctrl Pts',(-0.251411635436553,0.701383412068814,
-1.73967856167169));
#53962=CARTESIAN_POINT('Ctrl Pts',(-0.555992986056486,0.496002319162088,
-1.72382105109575));
#53963=CARTESIAN_POINT('Ctrl Pts',(-0.7254173712336,0.170047460053681,-1.70796354051981));
#53964=CARTESIAN_POINT('Ctrl Pts',(-0.718499225058212,-0.197244428942686,
-1.69210602994386));
#53965=CARTESIAN_POINT('Ctrl Pts',(-0.53692028752885,-0.51658794604415,
-1.67624851936792));
#53966=CARTESIAN_POINT('Ctrl Pts',(-0.224820788469039,-0.710353513562321,
-1.66039100879198));
#53967=CARTESIAN_POINT('Ctrl Pts',(0.141930650992857,-0.731438439970802,
-1.64453349821603));
#53968=CARTESIAN_POINT('Ctrl Pts',(0.474180007564145,-0.574717166599923,
-1.62867598764009));
#53969=CARTESIAN_POINT('Ctrl Pts',(0.691160408405278,-0.278287245505838,
-1.61281847706415));
#53970=CARTESIAN_POINT('Ctrl Pts',(0.740125841833161,0.0857918376591303,
-1.59696096648821));
#53971=CARTESIAN_POINT('Ctrl Pts',(0.609173245111979,0.429015685724797,
-1.58110345591226));
#53972=CARTESIAN_POINT('Ctrl Pts',(0.330136033470989,0.667949624269838,
-1.56524594533632));
#53973=CARTESIAN_POINT('Ctrl Pts',(-0.0291543209007144,0.744510931236738,
-1.54938843476037));
#53974=CARTESIAN_POINT('Ctrl Pts',(-0.38135751834543,0.640088231699029,
-1.53353092418443));
#53975=CARTESIAN_POINT('Ctrl Pts',(-0.640856084219246,0.380065758096348,
-1.51767341360849));
#53976=CARTESIAN_POINT('Ctrl Pts',(-0.744568217888247,0.0276526683864981,
-1.50181590303254));
#53977=CARTESIAN_POINT('Ctrl Pts',(-0.667282419175575,-0.331482539837873,
-1.4859583924566));
#53978=CARTESIAN_POINT('Ctrl Pts',(-0.4277861805277,-0.610037281571953,
-1.47010088188066));
#53979=CARTESIAN_POINT('Ctrl Pts',(-0.0842989141717446,-0.74029736878341,
-1.45424337130471));
#53980=CARTESIAN_POINT('Ctrl Pts',(0.27968067082008,-0.690597729164966,
-1.43838586072877));
#53981=CARTESIAN_POINT('Ctrl Pts',(0.575672364401323,-0.473019904467842,
-1.42252835015283));
#53982=CARTESIAN_POINT('Ctrl Pts',(0.731723210142681,-0.140455134817732,
-1.40667083957688));
#53983=CARTESIAN_POINT('Ctrl Pts',(0.709898631000685,0.226253032822831,
-1.39081332900094));
#53984=CARTESIAN_POINT('Ctrl Pts',(0.515503988666716,0.537961094157267,
-1.37495581842499));
#53985=CARTESIAN_POINT('Ctrl Pts',(0.195794897177476,0.718895583097738,
-1.35909830784905));
#53986=CARTESIAN_POINT('Ctrl Pts',(-0.17151019788618,0.725072929558965,
-1.34324079727311));
#53987=CARTESIAN_POINT('Ctrl Pts',(-0.497122684463518,0.554991475384949,
-1.32738328669717));
#53988=CARTESIAN_POINT('Ctrl Pts',(-0.701889053967625,0.249996514132912,
-1.31152577612122));
#53989=CARTESIAN_POINT('Ctrl Pts',(-0.736032417443101,-0.115770383220588,
-1.29566826554528));
#53990=CARTESIAN_POINT('Ctrl Pts',(-0.591252825946184,-0.453394526840398,
-1.27981075496934));
#53991=CARTESIAN_POINT('Ctrl Pts',(-0.302744914545142,-0.680802480808663,
-1.26395324439339));
#53992=CARTESIAN_POINT('Ctrl Pts',(0.0593576014270612,-0.742713387728404,
-1.24809573381745));
#53993=CARTESIAN_POINT('Ctrl Pts',(0.407030810760431,-0.624077255033285,
-1.2322382232415));
#53994=CARTESIAN_POINT('Ctrl Pts',(0.655758438757783,-0.353733474746353,
-1.21638071266556));
#53995=CARTESIAN_POINT('Ctrl Pts',(0.745077004287191,0.00259977702898679,
-1.20052320208962));
#53996=CARTESIAN_POINT('Ctrl Pts',(0.653273955972268,0.358301046058368,
-1.18466569151367));
#53997=CARTESIAN_POINT('Ctrl Pts',(0.402665800926975,0.626902507509751,
-1.16880818093773));
#53998=CARTESIAN_POINT('Ctrl Pts',(0.0541731597357335,0.743109527541145,
-1.15295067036179));
#53999=CARTESIAN_POINT('Ctrl Pts',(-0.307488496284748,0.678673209881398,
-1.13709315978584));
#54000=CARTESIAN_POINT('Ctrl Pts',(-0.594402425070052,0.449257452057301,
-1.1212356492099));
#54001=CARTESIAN_POINT('Ctrl Pts',(-0.736822394328756,0.110631190781873,
-1.10537813863396));
#54002=CARTESIAN_POINT('Ctrl Pts',(-0.700127372238149,-0.254888532109785,
-1.08952062805801));
#54003=CARTESIAN_POINT('Ctrl Pts',(-0.493237593328167,-0.558447112702729,
-1.07366311748207));
#54004=CARTESIAN_POINT('Ctrl Pts',(-0.166446128554507,-0.72625215142359,
-1.05780560690613));
#54005=CARTESIAN_POINT('Ctrl Pts',(0.200806914349289,-0.717511731128971,
-1.04194809633018));
#54006=CARTESIAN_POINT('Ctrl Pts',(0.519245576741049,-0.534350570499398,
-1.02609058575424));
#54007=CARTESIAN_POINT('Ctrl Pts',(0.711460243089813,-0.221293523765969,
-1.0102330751783));
#54008=CARTESIAN_POINT('Ctrl Pts',(0.730725232193086,0.145558016593173,
-0.994375564602353));
#54009=CARTESIAN_POINT('Ctrl Pts',(0.572357396004417,0.477025693644712,
-0.978518054026409));
#54010=CARTESIAN_POINT('Ctrl Pts',(0.274854551402442,0.692532653909937,
-0.962660543450467));
#54011=CARTESIAN_POINT('Ctrl Pts',(-0.0894629977683567,0.73969106604614,
-0.946803032874522));
#54012=CARTESIAN_POINT('Ctrl Pts',(-0.432032885366019,0.607037138172358,
-0.930945522298579));
#54013=CARTESIAN_POINT('Ctrl Pts',(-0.669579408960958,0.326817864036942,
-0.915088011722637));
#54014=CARTESIAN_POINT('Ctrl Pts',(-0.744357114769118,-0.0328479352588572,
-0.899230501146692));
#54015=CARTESIAN_POINT('Ctrl Pts',(-0.638188205492206,-0.384528692725023,
-0.88337299057075));
#54016=CARTESIAN_POINT('Ctrl Pts',(-0.376881401675451,-0.64273393424443,
-0.867515479994806));
#54017=CARTESIAN_POINT('Ctrl Pts',(-0.0239580705647442,-0.744696254867037,
-0.851657969418863));
#54018=CARTESIAN_POINT('Ctrl Pts',(0.334789255086544,-0.665629518453601,
-0.835800458842918));
#54019=CARTESIAN_POINT('Ctrl Pts',(0.612152281088124,-0.424754147615751,
-0.819942948266977));
#54020=CARTESIAN_POINT('Ctrl Pts',(0.740706514936408,-0.0806248093885304,
-0.804085437691032));
#54021=CARTESIAN_POINT('Ctrl Pts',(0.68920156215251,0.283103705176595,-0.788227927115088));
#54022=CARTESIAN_POINT('Ctrl Pts',(0.470157820112161,0.5780122190279,-0.772370416539146));
#54023=CARTESIAN_POINT('Ctrl Pts',(0.136822880450277,0.732411087124892,
-0.756512905963202));
#54024=CARTESIAN_POINT('Ctrl Pts',(-0.229772488369119,0.708767313542914,
-0.740655395387258));
#54025=CARTESIAN_POINT('Ctrl Pts',(-0.54051220244279,0.512828490012617,
-0.724797884811315));
#54026=CARTESIAN_POINT('Ctrl Pts',(-0.719858192316569,0.192225607328728,
-0.708940374235372));
#54027=CARTESIAN_POINT('Ctrl Pts',(-0.724213037944555,-0.175105616212887,
-0.693082863659428));
#54028=CARTESIAN_POINT('Ctrl Pts',(-0.552518114964911,-0.499870216950158,
-0.677225353083484));
#54029=CARTESIAN_POINT('Ctrl Pts',(-0.246510936896401,-0.703120799826482,
-0.661367842507542));
#54030=CARTESIAN_POINT('Ctrl Pts',(0.119420864350713,-0.735448950176627,
-0.645510331931598));
#54031=CARTESIAN_POINT('Ctrl Pts',(0.456322512266791,-0.588995981273811,
-0.629652821355655));
#54032=CARTESIAN_POINT('Ctrl Pts',(0.682296203233876,-0.299363311397401,
-0.613795310779712));
#54033=CARTESIAN_POINT('Ctrl Pts',(0.742409736474291,0.0630419253064556,
-0.597937800203768));
#54034=CARTESIAN_POINT('Ctrl Pts',(0.622050045027544,0.41012222890184,-0.582080289627824));
#54035=CARTESIAN_POINT('Ctrl Pts',(0.350475502767979,0.657505454819733,
-0.566222779051882));
#54036=CARTESIAN_POINT('Ctrl Pts',(-0.00629652687738437,0.745054934154154,
-0.550365268475936));
#54037=CARTESIAN_POINT('Ctrl Pts',(-0.361537926664331,0.651488164697928,
-0.534507757899994));
#54038=CARTESIAN_POINT('Ctrl Pts',(-0.628892661896185,0.39955039853715,
-0.51865024732405));
#54039=CARTESIAN_POINT('Ctrl Pts',(-0.743369166821858,0.0504854729301265,
-0.502792736748107));
#54040=CARTESIAN_POINT('Ctrl Pts',(-0.677139218048598,-0.310852023539114,
-0.486935226172163));
#54041=CARTESIAN_POINT('Ctrl Pts',(-0.446302728926307,-0.596624149118552,
-0.47107771559622));
#54042=CARTESIAN_POINT('Ctrl Pts',(-0.10697400334667,-0.737362233753777,
-0.455220205020277));
#54043=CARTESIAN_POINT('Ctrl Pts',(0.258359154003842,-0.698854096860472,
-0.439362694444332));
#54044=CARTESIAN_POINT('Ctrl Pts',(0.560887491653129,-0.490460725105599,
-0.42350518386839));
#54045=CARTESIAN_POINT('Ctrl Pts',(0.727069052926082,-0.162840699527328,
-0.407647673292446));
#54046=CARTESIAN_POINT('Ctrl Pts',(0.716506573706083,0.204364456341259,
-0.391790162716503));
#54047=CARTESIAN_POINT('Ctrl Pts',(0.531767698940294,0.521890424799043,
-0.375932652140559));
#54048=CARTESIAN_POINT('Ctrl Pts',(0.217760811380721,0.712549458064953,
-0.360075141564617));
#54049=CARTESIAN_POINT('Ctrl Pts',(-0.149181799006659,0.729994035651059,
-0.344217630988673));
#54050=CARTESIAN_POINT('Ctrl Pts',(-0.479859636199047,0.569983535206768,
-0.328360120412729));
#54051=CARTESIAN_POINT('Ctrl Pts',(-0.693887851295182,0.27141509112605,
-0.312502609836787));
#54052=CARTESIAN_POINT('Ctrl Pts',(-0.73923807984108,-0.0931319557401305,
-0.296645099260842));
#54053=CARTESIAN_POINT('Ctrl Pts',(-0.604886089121433,-0.435039448872488,
-0.280787588684899));
#54054=CARTESIAN_POINT('Ctrl Pts',(-0.323491645640655,-0.671192711037537,
-0.264930078108956));
#54055=CARTESIAN_POINT('Ctrl Pts',(0.0365407342377404,-0.74418497214044,
-0.249072567533012));
#54056=CARTESIAN_POINT('Ctrl Pts',(0.387690414045755,-0.636272472016097,
-0.233215056957068));
#54057=CARTESIAN_POINT('Ctrl Pts',(0.64459593589752,-0.373687760499387,
-0.217357546381126));
#54058=CARTESIAN_POINT('Ctrl Pts',(0.744806009371733,-0.0202628962177233,
-0.201500035805182));
#54059=CARTESIAN_POINT('Ctrl Pts',(0.663960133248361,0.338087754507852,
-0.185642525229238));
#54060=CARTESIAN_POINT('Ctrl Pts',(0.421711850082436,0.614252160152718,
-0.169785014653295));
#54061=CARTESIAN_POINT('Ctrl Pts',(0.0769483449333087,0.741097525544364,
-0.153927504077352));
#54062=CARTESIAN_POINT('Ctrl Pts',(-0.286519037709493,0.687788235191209,
-0.138069993501407));
#54063=CARTESIAN_POINT('Ctrl Pts',(-0.580339275444648,0.46728453937117,
-0.122212482925465));
#54064=CARTESIAN_POINT('Ctrl Pts',(-0.733078137321275,0.133186519459017,
-0.106354972349522));
#54065=CARTESIAN_POINT('Ctrl Pts',(-0.707624014265837,-0.233284843518718,
-0.0904974617735782));
#54066=CARTESIAN_POINT('Ctrl Pts',(-0.510129659904911,-0.543052839296335,
-0.0746399511976345));
#54067=CARTESIAN_POINT('Ctrl Pts',(-0.188672782786423,-0.720797397637529,
-0.058782440621692));
#54068=CARTESIAN_POINT('Ctrl Pts',(0.178741094754426,-0.723347949753151,
-0.0429249300457477));
#54069=CARTESIAN_POINT('Ctrl Pts',(0.394571264335502,-0.607775493600903,
-0.0323532563284519));
#54070=CARTESIAN_POINT('Ctrl Pts',(0.482201081976437,-0.527701441143757,
-0.0270674194698041));
#54071=CARTESIAN_POINT('Ctrl Pts',(0.392888236737257,-0.550964357679777,
-5.8089));
#54072=CARTESIAN_POINT('Ctrl Pts',(0.484381081792765,-0.485721548291323,
-5.80361416314135));
#54073=CARTESIAN_POINT('Ctrl Pts',(0.634146933675295,-0.308844853941977,
-5.79304248942406));
#54074=CARTESIAN_POINT('Ctrl Pts',(0.70461890056211,0.0317634872067408,
-5.77718497884811));
#54075=CARTESIAN_POINT('Ctrl Pts',(0.603809517943593,0.364559903875637,
-5.76132746827217));
#54076=CARTESIAN_POINT('Ctrl Pts',(0.356217202446025,0.608779534529828,
-5.74546995769622));
#54077=CARTESIAN_POINT('Ctrl Pts',(0.0220327184609351,0.704987657002684,
-5.72961244712028));
#54078=CARTESIAN_POINT('Ctrl Pts',(-0.317508269912238,0.629831081602948,
-5.71375493654434));
#54079=CARTESIAN_POINT('Ctrl Pts',(-0.5798655339509,0.401562243999013,-5.6978974259684));
#54080=CARTESIAN_POINT('Ctrl Pts',(-0.701262770546561,0.0756802099782287,
-5.68203991539245));
#54081=CARTESIAN_POINT('Ctrl Pts',(-0.652189172010462,-0.268600560210128,
-5.66618240481651));
#54082=CARTESIAN_POINT('Ctrl Pts',(-0.444574205494435,-0.547586123312261,
-5.65032489424056));
#54083=CARTESIAN_POINT('Ctrl Pts',(-0.128887172109694,-0.69345876028638,
-5.63446738366463));
#54084=CARTESIAN_POINT('Ctrl Pts',(0.218131180300111,-0.670757513336377,
-5.61860987308867));
#54085=CARTESIAN_POINT('Ctrl Pts',(0.512123781755499,-0.485001168094135,
-5.60275236251274));
#54086=CARTESIAN_POINT('Ctrl Pts',(0.681623629821306,-0.181345284572452,
-5.58689485193679));
#54087=CARTESIAN_POINT('Ctrl Pts',(0.685426818106913,0.166394001985959,
-5.57103734136085));
#54088=CARTESIAN_POINT('Ctrl Pts',(0.522608823274475,0.47368439616164,-5.5551798307849));
#54089=CARTESIAN_POINT('Ctrl Pts',(0.232749257329435,0.665826306056506,
-5.53932232020896));
#54090=CARTESIAN_POINT('Ctrl Pts',(-0.113689589679385,0.69611174793571,
-5.52346480963302));
#54091=CARTESIAN_POINT('Ctrl Pts',(-0.432491505325853,0.557178593751515,
-5.50760729905708));
#54092=CARTESIAN_POINT('Ctrl Pts',(-0.646158570569616,0.28280026438264,
-5.49174978848113));
#54093=CARTESIAN_POINT('Ctrl Pts',(-0.70275021616536,-0.0603243024334685,
-5.47589227790519));
#54094=CARTESIAN_POINT('Ctrl Pts',(-0.588509514849396,-0.388784565910968,
-5.46003476732924));
#54095=CARTESIAN_POINT('Ctrl Pts',(-0.331207368228394,-0.622734748534038,
-5.4441772567533));
#54096=CARTESIAN_POINT('Ctrl Pts',(0.00660835310116418,-0.705303634925465,
-5.42831974617736));
#54097=CARTESIAN_POINT('Ctrl Pts',(0.342817642383509,-0.616419460965605,
-5.41246223560141));
#54098=CARTESIAN_POINT('Ctrl Pts',(0.595691002243588,-0.377689181239748,
-5.39660472502547));
#54099=CARTESIAN_POINT('Ctrl Pts',(0.703757160891212,-0.0471460101786735,
-5.38074721444953));
#54100=CARTESIAN_POINT('Ctrl Pts',(0.64074619327961,0.294857937962055,-5.36488970387358));
#54101=CARTESIAN_POINT('Ctrl Pts',(0.421975506976434,0.565184535610204,
-5.34903219329764));
#54102=CARTESIAN_POINT('Ctrl Pts',(0.100626316187652,0.698119783613068,
-5.3331746827217));
#54103=CARTESIAN_POINT('Ctrl Pts',(-0.245184239907299,0.661348301791295,
-5.31731717214575));
#54104=CARTESIAN_POINT('Ctrl Pts',(-0.531392681099133,0.463808911358507,
-5.30145966156981));
#54105=CARTESIAN_POINT('Ctrl Pts',(-0.688424272875483,0.153521686732225,
-5.28560215099387));
#54106=CARTESIAN_POINT('Ctrl Pts',(-0.678106027527137,-0.194085298805999,
-5.26974464041792));
#54107=CARTESIAN_POINT('Ctrl Pts',(-0.502946219016085,-0.49451186897655,
-5.25388712984198));
#54108=CARTESIAN_POINT('Ctrl Pts',(-0.205524643813888,-0.674726988171084,
-5.23802961926603));
#54109=CARTESIAN_POINT('Ctrl Pts',(0.141858150105515,-0.690921958711615,
-5.2221721086901));
#54110=CARTESIAN_POINT('Ctrl Pts',(0.454756485457226,-0.539159926845312,
-5.20631459811414));
#54111=CARTESIAN_POINT('Ctrl Pts',(0.65710755109285,-0.256332896987509,
-5.19045708753821));
#54112=CARTESIAN_POINT('Ctrl Pts',(0.699721597013181,0.0888063874649557,
-5.17459957696226));
#54113=CARTESIAN_POINT('Ctrl Pts',(0.572239526473699,0.412357626487503,
-5.15874206638632));
#54114=CARTESIAN_POINT('Ctrl Pts',(0.30565110055879,0.635668382498652,-5.14288455581037));
#54115=CARTESIAN_POINT('Ctrl Pts',(-0.035238397980778,0.704453790598787,
-5.12702704523444));
#54116=CARTESIAN_POINT('Ctrl Pts',(-0.367561754396992,0.601992727934364,
-5.11116953465848));
#54117=CARTESIAN_POINT('Ctrl Pts',(-0.610534107144088,0.353192570413113,
-5.09531202408255));
#54118=CARTESIAN_POINT('Ctrl Pts',(-0.705091031476859,0.0185344304511741,
-5.0794545135066));
#54119=CARTESIAN_POINT('Ctrl Pts',(-0.628246577437432,-0.320629265226061,
-5.06359700293066));
#54120=CARTESIAN_POINT('Ctrl Pts',(-0.398680950495202,-0.581850829245344,
-5.04773949235472));
#54121=CARTESIAN_POINT('Ctrl Pts',(-0.0721995192170595,-0.701629615399804,
-5.03188198177877));
#54122=CARTESIAN_POINT('Ctrl Pts',(0.271832975057436,-0.650848462741271,
-5.01602447120283));
#54123=CARTESIAN_POINT('Ctrl Pts',(0.549785283183103,-0.441851819252255,
-5.00016696062688));
#54124=CARTESIAN_POINT('Ctrl Pts',(0.694089663396602,-0.125444915988027,
-4.98430945005094));
#54125=CARTESIAN_POINT('Ctrl Pts',(0.669667000279414,0.221456534150661,
-4.968451939475));
#54126=CARTESIAN_POINT('Ctrl Pts',(0.482454226702515,0.514523864284379,
-4.95259442889905));
#54127=CARTESIAN_POINT('Ctrl Pts',(0.177961108082654,0.682515004810329,
-4.93673691832311));
#54128=CARTESIAN_POINT('Ctrl Pts',(-0.169792778098127,0.684592798886295,
-4.92087940774717));
#54129=CARTESIAN_POINT('Ctrl Pts',(-0.476271545316318,0.520252153194254,
-4.90502189717122));
#54130=CARTESIAN_POINT('Ctrl Pts',(-0.666972922520502,0.229442821647816,
-4.88916438659529));
#54131=CARTESIAN_POINT('Ctrl Pts',(-0.695539095682312,-0.117142025587244,
-4.87330687601934));
#54132=CARTESIAN_POINT('Ctrl Pts',(-0.555025881375534,-0.435250684990344,
-4.85744936544339));
#54133=CARTESIAN_POINT('Ctrl Pts',(-0.279590796199469,-0.647553761831247,
-4.84159185486746));
#54134=CARTESIAN_POINT('Ctrl Pts',(0.0638103326637412,-0.702442260421875,
-4.8257343442915));
#54135=CARTESIAN_POINT('Ctrl Pts',(0.391699735402671,-0.586573273399606,
-4.80987683371557));
#54136=CARTESIAN_POINT('Ctrl Pts',(0.624370405298808,-0.32811352420809,
-4.79401932313962));
#54137=CARTESIAN_POINT('Ctrl Pts',(0.705262165372666,0.0101077136440157,
-4.77816181256367));
#54138=CARTESIAN_POINT('Ctrl Pts',(0.614710945941539,0.345871855924866,
-4.76230430198774));
#54139=CARTESIAN_POINT('Ctrl Pts',(0.374728945616527,0.597557616551221,
-4.74644679141179));
#54140=CARTESIAN_POINT('Ctrl Pts',(0.0436536609816854,0.703982418576024,
-4.73058928083585));
#54141=CARTESIAN_POINT('Ctrl Pts',(-0.298033441601801,0.639275336195787,
-4.71473177025991));
#54142=CARTESIAN_POINT('Ctrl Pts',(-0.567271256914447,0.419166087440235,
-4.69887425968396));
#54143=CARTESIAN_POINT('Ctrl Pts',(-0.69861045913254,0.0971612791798993,
-4.68301674910802));
#54144=CARTESIAN_POINT('Ctrl Pts',(-0.660123652658186,-0.248462574611278,
-4.66715923853208));
#54145=CARTESIAN_POINT('Ctrl Pts',(-0.461166638918949,-0.533687379398699,
-4.65130172795613));
#54146=CARTESIAN_POINT('Ctrl Pts',(-0.15010410398989,-0.689177513958953,
-4.63544421738019));
#54147=CARTESIAN_POINT('Ctrl Pts',(0.197447407787028,-0.677134705165401,
-4.61958670680424));
#54148=CARTESIAN_POINT('Ctrl Pts',(0.497001205311606,-0.500486453063479,
-4.6037291962283));
#54149=CARTESIAN_POINT('Ctrl Pts',(0.675738416267745,-0.202174381565054,
-4.58787168565236));
#54150=CARTESIAN_POINT('Ctrl Pts',(0.690209609366951,0.145284489601514,
-4.57201417507641));
#54151=CARTESIAN_POINT('Ctrl Pts',(0.536896965869284,0.457425989447045,
-4.55615666450047));
#54152=CARTESIAN_POINT('Ctrl Pts',(0.253069430129838,0.658371286824547,
-4.54029915392453));
#54153=CARTESIAN_POINT('Ctrl Pts',(-0.0922770403452622,0.699272361534738,
-4.52444164334858));
#54154=CARTESIAN_POINT('Ctrl Pts',(-0.415191780446262,0.570186524946981,
-4.50858413277264));
#54155=CARTESIAN_POINT('Ctrl Pts',(-0.637177079836271,0.302493399452904,
-4.49272662219669));
#54156=CARTESIAN_POINT('Ctrl Pts',(-0.704270280368694,-0.0387331895233606,
-4.47686911162076));
#54157=CARTESIAN_POINT('Ctrl Pts',(-0.600161619846482,-0.370544083537301,
-4.46101160104481));
#54158=CARTESIAN_POINT('Ctrl Pts',(-0.350158990608888,-0.61227899610963,
-4.44515409046887));
#54159=CARTESIAN_POINT('Ctrl Pts',(-0.0150358152851096,-0.705174313230397,
-4.42929657989292));
#54160=CARTESIAN_POINT('Ctrl Pts',(0.32374243342603,-0.626648006923061,
-4.41343906931699));
#54161=CARTESIAN_POINT('Ctrl Pts',(0.583821766891339,-0.39578912603194,
-4.39758155874103));
#54162=CARTESIAN_POINT('Ctrl Pts',(0.701979205024536,-0.0687174176928368,
-4.3817240481651));
#54163=CARTESIAN_POINT('Ctrl Pts',(0.649491722206451,0.275058885634601,
-4.36586653758914));
#54164=CARTESIAN_POINT('Ctrl Pts',(0.439118560152959,0.551970812553023,
-4.35000902701321));
#54165=CARTESIAN_POINT('Ctrl Pts',(0.121999569378052,0.694703528746487,
-4.33415151643726));
#54166=CARTESIAN_POINT('Ctrl Pts',(-0.224776435057083,0.668559976385276,
-4.31829400586132));
#54167=CARTESIAN_POINT('Ctrl Pts',(-0.516911281011339,0.479895421258078,
-4.30243649528538));
#54168=CARTESIAN_POINT('Ctrl Pts',(-0.683389577518488,0.174572544004934,
-4.28657898470943));
#54169=CARTESIAN_POINT('Ctrl Pts',(-0.683741926704308,-0.173187370925052,
-4.27072147413349));
#54170=CARTESIAN_POINT('Ctrl Pts',(-0.517882675605679,-0.478846971472886,
-4.25486396355754));
#54171=CARTESIAN_POINT('Ctrl Pts',(-0.226130737646503,-0.668103118741933,
-4.23900645298161));
#54172=CARTESIAN_POINT('Ctrl Pts',(0.120591577745708,-0.694949321287569,
-4.22314894240565));
#54173=CARTESIAN_POINT('Ctrl Pts',(0.437999149760179,-0.552859505291001,
-4.20729143182972));
#54174=CARTESIAN_POINT('Ctrl Pts',(0.648933011794961,-0.276374445244078,
-4.19143392125377));
#54175=CARTESIAN_POINT('Ctrl Pts',(0.702117012141806,0.0672947920890993,
-4.17557641067783));
#54176=CARTESIAN_POINT('Ctrl Pts',(0.584622591848963,0.394605262105121,
-4.15971890010188));
#54177=CARTESIAN_POINT('Ctrl Pts',(0.325011602776974,0.625990691497561,
-4.14386138952594));
#54178=CARTESIAN_POINT('Ctrl Pts',(-0.0136068253575281,0.705203333858357,
-4.12800387895));
#54179=CARTESIAN_POINT('Ctrl Pts',(-0.348917554886554,0.612987298133689,
-4.11214636837405));
#54180=CARTESIAN_POINT('Ctrl Pts',(-0.599409520346848,0.371759485015262,
-4.09628885779812));
#54181=CARTESIAN_POINT('Ctrl Pts',(-0.704190345811963,0.0401602371317554,
-4.08043134722216));
#54182=CARTESIAN_POINT('Ctrl Pts',(-0.637788741604482,-0.301201608335383,
-4.06457383664623));
#54183=CARTESIAN_POINT('Ctrl Pts',(-0.416346348986597,-0.569344013287909,
-4.04871632607028));
#54184=CARTESIAN_POINT('Ctrl Pts',(-0.0936938502820333,-0.699083936448678,
-4.03285881549434));
#54185=CARTESIAN_POINT('Ctrl Pts',(0.251734792730736,-0.658882752779327,
-4.01700130491839));
#54186=CARTESIAN_POINT('Ctrl Pts',(0.535968939526595,-0.458513013603747,
-4.00114379434245));
#54187=CARTESIAN_POINT('Ctrl Pts',(0.689913789056643,-0.146682826025263,
-3.98528628376651));
#54188=CARTESIAN_POINT('Ctrl Pts',(0.676146713284492,0.200804656061129,
-3.96942877319056));
#54189=CARTESIAN_POINT('Ctrl Pts',(0.49801436627063,0.499478306605316,-3.95357126261462));
#54190=CARTESIAN_POINT('Ctrl Pts',(0.198819142241936,0.676733209218694,
-3.93771375203867));
#54191=CARTESIAN_POINT('Ctrl Pts',(-0.148707252523208,0.689480268628661,
-3.92185624146274));
#54192=CARTESIAN_POINT('Ctrl Pts',(-0.460084232647476,0.534620787708854,
-3.90599873088679));
#54193=CARTESIAN_POINT('Ctrl Pts',(-0.659618814949835,0.249799733277333,
-3.89014122031085));
#54194=CARTESIAN_POINT('Ctrl Pts',(-0.698805911558285,-0.0957454215743307,
-3.8742837097349));
#54195=CARTESIAN_POINT('Ctrl Pts',(-0.568119486722484,-0.418015713325986,
-3.85842619915896));
#54196=CARTESIAN_POINT('Ctrl Pts',(-0.299328251646252,-0.638670091320746,
-3.84256868858302));
#54197=CARTESIAN_POINT('Ctrl Pts',(0.0422270275427583,-0.704069432603173,
-3.82671117800707));
#54198=CARTESIAN_POINT('Ctrl Pts',(0.373517290723508,-0.598315737142038,
-3.81085366743113));
#54199=CARTESIAN_POINT('Ctrl Pts',(0.614008812156318,-0.347116790685268,
-3.79499615685518));
#54200=CARTESIAN_POINT('Ctrl Pts',(0.705240235193272,-0.0115368299714127,
-3.77913864627925));
#54201=CARTESIAN_POINT('Ctrl Pts',(0.625034009757416,0.326847631822259,
-3.76328113570329));
#54202=CARTESIAN_POINT('Ctrl Pts',(0.392887558138946,0.585778332170854,
-3.74742362512736));
#54203=CARTESIAN_POINT('Ctrl Pts',(0.065233624501804,0.702311513514914,
-3.73156611455141));
#54204=CARTESIAN_POINT('Ctrl Pts',(-0.278278024886458,0.648118992659946,
-3.71570860397547));
#54205=CARTESIAN_POINT('Ctrl Pts',(-0.554142753654658,0.436374490951619,
-3.69985109339953));
#54206=CARTESIAN_POINT('Ctrl Pts',(-0.695300292072653,0.11855121941564,
-3.68399358282358));
#54207=CARTESIAN_POINT('Ctrl Pts',(-0.667436494062319,-0.228090802477984,
-3.66813607224764));
#54208=CARTESIAN_POINT('Ctrl Pts',(-0.47732480187785,-0.519285972556088,
-3.65227856167169));
#54209=CARTESIAN_POINT('Ctrl Pts',(-0.171179682347504,-0.684247326726716,
-3.63642105109576));
#54210=CARTESIAN_POINT('Ctrl Pts',(0.176577700272081,-0.682874222348358,
-3.6205635405198));
#54211=CARTESIAN_POINT('Ctrl Pts',(0.48141060950412,-0.51550044892136,-3.60470602994387));
#54212=CARTESIAN_POINT('Ctrl Pts',(0.66921686778135,-0.222813086819806,
-3.58884851936792));
#54213=CARTESIAN_POINT('Ctrl Pts',(0.694342438818249,0.12403816121331,-3.57299100879198));
#54214=CARTESIAN_POINT('Ctrl Pts',(0.550679519060578,0.440736831985327,
-3.55713349821603));
#54215=CARTESIAN_POINT('Ctrl Pts',(0.273151290577277,0.650296286501176,
-3.54127598764009));
#54216=CARTESIAN_POINT('Ctrl Pts',(-0.0707775948694625,0.701774479334883,
-3.52541847706415));
#54217=CARTESIAN_POINT('Ctrl Pts',(-0.397501074521878,0.582657518217351,
-3.5095609664882));
#54218=CARTESIAN_POINT('Ctrl Pts',(-0.627595567226647,0.321901680298058,
-3.49370345591226));
#54219=CARTESIAN_POINT('Ctrl Pts',(-0.705127141838962,-0.0171056021018824,
-3.47784594533632));
#54220=CARTESIAN_POINT('Ctrl Pts',(-0.611248559970205,-0.351954664290164,
-3.46198843476037));
#54221=CARTESIAN_POINT('Ctrl Pts',(-0.368780872539474,-0.601246668040893,
-3.44613092418443));
#54222=CARTESIAN_POINT('Ctrl Pts',(-0.0366658246279656,-0.704380937480284,
-3.43027341360848));
#54223=CARTESIAN_POINT('Ctrl Pts',(0.304362360169178,-0.636286446102303,
-3.41441590303255));
#54224=CARTESIAN_POINT('Ctrl Pts',(0.571402753704327,-0.413516361031052,
-3.3985583924566));
#54225=CARTESIAN_POINT('Ctrl Pts',(0.699540203905405,-0.0902241148542729,
-3.38270088188066));
#54226=CARTESIAN_POINT('Ctrl Pts',(0.657625632702926,0.255000813711106,
-3.36684337130472));
#54227=CARTESIAN_POINT('Ctrl Pts',(0.455848100739092,0.538237305315985,
-3.35098586072876));
#54228=CARTESIAN_POINT('Ctrl Pts',(0.143257937062477,0.690633080043126,
-3.33512835015283));
#54229=CARTESIAN_POINT('Ctrl Pts',(-0.204156960980475,0.675142076206533,
-3.31927083957688));
#54230=CARTESIAN_POINT('Ctrl Pts',(-0.501943111877064,0.495530019494702,
-3.30341332900094));
#54231=CARTESIAN_POINT('Ctrl Pts',(-0.677711342534395,0.195459008442898,
-3.28755581842499));
#54232=CARTESIAN_POINT('Ctrl Pts',(-0.688733954451453,-0.152126354609959,
-3.27169830784905));
#54233=CARTESIAN_POINT('Ctrl Pts',(-0.532331448398351,-0.462731149618616,
-3.25584079727311));
#54234=CARTESIAN_POINT('Ctrl Pts',(-0.246523886922497,-0.660850104757407,
-3.23998328669717));
#54235=CARTESIAN_POINT('Ctrl Pts',(0.0992114457684886,-0.698322258566757,
-3.22412577612122));
#54236=CARTESIAN_POINT('Ctrl Pts',(0.420829355607847,-0.566038462686005,
-3.20826826554528));
#54237=CARTESIAN_POINT('Ctrl Pts',(0.640147380197513,-0.296155735057606,
-3.19241075496933));
#54238=CARTESIAN_POINT('Ctrl Pts',(0.703851252246643,0.0457198260286,-3.17655324439339));
#54239=CARTESIAN_POINT('Ctrl Pts',(0.596455125262476,0.376481302762003,
-3.16069573381745));
#54240=CARTESIAN_POINT('Ctrl Pts',(0.344066045534297,0.615723512700013,
-3.14483822324151));
#54241=CARTESIAN_POINT('Ctrl Pts',(0.00803756064714361,0.705288795742634,
-3.12898071266556));
#54242=CARTESIAN_POINT('Ctrl Pts',(-0.32994478397183,0.623404625673433,
-3.11312320208962));
#54243=CARTESIAN_POINT('Ctrl Pts',(-0.587720476917705,0.38997631824622,
-3.09726569151367));
#54244=CARTESIAN_POINT('Ctrl Pts',(-0.702626532690257,0.0617482254070272,
-3.08140818093773));
#54245=CARTESIAN_POINT('Ctrl Pts',(-0.646730307895239,-0.281490313565102,
-3.06555067036178));
#54246=CARTESIAN_POINT('Ctrl Pts',(-0.433619679201001,-0.556301053019741,
-3.04969315978585));
#54247=CARTESIAN_POINT('Ctrl Pts',(-0.115099950991358,-0.695879938684137,
-3.0338356492099));
#54248=CARTESIAN_POINT('Ctrl Pts',(0.231399554821144,-0.666296580968136,
-3.01797813863396));
#54249=CARTESIAN_POINT('Ctrl Pts',(0.521647880459103,-0.474742431844655,
-3.00212062805801));
#54250=CARTESIAN_POINT('Ctrl Pts',(0.685088231319183,-0.167782606634913,
-2.98626311748207));
#54251=CARTESIAN_POINT('Ctrl Pts',(0.681989707179352,0.179963682677014,
-2.97040560690613));
#54252=CARTESIAN_POINT('Ctrl Pts',(0.513105531786303,0.48396239629908,-2.95454809633019));
#54253=CARTESIAN_POINT('Ctrl Pts',(0.219489950840751,0.670314142220776,
-2.93869058575424));
#54254=CARTESIAN_POINT('Ctrl Pts',(-0.127481691142976,0.693718463214421,
-2.92283307517829));
#54255=CARTESIAN_POINT('Ctrl Pts',(-0.443463664270248,0.548485976350586,
-2.90697556460236));
#54256=CARTESIAN_POINT('Ctrl Pts',(-0.651643552389154,0.269921411545835,
-2.89111805402641));
#54257=CARTESIAN_POINT('Ctrl Pts',(-0.701414670433489,-0.0742586552661132,
-2.87526054345047));
#54258=CARTESIAN_POINT('Ctrl Pts',(-0.580678100880426,-0.400387101364609,
-2.85940303287452));
#54259=CARTESIAN_POINT('Ctrl Pts',(-0.318783833330571,-0.629184992977676,
-2.84354552229858));
#54260=CARTESIAN_POINT('Ctrl Pts',(0.0206039577451542,-0.705033591190155,
-2.82768801172263));
#54261=CARTESIAN_POINT('Ctrl Pts',(0.35498310936897,-0.609494774254864,
-2.81183050114669));
#54262=CARTESIAN_POINT('Ctrl Pts',(0.603069014406956,-0.365793181515832,
-2.79597299057075));
#54263=CARTESIAN_POINT('Ctrl Pts',(0.704554188889049,-0.0331705094948168,
-2.78011547999481));
#54264=CARTESIAN_POINT('Ctrl Pts',(0.634768486672358,0.307515619292639,
-2.76425796941886));
#54265=CARTESIAN_POINT('Ctrl Pts',(0.410676193241495,0.573447427482177,
-2.74840045884292));
#54266=CARTESIAN_POINT('Ctrl Pts',(0.0867521583136464,0.699979250270445,
-2.73254294826698));
#54267=CARTESIAN_POINT('Ctrl Pts',(-0.258260557150356,0.656352323376431,
-2.71668543769103));
#54268=CARTESIAN_POINT('Ctrl Pts',(-0.54049242092486,0.453171965929088,
-2.70082792711509));
#54269=CARTESIAN_POINT('Ctrl Pts',(-0.691335369211096,0.139829521414503,
-2.68497041653915));
#54270=CARTESIAN_POINT('Ctrl Pts',(-0.674120818663402,-0.207504240018937,
-2.6691129059632));
#54271=CARTESIAN_POINT('Ctrl Pts',(-0.493033473894675,-0.504395560448939,
-2.65325539538726));
#54272=CARTESIAN_POINT('Ctrl Pts',(-0.19209406288682,-0.678672792135419,
-2.63739788481132));
#54273=CARTESIAN_POINT('Ctrl Pts',(0.155541711691216,-0.687970685207893,
-2.62154037423537));
#54274=CARTESIAN_POINT('Ctrl Pts',(0.465366675199364,-0.530029004296125,
-2.60568286365943));
#54275=CARTESIAN_POINT('Ctrl Pts',(0.662065125935696,-0.243241971709246,
-2.58982535308348));
#54276=CARTESIAN_POINT('Ctrl Pts',(0.697821414466598,0.102675027602084,
-2.57396784250754));
#54277=CARTESIAN_POINT('Ctrl Pts',(0.563943504067627,0.423632638026367,
-2.5581103319316));
#54278=CARTESIAN_POINT('Ctrl Pts',(0.292975927787107,0.641608910099083,
-2.54225282135566));
#54279=CARTESIAN_POINT('Ctrl Pts',(-0.0492114989961208,0.703615744670204,
-2.52639531077971));
#54280=CARTESIAN_POINT('Ctrl Pts',(-0.379436046685527,0.594579830011842,
-2.51053780020377));
#54281=CARTESIAN_POINT('Ctrl Pts',(-0.617423055528672,0.341006830258411,
-2.49468028962782));
#54282=CARTESIAN_POINT('Ctrl Pts',(-0.705319993683033,0.00453809345638933,
-2.47882277905188));
#54283=CARTESIAN_POINT('Ctrl Pts',(-0.621759894782861,-0.333033813629871,
-2.46296526847594));
#54284=CARTESIAN_POINT('Ctrl Pts',(-0.387055478021894,-0.589648153320687,
-2.4471077579));
#54285=CARTESIAN_POINT('Ctrl Pts',(-0.0582613062111292,-0.70292425479551,
-2.43125024732405));
#54286=CARTESIAN_POINT('Ctrl Pts',(0.284695672591286,-0.645325702098597,
-2.41539273674811));
#54287=CARTESIAN_POINT('Ctrl Pts',(0.558445657515852,-0.430854192718303,
-2.39953522617216));
#54288=CARTESIAN_POINT('Ctrl Pts',(0.696442454311359,-0.111645849067578,
-2.38367771559622));
#54289=CARTESIAN_POINT('Ctrl Pts',(0.665140265164793,0.234702610632607,
-2.36782020502028));
#54290=CARTESIAN_POINT('Ctrl Pts',(0.472148374730573,0.523996946575577,
-2.35196269444434));
#54291=CARTESIAN_POINT('Ctrl Pts',(0.164381400495464,0.685912270594717,
-2.33610518386839));
#54292=CARTESIAN_POINT('Ctrl Pts',(-0.183345234784635,0.681088402972051,
-2.32024767329245));
#54293=CARTESIAN_POINT('Ctrl Pts',(-0.486502269038555,0.510697983157941,
-2.3043901627165));
#54294=CARTESIAN_POINT('Ctrl Pts',(-0.671394915047807,0.216161411517411,
-2.28853265214056));
#54295=CARTESIAN_POINT('Ctrl Pts',(-0.69307740983695,-0.130922082762827,
-2.27267514156461));
#54296=CARTESIAN_POINT('Ctrl Pts',(-0.546278931161056,-0.446179579486538,
-2.25681763098868));
#54297=CARTESIAN_POINT('Ctrl Pts',(-0.266684887662029,-0.652974776292271,
-2.24096012041273));
#54298=CARTESIAN_POINT('Ctrl Pts',(0.0777378875832581,-0.701037594295302,
-2.22510260983679));
#54299=CARTESIAN_POINT('Ctrl Pts',(0.403263271585882,-0.578684388566949,
-2.20924509926084));
#54300=CARTESIAN_POINT('Ctrl Pts',(0.630758929622586,-0.315658138628835,
-2.1933875886849));
#54301=CARTESIAN_POINT('Ctrl Pts',(0.704922684214943,0.0241018061657587,
-2.17753007810895));
#54302=CARTESIAN_POINT('Ctrl Pts',(0.607725984161892,0.358002815569531,
-2.16167256753301));
#54303=CARTESIAN_POINT('Ctrl Pts',(0.362796485494498,0.604876514583012,
-2.14581505695707));
#54304=CARTESIAN_POINT('Ctrl Pts',(0.0296743777790237,0.704710095773204,
-2.12995754638113));
#54305=CARTESIAN_POINT('Ctrl Pts',(-0.310661308079694,0.633234900683358,
-2.11410003580518));
#54306=CARTESIAN_POINT('Ctrl Pts',(-0.575477984286229,0.407825915536408,
-2.09824252522924));
#54307=CARTESIAN_POINT('Ctrl Pts',(-0.700401064735479,0.0832780661318421,
-2.08238501465329));
#54308=CARTESIAN_POINT('Ctrl Pts',(-0.655062856145828,-0.261513942800995,
-2.06652750407735));
#54309=CARTESIAN_POINT('Ctrl Pts',(-0.450484675054114,-0.542734230837378,
-2.05066999350141));
#54310=CARTESIAN_POINT('Ctrl Pts',(-0.13639766348118,-0.692020639271782,
-2.03481248292547));
#54311=CARTESIAN_POINT('Ctrl Pts',(0.210846410774077,-0.67308296579615,
-2.01895497234952));
#54312=CARTESIAN_POINT('Ctrl Pts',(0.506835591947215,-0.490524790929845,
-2.00309746177358));
#54313=CARTESIAN_POINT('Ctrl Pts',(0.679617534353063,-0.188724388411024,
-1.98723995119763));
#54314=CARTESIAN_POINT('Ctrl Pts',(0.687190479687935,0.158953239688651,
-1.97138244062169));
#54315=CARTESIAN_POINT('Ctrl Pts',(0.527713512083115,0.467990744509071,
-1.95552493004575));
#54316=CARTESIAN_POINT('Ctrl Pts',(0.239954068430876,0.663263848573645,
-1.93966741946981));
#54317=CARTESIAN_POINT('Ctrl Pts',(-0.106136081809596,0.697303391587448,
-1.92380990889386));
#54318=CARTESIAN_POINT('Ctrl Pts',(-0.426425491571088,0.561834662440479,
-1.90795239831792));
#54319=CARTESIAN_POINT('Ctrl Pts',(-0.643054645045905,0.289788908114401,
-1.89209488774197));
#54320=CARTESIAN_POINT('Ctrl Pts',(-0.703362915671523,-0.0527019604882636,
-1.87623737716603));
#54321=CARTESIAN_POINT('Ctrl Pts',(-0.592689897555636,-0.382381449755007,
-1.86037986659008));
#54322=CARTESIAN_POINT('Ctrl Pts',(-0.337939220168536,-0.619107398803415,
-1.84452235601415));
#54323=CARTESIAN_POINT('Ctrl Pts',(-0.00103851454807973,-0.705333828246443,
-1.8286648454382));
#54324=CARTESIAN_POINT('Ctrl Pts',(0.336114644751484,-0.620099857575242,
-1.81280733486226));
#54325=CARTESIAN_POINT('Ctrl Pts',(0.591561313924781,-0.384125109370422,
-1.79694982428632));
#54326=CARTESIAN_POINT('Ctrl Pts',(0.70320467250143,-0.0547729527541542,
-1.78109231371037));
#54327=CARTESIAN_POINT('Ctrl Pts',(0.64390520984823,0.287894023056329,-1.76523480313443));
#54328=CARTESIAN_POINT('Ctrl Pts',(0.428078099583546,0.560576514347677,
-1.74937729255848));
#54329=CARTESIAN_POINT('Ctrl Pts',(0.10818899867648,0.69698782510646,-1.73351978198254));
#54330=CARTESIAN_POINT('Ctrl Pts',(-0.237999888598618,0.663967575118165,
-1.7176622714066));
#54331=CARTESIAN_POINT('Ctrl Pts',(-0.526333113076832,0.469542694395412,
-1.70180476083065));
#54332=CARTESIAN_POINT('Ctrl Pts',(-0.686719424267349,0.160976147659122,
-1.68594725025471));
#54333=CARTESIAN_POINT('Ctrl Pts',(-0.680170331914515,-0.186722273348817,
-1.67008973967877));
#54334=CARTESIAN_POINT('Ctrl Pts',(-0.508277862304651,-0.489030165196652,
-1.65423222910282));
#54335=CARTESIAN_POINT('Ctrl Pts',(-0.212827550790863,-0.672459159656269,
-1.63837471852688));
#54336=CARTESIAN_POINT('Ctrl Pts',(0.134359251378219,-0.692419294467113,
-1.62251720795094));
#54337=CARTESIAN_POINT('Ctrl Pts',(0.448884510774523,-0.54405843782444,
-1.60665969737499));
#54338=CARTESIAN_POINT('Ctrl Pts',(0.65428992543882,-0.263441798601729,
-1.59080218679905));
#54339=CARTESIAN_POINT('Ctrl Pts',(0.700643260203079,0.0812152061701052,
-1.57494467622311));
#54340=CARTESIAN_POINT('Ctrl Pts',(0.576676430357581,0.406129514380929,
-1.55908716564716));
#54341=CARTESIAN_POINT('Ctrl Pts',(0.312524673140342,0.63231733841464,-1.54322965507122));
#54342=CARTESIAN_POINT('Ctrl Pts',(-0.0275990612546199,0.704794423643601,
-1.52737214449527));
#54343=CARTESIAN_POINT('Ctrl Pts',(-0.361013708553533,0.605942233234882,
-1.51151463391933));
#54344=CARTESIAN_POINT('Ctrl Pts',(-0.606669124072505,0.359790858247332,
-1.49565712334339));
#54345=CARTESIAN_POINT('Ctrl Pts',(-0.704848654294675,0.0261775155474184,
-1.47979961276745));
#54346=CARTESIAN_POINT('Ctrl Pts',(-0.631685725888709,-0.313799349090631,
-1.4639421021915));
#54347=CARTESIAN_POINT('Ctrl Pts',(-0.404965598083139,-0.577494374128802,
-1.44808459161556));
#54348=CARTESIAN_POINT('Ctrl Pts',(-0.0798019238330923,-0.700805636916392,
-1.43222708103962));
#54349=CARTESIAN_POINT('Ctrl Pts',(0.264760890572085,-0.65375726275486,
-1.41636957046367));
#54350=CARTESIAN_POINT('Ctrl Pts',(0.544962679865294,-0.447786294269141,
-1.40051205988773));
#54351=CARTESIAN_POINT('Ctrl Pts',(0.692688873355398,-0.13296244774702,
-1.38465454931178));
#54352=CARTESIAN_POINT('Ctrl Pts',(0.672028543154347,0.21418339096928,-1.36879703873584));
#54353=CARTESIAN_POINT('Ctrl Pts',(0.488004032358267,0.509263146303875,
-1.3529395281599));
#54354=CARTESIAN_POINT('Ctrl Pts',(0.185350067969226,0.680545545929922,
-1.33708201758396));
#54355=CARTESIAN_POINT('Ctrl Pts',(-0.162360854618199,0.686393357098464,
-1.32122450700801));
#54356=CARTESIAN_POINT('Ctrl Pts',(-0.470603292949117,0.525385028761478,
-1.30536699643207));
#54357=CARTESIAN_POINT('Ctrl Pts',(-0.664446243161424,0.236660258028087,
-1.28950948585612));
#54358=CARTESIAN_POINT('Ctrl Pts',(-0.696768202681856,-0.109594523187739,
-1.27365197528018));
#54359=CARTESIAN_POINT('Ctrl Pts',(-0.559711989719446,-0.429207847488311,
-1.25779446470423));
#54360=CARTESIAN_POINT('Ctrl Pts',(-0.286594754496667,-0.644484549447267,
-1.2419369541283));
#54361=CARTESIAN_POINT('Ctrl Pts',(0.0561911245777891,-0.703092771474672,
-1.22607944355235));
#54362=CARTESIAN_POINT('Ctrl Pts',(0.385317439461293,-0.590785374419714,
-1.21022193297641));
#54363=CARTESIAN_POINT('Ctrl Pts',(0.620776501059534,-0.33486329078227,
-1.19436442240046));
#54364=CARTESIAN_POINT('Ctrl Pts',(0.705330299092296,0.00246108992610756,
-1.17850691182452));
#54365=CARTESIAN_POINT('Ctrl Pts',(0.618424554916906,0.339187201493628,
-1.16264940124858));
#54366=CARTESIAN_POINT('Ctrl Pts',(0.381185284430804,0.593459911632335,
-1.14679189067263));
#54367=CARTESIAN_POINT('Ctrl Pts',(0.0512832509114107,0.703467778904769,
-1.13093438009669));
#54368=CARTESIAN_POINT('Ctrl Pts',(-0.291085286224135,0.642468866113421,
-1.11507686952075));
#54369=CARTESIAN_POINT('Ctrl Pts',(-0.562693571058386,0.425291468137809,
-1.0992193589448));
#54370=CARTESIAN_POINT('Ctrl Pts',(-0.697516037643649,0.104729484917831,
-1.08336184836886));
#54371=CARTESIAN_POINT('Ctrl Pts',(-0.662778539697212,-0.241291307547711,
-1.06750433779292));
#54372=CARTESIAN_POINT('Ctrl Pts',(-0.466925454985086,-0.528656322451762,
-1.05164682721697));
#54373=CARTESIAN_POINT('Ctrl Pts',(-0.157566931955473,-0.687509672466789,
-1.03578931664103));
#54374=CARTESIAN_POINT('Ctrl Pts',(0.190094715234546,-0.679235516607566,
-1.01993180606508));
#54375=CARTESIAN_POINT('Ctrl Pts',(0.491546022542315,-0.505845228804307,
-1.00407429548914));
#54376=CARTESIAN_POINT('Ctrl Pts',(0.673506849846877,-0.209488450733178,
-0.988216784913199));
#54377=CARTESIAN_POINT('Ctrl Pts',(0.691744133306218,0.137793112373883,
-0.972359274337254));
#54378=CARTESIAN_POINT('Ctrl Pts',(0.541824551004231,0.45157839154494,-0.956501763761313));
#54379=CARTESIAN_POINT('Ctrl Pts',(0.260192224202427,0.655588967452813,
-0.940644253185368));
#54380=CARTESIAN_POINT('Ctrl Pts',(-0.0846905254229573,0.700231677864431,
-0.924786742609425));
#54381=CARTESIAN_POINT('Ctrl Pts',(-0.408985759189344,0.574654275683705,
-0.908929232033481));
#54382=CARTESIAN_POINT('Ctrl Pts',(-0.633860180989338,0.30938351400392,
-0.89307172145754));
#54383=CARTESIAN_POINT('Ctrl Pts',(-0.704648812633615,-0.0310956369172294,
-0.877214210881594));
#54384=CARTESIAN_POINT('Ctrl Pts',(-0.604143565385745,-0.364015714199608,
-0.861356700305653));
#54385=CARTESIAN_POINT('Ctrl Pts',(-0.356776373766072,-0.608446798745448,
-0.845499189729708));
#54386=CARTESIAN_POINT('Ctrl Pts',(-0.0226800088848199,-0.704969861042468,
-0.829641679153765));
#54387=CARTESIAN_POINT('Ctrl Pts',(0.316929665073997,-0.630121000425581,
-0.813784168577821));
#54388=CARTESIAN_POINT('Ctrl Pts',(0.579496547370947,-0.40209531129622,
-0.797926658001879));
#54389=CARTESIAN_POINT('Ctrl Pts',(0.701192956853533,-0.0763238169921492,
-0.782069147425935));
#54390=CARTESIAN_POINT('Ctrl Pts',(0.652435575344282,0.268001320531126,
-0.76621163684999));
#54391=CARTESIAN_POINT('Ctrl Pts',(0.445076890002194,0.547177713149235,
-0.750354126274048));
#54392=CARTESIAN_POINT('Ctrl Pts',(0.129523958779256,0.693340055011537,
-0.734496615698105));
#54393=CARTESIAN_POINT('Ctrl Pts',(-0.217515098455649,0.670957576695487,
-0.718639105122159));
#54394=CARTESIAN_POINT('Ctrl Pts',(-0.511678163758033,0.485471260235309,
-0.702781594546218));
#54395=CARTESIAN_POINT('Ctrl Pts',(-0.681456804020454,0.181971184629545,
-0.686924083970274));
#54396=CARTESIAN_POINT('Ctrl Pts',(-0.685579337062831,-0.165764472592108,
-0.671066573394329));
#54397=CARTESIAN_POINT('Ctrl Pts',(-0.523043611653193,-0.47320425620448,
-0.655209062818387));
#54398=CARTESIAN_POINT('Ctrl Pts',(-0.233360621587032,-0.66561228059116,
-0.639351552242444));
#54399=CARTESIAN_POINT('Ctrl Pts',(0.113050266597516,-0.696215860924957,
-0.6234940416665));
#54400=CARTESIAN_POINT('Ctrl Pts',(0.431979637282727,-0.55757553815993,
-0.607636531090557));
#54401=CARTESIAN_POINT('Ctrl Pts',(0.645898588102162,-0.283393545566738,
-0.591779020514614));
#54402=CARTESIAN_POINT('Ctrl Pts',(0.702805318729989,0.0596789053693757,
-0.57592150993867));
#54403=CARTESIAN_POINT('Ctrl Pts',(0.588866307489121,0.388243943526985,
-0.560063999362727));
#54404=CARTESIAN_POINT('Ctrl Pts',(0.331779117822002,0.622430321207524,
-0.544206488786783));
#54405=CARTESIAN_POINT('Ctrl Pts',(-0.00596063381383579,0.705309406307461,
-0.52834897821084));
#54406=CARTESIAN_POINT('Ctrl Pts',(-0.34225140821695,0.616734028050019,
-0.512491467634896));
#54407=CARTESIAN_POINT('Ctrl Pts',(-0.595343899704099,0.378236075574855,
-0.496633957058954));
#54408=CARTESIAN_POINT('Ctrl Pts',(-0.703713567528586,0.0477922865914934,
-0.480776446483009));
#54409=CARTESIAN_POINT('Ctrl Pts',(-0.641016706253422,-0.294269383533106,
-0.464918935907065));
#54410=CARTESIAN_POINT('Ctrl Pts',(-0.422494366982188,-0.564796775530692,
-0.449061425331123));
#54411=CARTESIAN_POINT('Ctrl Pts',(-0.101267392955972,-0.698027078919814,
-0.433203914755179));
#54412=CARTESIAN_POINT('Ctrl Pts',(0.244576786450544,-0.661573188172743,
-0.417346404179235));
#54413=CARTESIAN_POINT('Ctrl Pts',(0.530966517512247,-0.464296720931165,
-0.401488893603292));
#54414=CARTESIAN_POINT('Ctrl Pts',(0.68828299573105,-0.1541538373096,-0.385631383027349));
#54415=CARTESIAN_POINT('Ctrl Pts',(0.678283980079609,0.193462477415893,
-0.369773872451405));
#54416=CARTESIAN_POINT('Ctrl Pts',(0.503400142512799,0.494049779148767,
-0.353916361875461));
#54417=CARTESIAN_POINT('Ctrl Pts',(0.206144193604109,0.674537959812384,
-0.338058851299519));
#54418=CARTESIAN_POINT('Ctrl Pts',(-0.141223581330571,0.691051943005463,
-0.322201340723575));
#54419=CARTESIAN_POINT('Ctrl Pts',(-0.454261155256553,0.539577325634538,
-0.306343830147631));
#54420=CARTESIAN_POINT('Ctrl Pts',(-0.65687187079242,0.256936244576825,
-0.29048631957169));
#54421=CARTESIAN_POINT('Ctrl Pts',(-0.699802856556483,-0.0881637600130705,
-0.274628808995744));
#54422=CARTESIAN_POINT('Ctrl Pts',(-0.572617975996934,-0.411831935255785,
-0.258771298419802));
#54423=CARTESIAN_POINT('Ctrl Pts',(-0.306234735283331,-0.635387420227233,
-0.242913787843858));
#54424=CARTESIAN_POINT('Ctrl Pts',(0.0345914406976117,-0.704485853085711,
-0.227056277267915));
#54425=CARTESIAN_POINT('Ctrl Pts',(0.367008771067512,-0.602330028183672,
-0.21119876669197));
#54426=CARTESIAN_POINT('Ctrl Pts',(0.610209470489882,-0.353753099832041,
-0.195341256116028));
#54427=CARTESIAN_POINT('Ctrl Pts',(0.705073760608792,-0.0191819564521373,
-0.179483745540084));
#54428=CARTESIAN_POINT('Ctrl Pts',(0.62854066985661,0.320052203509621,-0.16362623496414));
#54429=CARTESIAN_POINT('Ctrl Pts',(0.399215307462047,0.58148440677362,-0.147768724388197));
#54430=CARTESIAN_POINT('Ctrl Pts',(0.0728434763577143,0.701563108700217,
-0.131911213812254));
#54431=CARTESIAN_POINT('Ctrl Pts',(-0.271234459526246,0.651097643395513,
-0.11605370323631));
#54432=CARTESIAN_POINT('Ctrl Pts',(-0.549380630953683,0.442356886629713,
-0.100196192660368));
#54433=CARTESIAN_POINT('Ctrl Pts',(-0.693971520902736,0.126081582258689,
-0.084338682084424));
#54434=CARTESIAN_POINT('Ctrl Pts',(-0.669875267596679,-0.220840084321447,
-0.0684811715084805));
#54435=CARTESIAN_POINT('Ctrl Pts',(-0.482916401293059,-0.514083268386795,
-0.0526236609325368));
#54436=CARTESIAN_POINT('Ctrl Pts',(-0.178607888241887,-0.68234590671203,
-0.0367661503565942));
#54437=CARTESIAN_POINT('Ctrl Pts',(0.169206013737912,-0.684760397665597,
-0.0209086397806501));
#54438=CARTESIAN_POINT('Ctrl Pts',(0.373522557112378,-0.575353242974678,
-0.0103369660633542));
#54439=CARTESIAN_POINT('Ctrl Pts',(0.456477694810146,-0.499550802362297,
-0.00505112920470641));
#54440=CARTESIAN_POINT('Ctrl Pts',(0.533647856309019,-0.584002718706676,
-0.0710999999999995));
#54441=CARTESIAN_POINT('Ctrl Pts',(0.43666867878175,-0.672619994853351,
-0.0763858368586472));
#54442=CARTESIAN_POINT('Ctrl Pts',(0.3172399677846,-0.736571524390805,-0.0816716737172953));
#54443=CARTESIAN_POINT('Ctrl Pts',(0.189756640842203,-0.768076843419576,
-0.0869575105759432));
#54444=CARTESIAN_POINT('Ctrl Pts',(0.0622733138997992,-0.79958216244835,
-0.0922433474345914));
#54445=CARTESIAN_POINT('Ctrl Pts',(-0.073264628987864,-0.798641270968439,
-0.09752918429324));
#54446=CARTESIAN_POINT('Ctrl Pts',(-0.200325867973879,-0.765386092166293,
-0.102815021151888));
#54447=CARTESIAN_POINT('Ctrl Pts',(-0.327387106959887,-0.732130913364149,
-0.108100858010536));
#54448=CARTESIAN_POINT('Ctrl Pts',(-0.445971642044243,-0.666561447239783,
-0.113386694869182));
#54449=CARTESIAN_POINT('Ctrl Pts',(-0.541691464665684,-0.576640444310574,
-0.11867253172783));
#54450=CARTESIAN_POINT('Ctrl Pts',(-0.637411287287125,-0.486719441381364,
-0.123958368586478));
#54451=CARTESIAN_POINT('Ctrl Pts',(-0.71026639744564,-0.372446901647311,
-0.129244205445126));
#54452=CARTESIAN_POINT('Ctrl Pts',(-0.751388929617263,-0.24771550581813,
-0.134530042303774));
#54453=CARTESIAN_POINT('Ctrl Pts',(-0.777676231444153,-0.167981800807776,
-0.137908977927949));
#54454=CARTESIAN_POINT('Ctrl Pts',(-0.790996587895958,-0.0839742729858109,
-0.141287913552124));
#54455=CARTESIAN_POINT('Ctrl Pts',(-0.791053554504038,1.52922707510328E-5,
-0.144666849176299));
#54456=CARTESIAN_POINT('Origin',(0.,0.,-0.599));
#54457=CARTESIAN_POINT('',(0.23094010767585,-0.4,-0.599));
#54458=CARTESIAN_POINT('',(-0.230940107675851,-0.4,-0.599));
#54459=CARTESIAN_POINT('',(0.115470053837925,-0.4,-0.599));
#54460=CARTESIAN_POINT('Origin',(0.,0.,-0.599));
#54461=CARTESIAN_POINT('Origin',(0.,0.,-0.599));
#54462=CARTESIAN_POINT('',(-0.461880215351701,1.11022302462516E-16,-0.599));
#54463=CARTESIAN_POINT('',(-0.288675134594813,-0.3,-0.599));
#54464=CARTESIAN_POINT('Origin',(0.,0.,-0.599));
#54465=CARTESIAN_POINT('Origin',(0.,0.,-0.599));
#54466=CARTESIAN_POINT('',(-0.23094010767585,0.4,-0.599));
#54467=CARTESIAN_POINT('',(-0.404145188432738,0.1,-0.599));
#54468=CARTESIAN_POINT('Origin',(0.,0.,-0.599));
#54469=CARTESIAN_POINT('Origin',(0.,0.,-0.599));
#54470=CARTESIAN_POINT('',(0.23094010767585,0.4,-0.599));
#54471=CARTESIAN_POINT('',(-0.115470053837925,0.4,-0.599));
#54472=CARTESIAN_POINT('Origin',(0.,0.,-0.599));
#54473=CARTESIAN_POINT('Origin',(0.,0.,-0.599));
#54474=CARTESIAN_POINT('',(0.461880215351701,0.,-0.599));
#54475=CARTESIAN_POINT('',(0.288675134594813,0.3,-0.599));
#54476=CARTESIAN_POINT('Origin',(0.,0.,-0.599));
#54477=CARTESIAN_POINT('Origin',(0.,0.,-0.599));
#54478=CARTESIAN_POINT('',(0.404145188432738,-0.1,-0.599));
#54479=CARTESIAN_POINT('Origin',(0.,0.,-0.599));
#54480=CARTESIAN_POINT('Origin',(0.,0.,-0.73806406460551));
#54481=CARTESIAN_POINT('',(0.,0.,-0.87712812921102));
#54482=CARTESIAN_POINT('',(-0.460219541126976,-5.63606387946214E-17,-0.6));
#54483=CARTESIAN_POINT('',(-0.23094010767585,-2.82820063659975E-17,-0.73806406460551));
#54484=CARTESIAN_POINT('',(-0.460210453731243,-0.00289211196316049,-0.6));
#54485=CARTESIAN_POINT('Origin',(0.,0.,-0.6));
#54486=CARTESIAN_POINT('Ctrl Pts',(-0.4618802153517,-6.93889390390722E-16,
-0.599));
#54487=CARTESIAN_POINT('Ctrl Pts',(-0.461043830945924,-0.00144866028546382,
-0.599503641468823));
#54488=CARTESIAN_POINT('Ctrl Pts',(-0.460210453731243,-0.00289211196316079,
-0.6));
#54489=CARTESIAN_POINT('',(-0.232609869296308,-0.397107888036839,-0.6));
#54490=CARTESIAN_POINT('Ctrl Pts',(-0.232609869296308,-0.397107888036839,
-0.6));
#54491=CARTESIAN_POINT('Ctrl Pts',(-0.231776492081632,-0.398551339714529,
-0.599503641468825));
#54492=CARTESIAN_POINT('Ctrl Pts',(-0.230940107675851,-0.399999999999999,
-0.599));
#54493=CARTESIAN_POINT('',(-0.227600584434936,-0.4,-0.6));
#54494=CARTESIAN_POINT('Origin',(0.,0.,-0.6));
#54495=CARTESIAN_POINT('Ctrl Pts',(-0.23094010767585,-0.4,-0.599));
#54496=CARTESIAN_POINT('Ctrl Pts',(-0.229267338864258,-0.4,-0.599503641468835));
#54497=CARTESIAN_POINT('Ctrl Pts',(-0.227600584434936,-0.4,-0.6));
#54498=CARTESIAN_POINT('',(0.227600584434936,-0.4,-0.6));
#54499=CARTESIAN_POINT('Ctrl Pts',(0.227600584434936,-0.4,-0.6));
#54500=CARTESIAN_POINT('Ctrl Pts',(0.229267338864223,-0.4,-0.599503641468845));
#54501=CARTESIAN_POINT('Ctrl Pts',(0.23094010767585,-0.4,-0.599));
#54502=CARTESIAN_POINT('',(0.232609869296308,-0.397107888036839,-0.6));
#54503=CARTESIAN_POINT('Origin',(0.,0.,-0.6));
#54504=CARTESIAN_POINT('Ctrl Pts',(0.230940107675851,-0.399999999999999,
-0.599));
#54505=CARTESIAN_POINT('Ctrl Pts',(0.231776492081654,-0.39855133971449,
-0.599503641468839));
#54506=CARTESIAN_POINT('Ctrl Pts',(0.232609869296308,-0.397107888036839,
-0.6));
#54507=CARTESIAN_POINT('',(0.460210453731243,-0.0028921119631606,-0.6));
#54508=CARTESIAN_POINT('Ctrl Pts',(0.460210453731243,-0.00289211196316057,
-0.6));
#54509=CARTESIAN_POINT('Ctrl Pts',(0.461043830945901,-0.00144866028550258,
-0.599503641468836));
#54510=CARTESIAN_POINT('Ctrl Pts',(0.4618802153517,-7.21644966006351E-16,
-0.599));
#54511=CARTESIAN_POINT('',(0.460210453731243,0.0028921119631606,-0.6));
#54512=CARTESIAN_POINT('Origin',(0.,0.,-0.6));
#54513=CARTESIAN_POINT('Ctrl Pts',(0.4618802153517,9.15933995315753E-16,
-0.599));
#54514=CARTESIAN_POINT('Ctrl Pts',(0.461043830945894,0.00144866028551485,
-0.59950364146884));
#54515=CARTESIAN_POINT('Ctrl Pts',(0.460210453731243,0.0028921119631606,
-0.6));
#54516=CARTESIAN_POINT('',(0.232609869296308,0.397107888036839,-0.6));
#54517=CARTESIAN_POINT('Ctrl Pts',(0.232609869296308,0.397107888036839,
-0.6));
#54518=CARTESIAN_POINT('Ctrl Pts',(0.231776492081656,0.398551339714487,
-0.59950364146884));
#54519=CARTESIAN_POINT('Ctrl Pts',(0.230940107675851,0.399999999999999,
-0.599));
#54520=CARTESIAN_POINT('',(0.227600584434936,0.4,-0.6));
#54521=CARTESIAN_POINT('Origin',(0.,0.,-0.6));
#54522=CARTESIAN_POINT('Ctrl Pts',(0.23094010767585,0.4,-0.599));
#54523=CARTESIAN_POINT('Ctrl Pts',(0.229267338864267,0.4,-0.599503641468832));
#54524=CARTESIAN_POINT('Ctrl Pts',(0.227600584434936,0.4,-0.6));
#54525=CARTESIAN_POINT('',(-0.227600584434936,0.4,-0.6));
#54526=CARTESIAN_POINT('Ctrl Pts',(-0.227600584434935,0.4,-0.6));
#54527=CARTESIAN_POINT('Ctrl Pts',(-0.22926733886426,0.4,-0.599503641468834));
#54528=CARTESIAN_POINT('Ctrl Pts',(-0.230940107675849,0.4,-0.599));
#54529=CARTESIAN_POINT('',(-0.232609869296308,0.397107888036839,-0.6));
#54530=CARTESIAN_POINT('Origin',(0.,0.,-0.6));
#54531=CARTESIAN_POINT('Ctrl Pts',(-0.230940107675851,0.399999999999999,
-0.599));
#54532=CARTESIAN_POINT('Ctrl Pts',(-0.231776492081655,0.398551339714488,
-0.599503641468839));
#54533=CARTESIAN_POINT('Ctrl Pts',(-0.232609869296308,0.397107888036839,
-0.6));
#54534=CARTESIAN_POINT('',(-0.460210453731243,0.00289211196316071,-0.6));
#54535=CARTESIAN_POINT('Ctrl Pts',(-0.460210453731243,0.00289211196316076,
-0.6));
#54536=CARTESIAN_POINT('Ctrl Pts',(-0.461043830945898,0.00144866028550932,
-0.599503641468838));
#54537=CARTESIAN_POINT('Ctrl Pts',(-0.4618802153517,9.15933995315753E-16,
-0.599));
#54538=CARTESIAN_POINT('Origin',(0.,0.,-0.6));
#54539=CARTESIAN_POINT('Origin',(-0.461880215351701,5.55111512312578E-17,
0.));
#54540=CARTESIAN_POINT('',(-0.23094010767585,0.4,0.));
#54541=CARTESIAN_POINT('',(-0.23094010767585,0.4,0.));
#54542=CARTESIAN_POINT('',(-0.461880215351701,5.6564012731995E-17,0.));
#54543=CARTESIAN_POINT('',(-0.404145188432738,0.1,0.));
#54544=CARTESIAN_POINT('',(-0.461880215351701,5.6564012731995E-17,0.));
#54545=CARTESIAN_POINT('Origin',(-0.461880215351701,5.55111512312578E-17,
0.));
#54546=CARTESIAN_POINT('',(-0.461880215351701,5.55111512312578E-17,-0.6));
#54547=CARTESIAN_POINT('',(-0.461880215351701,5.6564012731995E-17,0.));
#54548=CARTESIAN_POINT('',(-0.23094010767585,0.4,-0.6));
#54549=CARTESIAN_POINT('Origin',(-0.23094010767585,0.4,0.));
#54550=CARTESIAN_POINT('',(0.23094010767585,0.4,0.));
#54551=CARTESIAN_POINT('',(0.23094010767585,0.4,0.));
#54552=CARTESIAN_POINT('',(-0.115470053837925,0.4,0.));
#54553=CARTESIAN_POINT('Origin',(-0.23094010767585,0.4,0.));
#54554=CARTESIAN_POINT('',(0.23094010767585,0.4,-0.6));
#54555=CARTESIAN_POINT('',(0.23094010767585,0.4,-0.6));
#54556=CARTESIAN_POINT('',(0.23094010767585,0.4,0.));
#54557=CARTESIAN_POINT('Origin',(-0.23094010767585,0.4,0.));
#54558=CARTESIAN_POINT('',(-0.23094010767585,0.4,-0.6));
#54559=CARTESIAN_POINT('',(-0.23094010767585,0.4,0.));
#54560=CARTESIAN_POINT('',(0.23094010767585,0.4,-0.6));
#54561=CARTESIAN_POINT('Origin',(-0.230940107675851,-0.4,0.));
#54562=CARTESIAN_POINT('',(-0.230940107675851,-0.4,0.));
#54563=CARTESIAN_POINT('',(-0.288675134594813,-0.3,0.));
#54564=CARTESIAN_POINT('',(-0.230940107675851,-0.4,0.));
#54565=CARTESIAN_POINT('Origin',(-0.230940107675851,-0.4,0.));
#54566=CARTESIAN_POINT('',(-0.230940107675851,-0.4,-0.6));
#54567=CARTESIAN_POINT('',(-0.230940107675851,-0.4,0.));
#54568=CARTESIAN_POINT('',(-0.461880215351701,5.6564012731995E-17,-0.6));
#54569=CARTESIAN_POINT('Origin',(0.23094010767585,0.4,0.));
#54570=CARTESIAN_POINT('',(0.461880215351701,0.,0.));
#54571=CARTESIAN_POINT('',(0.461880215351701,0.,0.));
#54572=CARTESIAN_POINT('',(0.288675134594813,0.3,0.));
#54573=CARTESIAN_POINT('Origin',(0.23094010767585,0.4,0.));
#54574=CARTESIAN_POINT('',(0.461880215351701,0.,-0.6));
#54575=CARTESIAN_POINT('',(0.461880215351701,0.,-0.6));
#54576=CARTESIAN_POINT('',(0.461880215351701,0.,0.));
#54577=CARTESIAN_POINT('Origin',(0.23094010767585,0.4,0.));
#54578=CARTESIAN_POINT('',(0.461880215351701,0.,-0.6));
#54579=CARTESIAN_POINT('Origin',(0.,0.,-0.6));
#54580=CARTESIAN_POINT('',(-0.23094010767585,0.4,-0.6));
#54581=CARTESIAN_POINT('Origin',(0.,0.,-0.6));
#54582=CARTESIAN_POINT('Origin',(0.,0.,-0.6));
#54583=CARTESIAN_POINT('',(0.23094010767585,-0.4,-0.6));
#54584=CARTESIAN_POINT('Origin',(0.,0.,-0.6));
#54585=CARTESIAN_POINT('',(0.23094010767585,-0.4,-0.6));
#54586=CARTESIAN_POINT('',(-0.230940107675851,-0.4,-0.6));
#54587=CARTESIAN_POINT('',(0.23094010767585,-0.4,-0.6));
#54588=CARTESIAN_POINT('Origin',(0.,0.,-0.6));
#54589=CARTESIAN_POINT('',(-0.230940107675851,-0.4,-0.6));
#54590=CARTESIAN_POINT('Origin',(0.,0.,-0.6));
#54591=CARTESIAN_POINT('',(-0.461880215351701,5.6564012731995E-17,-0.6));
#54592=CARTESIAN_POINT('Origin',(0.461880215351701,0.,0.));
#54593=CARTESIAN_POINT('',(0.23094010767585,-0.4,0.));
#54594=CARTESIAN_POINT('',(0.23094010767585,-0.4,0.));
#54595=CARTESIAN_POINT('',(0.404145188432738,-0.1,0.));
#54596=CARTESIAN_POINT('Origin',(0.461880215351701,0.,0.));
#54597=CARTESIAN_POINT('',(0.23094010767585,-0.4,0.));
#54598=CARTESIAN_POINT('Origin',(0.461880215351701,0.,0.));
#54599=CARTESIAN_POINT('Origin',(0.23094010767585,-0.4,0.));
#54600=CARTESIAN_POINT('Origin',(0.23094010767585,-0.4,0.));
#54601=CARTESIAN_POINT('',(0.115470053837925,-0.4,0.));
#54602=CARTESIAN_POINT('Origin',(-0.461880215351701,5.55111512312578E-17,
0.));
#54603=CARTESIAN_POINT('Origin',(-0.230940107675851,-0.4,0.));
#54604=CARTESIAN_POINT('Origin',(0.23094010767585,-0.4,0.));
#54605=CARTESIAN_POINT('Origin',(0.6,0.,-6.));
#54606=CARTESIAN_POINT('',(-0.6,-7.34788079488412E-17,-6.));
#54607=CARTESIAN_POINT('Origin',(0.,0.,-6.));
#54608=CARTESIAN_POINT('Origin',(0.,0.,-5.9));
#54609=CARTESIAN_POINT('',(-0.7,-8.57252759403147E-17,-5.9));
#54610=CARTESIAN_POINT('Origin',(0.,0.,-2.94));
#54611=CARTESIAN_POINT('Origin',(0.,0.,-0.0711000000000004));
#54612=CARTESIAN_POINT('Origin',(0.,0.,-0.04));
#54613=CARTESIAN_POINT('',(-0.72,-8.81745695386094E-17,-6.93889390390723E-18));
#54614=CARTESIAN_POINT('Origin',(0.,0.,0.));
#54615=CARTESIAN_POINT('',(-0.76,-9.30731567351988E-17,-0.04));
#54616=CARTESIAN_POINT('Origin',(0.,0.,0.));
#54617=CARTESIAN_POINT('',(0.,0.,0.));
#54618=CARTESIAN_POINT('Origin',(0.,0.,0.04));
#54619=CARTESIAN_POINT('',(-0.805,-9.85840673313619E-17,0.08));
#54620=CARTESIAN_POINT('Origin',(0.,0.,0.08));
#54621=CARTESIAN_POINT('',(-0.885,1.08381241724541E-16,0.));
#54622=CARTESIAN_POINT('',(-0.845,-1.03482654527951E-16,0.04));
#54623=CARTESIAN_POINT('Origin',(0.,0.,0.));
#54624=CARTESIAN_POINT('Origin',(0.,0.,0.));
#54625=CARTESIAN_POINT('',(-0.805,9.85840673313619E-17,0.72));
#54626=CARTESIAN_POINT('Origin',(0.,0.,0.72));
#54627=CARTESIAN_POINT('',(-0.805,-9.85840673313619E-17,0.));
#54628=CARTESIAN_POINT('Origin',(0.,0.,0.));
#54629=CARTESIAN_POINT('',(-1.14,-1.39609735102798E-16,-8.32667268468867E-17));
#54630=CARTESIAN_POINT('Origin',(0.,0.,0.));
#54631=CARTESIAN_POINT('Origin',(0.,0.,0.76));
#54632=CARTESIAN_POINT('',(-0.885,-1.08381241724541E-16,0.8));
#54633=CARTESIAN_POINT('Origin',(0.,0.,0.8));
#54634=CARTESIAN_POINT('',(-0.845,-1.03482654527951E-16,0.76));
#54635=CARTESIAN_POINT('Origin',(0.,0.,0.8));
#54636=CARTESIAN_POINT('',(-1.14,-1.39609735102798E-16,0.8));
#54637=CARTESIAN_POINT('Origin',(0.,0.,0.8));
#54638=CARTESIAN_POINT('Origin',(0.,0.,0.085344103291654));
#54639=CARTESIAN_POINT('',(-1.2,-1.36663997456004E-16,0.0346410161513778));
#54640=CARTESIAN_POINT('',(-1.28782032302755,-1.5771250364726E-16,0.085344103291654));
#54641=CARTESIAN_POINT('',(-1.2,0.692820323027551,0.141820693123827));
#54642=CARTESIAN_POINT('Ctrl Pts',(-1.2,0.692820323027551,0.141820693123827));
#54643=CARTESIAN_POINT('Ctrl Pts',(-1.2,0.321539030917347,0.0346410161513777));
#54644=CARTESIAN_POINT('Ctrl Pts',(-1.2,-1.26370379014326E-16,0.0346410161513778));
#54645=CARTESIAN_POINT('',(8.48460190979925E-17,1.3856406460551,0.141820693123827));
#54646=CARTESIAN_POINT('Ctrl Pts',(8.48460190979925E-17,1.3856406460551,
0.141820693123827));
#54647=CARTESIAN_POINT('Ctrl Pts',(-0.599999999999999,1.03923048454133,
-0.0581793068761738));
#54648=CARTESIAN_POINT('Ctrl Pts',(-1.2,0.692820323027551,0.141820693123827));
#54649=CARTESIAN_POINT('',(1.2,0.692820323027551,0.141820693123827));
#54650=CARTESIAN_POINT('Ctrl Pts',(1.2,0.692820323027551,0.141820693123827));
#54651=CARTESIAN_POINT('Ctrl Pts',(0.6,1.03923048454133,-0.0581793068761734));
#54652=CARTESIAN_POINT('Ctrl Pts',(8.48460190979925E-17,1.3856406460551,
0.141820693123827));
#54653=CARTESIAN_POINT('',(1.2,-0.692820323027552,0.141820693123827));
#54654=CARTESIAN_POINT('Ctrl Pts',(1.2,-0.692820323027552,0.141820693123827));
#54655=CARTESIAN_POINT('Ctrl Pts',(1.2,-9.99200722162641E-16,-0.0581793068761738));
#54656=CARTESIAN_POINT('Ctrl Pts',(1.2,0.692820323027551,0.141820693123827));
#54657=CARTESIAN_POINT('',(-2.54538057293978E-16,-1.3856406460551,0.141820693123827));
#54658=CARTESIAN_POINT('Ctrl Pts',(-2.54538057293978E-16,-1.3856406460551,
0.141820693123827));
#54659=CARTESIAN_POINT('Ctrl Pts',(0.6,-1.03923048454133,-0.0581793068761735));
#54660=CARTESIAN_POINT('Ctrl Pts',(1.2,-0.692820323027551,0.141820693123827));
#54661=CARTESIAN_POINT('',(-1.2,-0.692820323027551,0.141820693123827));
#54662=CARTESIAN_POINT('Ctrl Pts',(-1.2,-0.692820323027551,0.141820693123827));
#54663=CARTESIAN_POINT('Ctrl Pts',(-0.6,-1.03923048454133,-0.0581793068761732));
#54664=CARTESIAN_POINT('Ctrl Pts',(-2.54538057293978E-16,-1.3856406460551,
0.141820693123827));
#54665=CARTESIAN_POINT('Ctrl Pts',(-1.2,-1.26370379014326E-16,0.0346410161513778));
#54666=CARTESIAN_POINT('Ctrl Pts',(-1.2,-0.321539030917348,0.0346410161513778));
#54667=CARTESIAN_POINT('Ctrl Pts',(-1.2,-0.692820323027551,0.141820693123827));
#54668=CARTESIAN_POINT('Origin',(-2.54538057293978E-16,-1.3856406460551,
0.));
#54669=CARTESIAN_POINT('',(1.2,-0.692820323027552,0.658179306876173));
#54670=CARTESIAN_POINT('',(1.2,-0.692820323027552,0.));
#54671=CARTESIAN_POINT('',(-2.54538057293978E-16,-1.3856406460551,0.658179306876173));
#54672=CARTESIAN_POINT('Ctrl Pts',(1.2,-0.692820323027552,0.658179306876173));
#54673=CARTESIAN_POINT('Ctrl Pts',(0.6,-1.03923048454133,0.858179306876173));
#54674=CARTESIAN_POINT('Ctrl Pts',(-2.54538057293978E-16,-1.3856406460551,
0.658179306876173));
#54675=CARTESIAN_POINT('',(-2.54538057293978E-16,-1.3856406460551,0.));
#54676=CARTESIAN_POINT('Origin',(1.2,-0.692820323027552,0.));
#54677=CARTESIAN_POINT('',(1.2,0.692820323027551,0.658179306876173));
#54678=CARTESIAN_POINT('',(1.2,0.692820323027551,0.));
#54679=CARTESIAN_POINT('Ctrl Pts',(1.2,0.692820323027551,0.658179306876173));
#54680=CARTESIAN_POINT('Ctrl Pts',(1.2,-3.33066907387547E-16,0.858179306876173));
#54681=CARTESIAN_POINT('Ctrl Pts',(1.2,-0.692820323027552,0.658179306876173));
#54682=CARTESIAN_POINT('Origin',(1.2,0.692820323027551,0.));
#54683=CARTESIAN_POINT('',(8.48460190979925E-17,1.3856406460551,0.658179306876173));
#54684=CARTESIAN_POINT('',(8.48460190979926E-17,1.3856406460551,0.));
#54685=CARTESIAN_POINT('Ctrl Pts',(8.48460190979925E-17,1.3856406460551,
0.658179306876173));
#54686=CARTESIAN_POINT('Ctrl Pts',(0.6,1.03923048454133,0.858179306876174));
#54687=CARTESIAN_POINT('Ctrl Pts',(1.2,0.692820323027551,0.658179306876173));
#54688=CARTESIAN_POINT('Origin',(0.,0.,0.714655896708346));
#54689=CARTESIAN_POINT('',(-1.2,0.692820323027551,0.658179306876173));
#54690=CARTESIAN_POINT('Ctrl Pts',(-1.2,0.692820323027551,0.658179306876173));
#54691=CARTESIAN_POINT('Ctrl Pts',(-0.6,1.03923048454133,0.858179306876173));
#54692=CARTESIAN_POINT('Ctrl Pts',(8.48460190979925E-17,1.3856406460551,
0.658179306876173));
#54693=CARTESIAN_POINT('',(-1.2,-2.29306563431106E-17,0.765358983848622));
#54694=CARTESIAN_POINT('Ctrl Pts',(-1.2,1.01096303211461E-16,0.765358983848622));
#54695=CARTESIAN_POINT('Ctrl Pts',(-1.2,0.321539030917348,0.765358983848622));
#54696=CARTESIAN_POINT('Ctrl Pts',(-1.2,0.692820323027551,0.658179306876173));
#54697=CARTESIAN_POINT('',(-1.28782032302755,-1.5771250364726E-16,0.714655896708346));
#54698=CARTESIAN_POINT('',(-1.2,-0.692820323027551,0.658179306876173));
#54699=CARTESIAN_POINT('Ctrl Pts',(-1.2,-0.692820323027551,0.658179306876173));
#54700=CARTESIAN_POINT('Ctrl Pts',(-1.2,-0.321539030917348,0.765358983848622));
#54701=CARTESIAN_POINT('Ctrl Pts',(-1.2,1.01096303211461E-16,0.765358983848622));
#54702=CARTESIAN_POINT('Ctrl Pts',(-2.54538057293978E-16,-1.3856406460551,
0.658179306876173));
#54703=CARTESIAN_POINT('Ctrl Pts',(-0.6,-1.03923048454133,0.858179306876173));
#54704=CARTESIAN_POINT('Ctrl Pts',(-1.2,-0.692820323027551,0.658179306876173));
#54705=CARTESIAN_POINT('Origin',(8.48460190979926E-17,1.3856406460551,0.));
#54706=CARTESIAN_POINT('',(-1.2,0.692820323027551,0.));
#54707=CARTESIAN_POINT('Origin',(-1.2,-0.692820323027551,0.));
#54708=CARTESIAN_POINT('',(-1.2,-0.692820323027551,0.));
#54709=CARTESIAN_POINT('Origin',(-1.2,0.692820323027551,0.));
#54710=CARTESIAN_POINT('',(0.,0.,0.));
#54711=CARTESIAN_POINT('Origin',(0.,0.,-1.94));
#54712=CARTESIAN_POINT('',(-0.791104428578755,2.03359169429485E-5,-3.7446668491763));
#54713=CARTESIAN_POINT('',(-0.791090383745199,1.30219247384927E-5,-3.77313315082371));
#54714=CARTESIAN_POINT('',(-0.7911,-9.68818082805471E-17,-1.94));
#54715=CARTESIAN_POINT('',(0.342081771909262,0.713331083684022,-3.8089));
#54716=CARTESIAN_POINT('Ctrl Pts',(-0.791104428578755,2.03359169429485E-5,
-3.7446668491763));
#54717=CARTESIAN_POINT('Ctrl Pts',(-0.791134076001446,0.0289074239465487,
-3.74582920226268));
#54718=CARTESIAN_POINT('Ctrl Pts',(-0.789582317070316,0.0577913339263522,
-3.74699155534907));
#54719=CARTESIAN_POINT('Ctrl Pts',(-0.786424813073281,0.0864986137826184,
-3.74815390843545));
#54720=CARTESIAN_POINT('Ctrl Pts',(-0.772073336273596,0.216978847925223,
-3.75343703186711));
#54721=CARTESIAN_POINT('Ctrl Pts',(-0.724549072123798,0.343810113341632,
-3.75872015529877));
#54722=CARTESIAN_POINT('Ctrl Pts',(-0.649622613351398,0.451592994815809,
-3.76400327873043));
#54723=CARTESIAN_POINT('Ctrl Pts',(-0.574696154578998,0.559375876289986,
-3.76928640216209));
#54724=CARTESIAN_POINT('Ctrl Pts',(-0.472367501183996,0.648110373821931,
-3.77456952559375));
#54725=CARTESIAN_POINT('Ctrl Pts',(-0.355061677451252,0.707020342729974,
-3.77985264902541));
#54726=CARTESIAN_POINT('Ctrl Pts',(-0.237755853718509,0.765930311638017,
-3.78513577245707));
#54727=CARTESIAN_POINT('Ctrl Pts',(-0.105472859648023,0.795015751922158,
-3.79041889588873));
#54728=CARTESIAN_POINT('Ctrl Pts',(0.0257249193947987,0.790748341450471,
-3.79570201932039));
#54729=CARTESIAN_POINT('Ctrl Pts',(0.134975048629466,0.787194812199209,
-3.8001013462136));
#54730=CARTESIAN_POINT('Ctrl Pts',(0.243472677435947,0.760514037346664,
-3.8045006731068));
#54731=CARTESIAN_POINT('Ctrl Pts',(0.342095581308745,0.713339856610551,
-3.8089));
#54732=CARTESIAN_POINT('',(-0.342067962509748,0.713322310757507,-3.8089));
#54733=CARTESIAN_POINT('Origin',(0.,0.,-3.8089));
#54734=CARTESIAN_POINT('Ctrl Pts',(-0.342067962509747,0.713322310757508,
-3.8089));
#54735=CARTESIAN_POINT('Ctrl Pts',(-0.460461074940846,0.65654784831081,
-3.80361687656834));
#54736=CARTESIAN_POINT('Ctrl Pts',(-0.564388400447012,0.569759817632143,
-3.79833375313668));
#54737=CARTESIAN_POINT('Ctrl Pts',(-0.641269208406438,0.463381943464528,
-3.79305062970502));
#54738=CARTESIAN_POINT('Ctrl Pts',(-0.718150016365868,0.357004069296908,
-3.78776750627336));
#54739=CARTESIAN_POINT('Ctrl Pts',(-0.767984306778557,0.231036351640338,
-3.7824843828417));
#54740=CARTESIAN_POINT('Ctrl Pts',(-0.784715742391765,0.100833355385061,
-3.77720125941004));
#54741=CARTESIAN_POINT('Ctrl Pts',(-0.789010253505645,0.0674137357298711,
-3.7758452232146));
#54742=CARTESIAN_POINT('Ctrl Pts',(-0.791123911091846,0.0337150911286863,
-3.77448918701915));
#54743=CARTESIAN_POINT('Ctrl Pts',(-0.791090383745199,1.30219247384927E-5,
-3.77313315082371));
#54744=CARTESIAN_POINT('Origin',(0.,0.,-1.94));
#54745=CARTESIAN_POINT('',(-0.791128448098422,-1.786362598305E-5,-3.5446668491763));
#54746=CARTESIAN_POINT('',(-0.791142152082714,-1.50645020713617E-5,-3.57313315082371));
#54747=CARTESIAN_POINT('',(-0.7911,-9.68818082805471E-17,-1.94));
#54748=CARTESIAN_POINT('Ctrl Pts',(-0.791128448098422,-1.786362598305E-5,
-3.5446668491763));
#54749=CARTESIAN_POINT('Ctrl Pts',(-0.791020967662586,0.110106180651968,
-3.54909838774943));
#54750=CARTESIAN_POINT('Ctrl Pts',(-0.767821030540255,0.220274089461432,
-3.55352992632255));
#54751=CARTESIAN_POINT('Ctrl Pts',(-0.723158334650058,0.320917426638007,
-3.55796146489568));
#54752=CARTESIAN_POINT('Ctrl Pts',(-0.669913049455132,0.440900850928166,
-3.56324458832734));
#54753=CARTESIAN_POINT('Ctrl Pts',(-0.586163680035589,0.547347416399969,
-3.56852771175901));
#54754=CARTESIAN_POINT('Ctrl Pts',(-0.482079359508604,0.627332019525317,
-3.57381083519067));
#54755=CARTESIAN_POINT('Ctrl Pts',(-0.37799503898162,0.707316622650663,
-3.57909395862233));
#54756=CARTESIAN_POINT('Ctrl Pts',(-0.253575767347198,0.760839263429553,
-3.58437708205399));
#54757=CARTESIAN_POINT('Ctrl Pts',(-0.123928955457381,0.781401040356963,
-3.58966020548565));
#54758=CARTESIAN_POINT('Ctrl Pts',(0.00571785643243594,0.801962817284373,
-3.59494332891731));
#54759=CARTESIAN_POINT('Ctrl Pts',(0.140592208577647,0.789563730360299,
-3.60022645234897));
#54760=CARTESIAN_POINT('Ctrl Pts',(0.264317198649155,0.745709319909767,
-3.60550957578063));
#54761=CARTESIAN_POINT('Ctrl Pts',(0.388042188720661,0.701854909459236,
-3.61079269921229));
#54762=CARTESIAN_POINT('Ctrl Pts',(0.500617816718466,0.626545175482247,
-3.61607582264395));
#54763=CARTESIAN_POINT('Ctrl Pts',(0.588374767319508,0.528924479815501,
-3.62135894607561));
#54764=CARTESIAN_POINT('Ctrl Pts',(0.67613171792055,0.431303784148756,-3.62664206950727));
#54765=CARTESIAN_POINT('Ctrl Pts',(0.739069991124828,0.311372126792253,
-3.63192519293893));
#54766=CARTESIAN_POINT('Ctrl Pts',(0.76954740770552,0.183692021249386,-3.63720831637059));
#54767=CARTESIAN_POINT('Ctrl Pts',(0.800024824286212,0.0560119157065181,
-3.64249143980225));
#54768=CARTESIAN_POINT('Ctrl Pts',(0.798041384243317,-0.0794166380227145,
-3.64777456323391));
#54769=CARTESIAN_POINT('Ctrl Pts',(0.763837923925609,-0.206149452463652,
-3.65305768666557));
#54770=CARTESIAN_POINT('Ctrl Pts',(0.729634463607901,-0.33288226690459,
-3.65834081009723));
#54771=CARTESIAN_POINT('Ctrl Pts',(0.66321098301538,-0.450919342057233,
-3.66362393352889));
#54772=CARTESIAN_POINT('Ctrl Pts',(0.572632846320033,-0.54592819965897,
-3.66890705696055));
#54773=CARTESIAN_POINT('Ctrl Pts',(0.482054709624687,-0.640937057260705,
-3.67419018039221));
#54774=CARTESIAN_POINT('Ctrl Pts',(0.367321916826515,-0.712917697311535,
-3.67947330382387));
#54775=CARTESIAN_POINT('Ctrl Pts',(0.242365714829211,-0.753130015950053,
-3.68475642725553));
#54776=CARTESIAN_POINT('Ctrl Pts',(0.117409512831907,-0.793342334588571,
-3.69003955068719));
#54777=CARTESIAN_POINT('Ctrl Pts',(-0.0177700983645308,-0.801786331814778,
-3.69532267411885));
#54778=CARTESIAN_POINT('Ctrl Pts',(-0.146759153262384,-0.777436649787474,
-3.70060579755051));
#54779=CARTESIAN_POINT('Ctrl Pts',(-0.275748208160238,-0.753086967760169,
-3.70588892098217));
#54780=CARTESIAN_POINT('Ctrl Pts',(-0.398546706759508,-0.695943606479353,
-3.71117204441383));
#54781=CARTESIAN_POINT('Ctrl Pts',(-0.500244033294698,-0.612945222655453,
-3.71645516784549));
#54782=CARTESIAN_POINT('Ctrl Pts',(-0.601941359829888,-0.529946838831553,
-3.72173829127715));
#54783=CARTESIAN_POINT('Ctrl Pts',(-0.682537514300998,-0.421093432464569,
-3.72702141470881));
#54784=CARTESIAN_POINT('Ctrl Pts',(-0.732246246811768,-0.299602127846677,
-3.73230453814047));
#54785=CARTESIAN_POINT('Ctrl Pts',(-0.771018437823636,-0.20484042641111,
-3.73642530848574));
#54786=CARTESIAN_POINT('Ctrl Pts',(-0.790999322633179,-0.10239007371512,
-3.74054607883102));
#54787=CARTESIAN_POINT('Ctrl Pts',(-0.791104428578755,2.03359169429485E-5,
-3.7446668491763));
#54788=CARTESIAN_POINT('Ctrl Pts',(-0.791090383745199,1.30219247384927E-5,
-3.77313315082371));
#54789=CARTESIAN_POINT('Ctrl Pts',(-0.790993288390722,-0.0975883299045687,
-3.76920606358749));
#54790=CARTESIAN_POINT('Ctrl Pts',(-0.772888089260372,-0.195218403340946,
-3.76527897635128));
#54791=CARTESIAN_POINT('Ctrl Pts',(-0.737592540570363,-0.286183324054275,
-3.76135188911506));
#54792=CARTESIAN_POINT('Ctrl Pts',(-0.690109322322024,-0.408558732384351,
-3.7560687656834));
#54793=CARTESIAN_POINT('Ctrl Pts',(-0.611514305011616,-0.518871274190519,
-3.75078564225174));
#54794=CARTESIAN_POINT('Ctrl Pts',(-0.511349099416939,-0.603713633894183,
-3.74550251882008));
#54795=CARTESIAN_POINT('Ctrl Pts',(-0.411183893822262,-0.688555993597846,
-3.74021939538842));
#54796=CARTESIAN_POINT('Ctrl Pts',(-0.289448499943316,-0.747928171199005,
-3.73493627195676));
#54797=CARTESIAN_POINT('Ctrl Pts',(-0.160925296224211,-0.774627492756042,
-3.7296531485251));
#54798=CARTESIAN_POINT('Ctrl Pts',(-0.0324020925051069,-0.80132681431308,
-3.72437002509344));
#54799=CARTESIAN_POINT('Ctrl Pts',(0.102908921054156,-0.795353279825997,
-3.71908690166178));
#54800=CARTESIAN_POINT('Ctrl Pts',(0.228578257335151,-0.75742890064077,
-3.71380377823012));
#54801=CARTESIAN_POINT('Ctrl Pts',(0.354247593616146,-0.719504521455543,
-3.70852065479846));
#54802=CARTESIAN_POINT('Ctrl Pts',(0.470275252618875,-0.649629297572173,
-3.7032375313668));
#54803=CARTESIAN_POINT('Ctrl Pts',(0.562572538830204,-0.556289409358392,
-3.69795440793514));
#54804=CARTESIAN_POINT('Ctrl Pts',(0.654869825041534,-0.462949521144612,
-3.69267128450348));
#54805=CARTESIAN_POINT('Ctrl Pts',(0.723436738461466,-0.34614496860042,
-3.68738816107182));
#54806=CARTESIAN_POINT('Ctrl Pts',(0.759947765185156,-0.220057692724725,
-3.68210503764016));
#54807=CARTESIAN_POINT('Ctrl Pts',(0.796458791908846,-0.0939704168490289,
-3.6768219142085));
#54808=CARTESIAN_POINT('Ctrl Pts',(0.800913931936294,0.0413995823581705,
-3.67153879077684));
#54809=CARTESIAN_POINT('Ctrl Pts',(0.77277216890208,0.16961477774449,-3.66625566734518));
#54810=CARTESIAN_POINT('Ctrl Pts',(0.744630405867867,0.297829973130809,
-3.66097254391352));
#54811=CARTESIAN_POINT('Ctrl Pts',(0.683891739771991,0.418890364696249,
-3.65568942048186));
#54812=CARTESIAN_POINT('Ctrl Pts',(0.597931295593872,0.518096613818281,
-3.6504062970502));
#54813=CARTESIAN_POINT('Ctrl Pts',(0.511970851415752,0.617302862940314,
-3.64512317361854));
#54814=CARTESIAN_POINT('Ctrl Pts',(0.400788629155388,0.694654969618939,
-3.63984005018688));
#54815=CARTESIAN_POINT('Ctrl Pts',(0.277884736994597,0.740760462896105,
-3.63455692675522));
#54816=CARTESIAN_POINT('Ctrl Pts',(0.154980844833807,0.786865956173271,
-3.62927380332356));
#54817=CARTESIAN_POINT('Ctrl Pts',(0.0203552827725882,0.801724836048977,
-3.6239906798919));
#54818=CARTESIAN_POINT('Ctrl Pts',(-0.109645248094981,0.783532945683037,
-3.61870755646024));
#54819=CARTESIAN_POINT('Ctrl Pts',(-0.239645778962551,0.765341055317096,
-3.61342443302858));
#54820=CARTESIAN_POINT('Ctrl Pts',(-0.365021278636471,0.714098394709508,
-3.60814130959692));
#54821=CARTESIAN_POINT('Ctrl Pts',(-0.470548231740154,0.636026991824806,
-3.60285818616526));
#54822=CARTESIAN_POINT('Ctrl Pts',(-0.576075184843836,0.557955588940104,
-3.5975750627336));
#54823=CARTESIAN_POINT('Ctrl Pts',(-0.66175359137728,0.453055443778288,
-3.59229193930193));
#54824=CARTESIAN_POINT('Ctrl Pts',(-0.717180085970426,0.334063903885682,
-3.58700881587028));
#54825=CARTESIAN_POINT('Ctrl Pts',(-0.765704378063189,0.229890254068931,
-3.58238359418809));
#54826=CARTESIAN_POINT('Ctrl Pts',(-0.791042104935038,0.114916260669801,
-3.5777583725059));
#54827=CARTESIAN_POINT('Ctrl Pts',(-0.791142152082714,-1.50645020713617E-5,
-3.57313315082371));
#54828=CARTESIAN_POINT('Origin',(0.,0.,-1.94));
#54829=CARTESIAN_POINT('',(-0.791034765442454,5.10246101870227E-6,-3.3446668491763));
#54830=CARTESIAN_POINT('',(-0.791032851165218,6.96852469137922E-7,-3.3731331508237));
#54831=CARTESIAN_POINT('',(-0.7911,-9.68818082805471E-17,-1.94));
#54832=CARTESIAN_POINT('Ctrl Pts',(-0.791034765442454,5.10246101870227E-6,
-3.3446668491763));
#54833=CARTESIAN_POINT('Ctrl Pts',(-0.791048344631556,0.0601030927221048,
-3.34708444980451));
#54834=CARTESIAN_POINT('Ctrl Pts',(-0.784287366750522,0.120198076074771,
-3.34950205043273));
#54835=CARTESIAN_POINT('Ctrl Pts',(-0.770718569515641,0.178714460170998,
-3.35191965106094));
#54836=CARTESIAN_POINT('Ctrl Pts',(-0.74106700929745,0.306588880928024,
-3.3572027744926));
#54837=CARTESIAN_POINT('Ctrl Pts',(-0.678905190912391,0.426924812970615,
-3.36248589792426));
#54838=CARTESIAN_POINT('Ctrl Pts',(-0.591781013642106,0.525110658398002,
-3.36776902135592));
#54839=CARTESIAN_POINT('Ctrl Pts',(-0.50465683637182,0.623296503825389,
-3.37305214478758));
#54840=CARTESIAN_POINT('Ctrl Pts',(-0.392570300216308,0.699332262637573,
-3.37833526821924));
#54841=CARTESIAN_POINT('Ctrl Pts',(-0.269131333387287,0.743985414547624,
-3.3836183916509));
#54842=CARTESIAN_POINT('Ctrl Pts',(-0.145692366558263,0.788638566457676,
-3.38890151508256));
#54843=CARTESIAN_POINT('Ctrl Pts',(-0.0109009690557307,0.801909111465594,
-3.39418463851422));
#54844=CARTESIAN_POINT('Ctrl Pts',(0.118876029468087,0.782185694888634,
-3.39946776194588));
#54845=CARTESIAN_POINT('Ctrl Pts',(0.248653027991902,0.762462278311674,
-3.40475088537754));
#54846=CARTESIAN_POINT('Ctrl Pts',(0.373415627537002,0.709744900149836,
-3.4100340088092));
#54847=CARTESIAN_POINT('Ctrl Pts',(0.478014729187874,0.630434683650731,
-3.41531713224086));
#54848=CARTESIAN_POINT('Ctrl Pts',(0.582613830838747,0.551124467151625,
-3.42060025567252));
#54849=CARTESIAN_POINT('Ctrl Pts',(0.667049434595391,0.445221412315251,
-3.42588337910418));
#54850=CARTESIAN_POINT('Ctrl Pts',(0.721069082445871,0.325584628032729,
-3.43116650253584));
#54851=CARTESIAN_POINT('Ctrl Pts',(0.77508873029635,0.205947843750209,-3.4364496259675));
#54852=CARTESIAN_POINT('Ctrl Pts',(0.798692422240667,0.0725773300215417,
-3.44173274939916));
#54853=CARTESIAN_POINT('Ctrl Pts',(0.789014117771925,-0.0583326120373118,
-3.44701587283082));
#54854=CARTESIAN_POINT('Ctrl Pts',(0.779335813303183,-0.189242554096167,
-3.45229899626248));
#54855=CARTESIAN_POINT('Ctrl Pts',(0.736375512421381,-0.317691924485209,
-3.45758211969414));
#54856=CARTESIAN_POINT('Ctrl Pts',(0.665349600885421,-0.42808396404388,
-3.4628652431258));
#54857=CARTESIAN_POINT('Ctrl Pts',(0.594323689349462,-0.538476003602551,
-3.46814836655746));
#54858=CARTESIAN_POINT('Ctrl Pts',(0.495232167159344,-0.630810712330852,
-3.47343148998912));
#54859=CARTESIAN_POINT('Ctrl Pts',(0.380107063759745,-0.693876496036605,
-3.47871461342078));
#54860=CARTESIAN_POINT('Ctrl Pts',(0.264981960360147,-0.756942279742356,
-3.48399773685244));
#54861=CARTESIAN_POINT('Ctrl Pts',(0.13382327575107,-0.79073913842556,-3.4892808602841));
#54862=CARTESIAN_POINT('Ctrl Pts',(0.00255674323769956,-0.791163342635944,
-3.49456398371576));
#54863=CARTESIAN_POINT('Ctrl Pts',(-0.128709789275672,-0.791587546846327,
-3.49984710714743));
#54864=CARTESIAN_POINT('Ctrl Pts',(-0.260084169693336,-0.75863909658389,
-3.50513023057909));
#54865=CARTESIAN_POINT('Ctrl Pts',(-0.375614474192984,-0.69631870465558,
-3.51041335401075));
#54866=CARTESIAN_POINT('Ctrl Pts',(-0.491144778692633,-0.633998312727271,
-3.51569647744241));
#54867=CARTESIAN_POINT('Ctrl Pts',(-0.590831007274266,-0.542305979133088,
-3.52097960087406));
#54868=CARTESIAN_POINT('Ctrl Pts',(-0.662568919220032,-0.432375298724376,
-3.52626272430572));
#54869=CARTESIAN_POINT('Ctrl Pts',(-0.734306831165799,-0.322444618315663,
-3.53154584773739));
#54870=CARTESIAN_POINT('Ctrl Pts',(-0.778096426475699,-0.194275591092421,
-3.53682897116905));
#54871=CARTESIAN_POINT('Ctrl Pts',(-0.788620623645495,-0.0634309359265427,
-3.54211209460071));
#54872=CARTESIAN_POINT('Ctrl Pts',(-0.790317015386842,-0.0423401307238582,
-3.54296367945924));
#54873=CARTESIAN_POINT('Ctrl Pts',(-0.791149102033898,-0.0211798070728596,
-3.54381526431777));
#54874=CARTESIAN_POINT('Ctrl Pts',(-0.791128448098422,-1.786362598305E-5,
-3.5446668491763));
#54875=CARTESIAN_POINT('Ctrl Pts',(-0.791142152082714,-1.50645020713617E-5,
-3.57313315082371));
#54876=CARTESIAN_POINT('Ctrl Pts',(-0.791156383010009,-0.0163631500847965,
-3.57247524907424));
#54877=CARTESIAN_POINT('Ctrl Pts',(-0.790659983849077,-0.0327103723678489,
-3.57181734732477));
#54878=CARTESIAN_POINT('Ctrl Pts',(-0.789647051564748,-0.049025525545824,
-3.5711594455753));
#54879=CARTESIAN_POINT('Ctrl Pts',(-0.781512939913075,-0.18004048046133,
-3.56587632214364));
#54880=CARTESIAN_POINT('Ctrl Pts',(-0.740070133956881,-0.308987455668947,
-3.56059319871197));
#54881=CARTESIAN_POINT('Ctrl Pts',(-0.670350759535863,-0.420209267130899,
-3.55531007528031));
#54882=CARTESIAN_POINT('Ctrl Pts',(-0.600631385114846,-0.531431078592849,
-3.55002695184865));
#54883=CARTESIAN_POINT('Ctrl Pts',(-0.502635442229007,-0.624927726309134,
-3.544743828417));
#54884=CARTESIAN_POINT('Ctrl Pts',(-0.388261931629374,-0.689346531557255,
-3.53946070498534));
#54885=CARTESIAN_POINT('Ctrl Pts',(-0.273888421029741,-0.753765336805377,
-3.53417758155368));
#54886=CARTESIAN_POINT('Ctrl Pts',(-0.143137342716314,-0.789106299585334,
-3.52889445812201));
#54887=CARTESIAN_POINT('Ctrl Pts',(-0.011884936914468,-0.791078199024235,
-3.52361133469035));
#54888=CARTESIAN_POINT('Ctrl Pts',(0.119367468887379,-0.793050098463135,
-3.51832821125869));
#54889=CARTESIAN_POINT('Ctrl Pts',(0.251121202177644,-0.761652934560978,
-3.51304508782703));
#54890=CARTESIAN_POINT('Ctrl Pts',(0.367378276747785,-0.700699058214266,
-3.50776196439537));
#54891=CARTESIAN_POINT('Ctrl Pts',(0.483635351317926,-0.639745181867554,
-3.50247884096371));
#54892=CARTESIAN_POINT('Ctrl Pts',(0.584395767167944,-0.549234593076287,
-3.49719571753205));
#54893=CARTESIAN_POINT('Ctrl Pts',(0.657424852147946,-0.440157394912042,
-3.49191259410039));
#54894=CARTESIAN_POINT('Ctrl Pts',(0.730453937127948,-0.331080196747798,
-3.48662947066873));
#54895=CARTESIAN_POINT('Ctrl Pts',(0.775751691237936,-0.203436389210576,
-3.48134634723707));
#54896=CARTESIAN_POINT('Ctrl Pts',(0.787817907184613,-0.0727249174230299,
-3.47606322380541));
#54897=CARTESIAN_POINT('Ctrl Pts',(0.79988412313129,0.0579865543645165,
-3.47078010037375));
#54898=CARTESIAN_POINT('Ctrl Pts',(0.778718800914655,0.191765690402387,
-3.46549697694209));
#54899=CARTESIAN_POINT('Ctrl Pts',(0.726891905910353,0.312368573337293,
-3.46021385351043));
#54900=CARTESIAN_POINT('Ctrl Pts',(0.67506501090605,0.432971456272199,-3.45493073007877));
#54901=CARTESIAN_POINT('Ctrl Pts',(0.592576543114078,0.54039808610414,-3.44964760664711));
#54902=CARTESIAN_POINT('Ctrl Pts',(0.489442532674306,0.621604356250294,
-3.44436448321545));
#54903=CARTESIAN_POINT('Ctrl Pts',(0.386308522234534,0.702810626396448,
-3.43908135978379));
#54904=CARTESIAN_POINT('Ctrl Pts',(0.262528969146962,0.757796536856814,
-3.43379823635213));
#54905=CARTESIAN_POINT('Ctrl Pts',(0.133133607487199,0.779885511500048,
-3.42851511292047));
#54906=CARTESIAN_POINT('Ctrl Pts',(0.00373824582743582,0.801974486143282,
-3.42323198948881));
#54907=CARTESIAN_POINT('Ctrl Pts',(-0.131272924404518,0.791166524969384,
-3.41794886605715));
#54908=CARTESIAN_POINT('Ctrl Pts',(-0.255506388005845,0.748773967351791,
-3.41266574262549));
#54909=CARTESIAN_POINT('Ctrl Pts',(-0.379739851607171,0.706381409734199,
-3.40738261919383));
#54910=CARTESIAN_POINT('Ctrl Pts',(-0.493195608577871,0.632404255672914,
-3.40209949576217));
#54911=CARTESIAN_POINT('Ctrl Pts',(-0.582097475260115,0.535825062673564,
-3.39681637233051));
#54912=CARTESIAN_POINT('Ctrl Pts',(-0.670999341942359,0.439245869674214,
-3.39153324889885));
#54913=CARTESIAN_POINT('Ctrl Pts',(-0.735347318336148,0.3200646377368,-3.38625012546719));
#54914=CARTESIAN_POINT('Ctrl Pts',(-0.767328054423804,0.192752757147877,
-3.38096700203553));
#54915=CARTESIAN_POINT('Ctrl Pts',(-0.78313513845885,0.129826450836074,
-3.37835571829825));
#54916=CARTESIAN_POINT('Ctrl Pts',(-0.791034848401665,0.0649138126686076,
-3.37574443456098));
#54917=CARTESIAN_POINT('Ctrl Pts',(-0.791032851165218,6.96852469137922E-7,
-3.3731331508237));
#54918=CARTESIAN_POINT('Origin',(0.,0.,-1.94));
#54919=CARTESIAN_POINT('',(-0.791156898220181,1.00405986563634E-5,-3.1446668491763));
#54920=CARTESIAN_POINT('',(-0.791146063621827,1.39968631027903E-5,-3.17313315082371));
#54921=CARTESIAN_POINT('',(-0.7911,-9.68818082805471E-17,-1.94));
#54922=CARTESIAN_POINT('Ctrl Pts',(-0.791156898220181,1.00405986563634E-5,
-3.1446668491763));
#54923=CARTESIAN_POINT('Ctrl Pts',(-0.791163256457482,0.0100400424277527,
-3.1450705118596));
#54924=CARTESIAN_POINT('Ctrl Pts',(-0.790976464647033,0.0200698071486357,
-3.1454741745429));
#54925=CARTESIAN_POINT('Ctrl Pts',(-0.790594987006842,0.0300921616056704,
-3.1458778372262));
#54926=CARTESIAN_POINT('Ctrl Pts',(-0.78560222066274,0.161264394915736,
-3.15116096065786));
#54927=CARTESIAN_POINT('Ctrl Pts',(-0.747260774074463,0.291167288182243,
-3.15644408408952));
#54928=CARTESIAN_POINT('Ctrl Pts',(-0.68022619601261,0.404027590553744,
-3.16172720752118));
#54929=CARTESIAN_POINT('Ctrl Pts',(-0.613191617950758,0.516887892925243,
-3.16701033095284));
#54930=CARTESIAN_POINT('Ctrl Pts',(-0.517463908415333,0.612705604401734,
-3.1722934543845));
#54931=CARTESIAN_POINT('Ctrl Pts',(-0.404666651284786,0.679846212763156,
-3.17757657781616));
#54932=CARTESIAN_POINT('Ctrl Pts',(-0.291869394154238,0.74698682112458,
-3.18285970124782));
#54933=CARTESIAN_POINT('Ctrl Pts',(-0.162002589428568,0.785450326370933,
-3.18814282467948));
#54934=CARTESIAN_POINT('Ctrl Pts',(-0.0308351059659308,0.790566358954465,
-3.19342594811114));
#54935=CARTESIAN_POINT('Ctrl Pts',(0.100332377496707,0.795682391537996,
-3.1987090715428));
#54936=CARTESIAN_POINT('Ctrl Pts',(0.232800539696312,0.767450951458705,
-3.20399219497446));
#54937=CARTESIAN_POINT('Ctrl Pts',(0.350484646108009,0.709299996132096,
-3.20927531840612));
#54938=CARTESIAN_POINT('Ctrl Pts',(0.468168752519706,0.651149040805489,
-3.21455844183778));
#54939=CARTESIAN_POINT('Ctrl Pts',(0.571068803143495,0.563078570231564,
-3.21984156526944));
#54940=CARTESIAN_POINT('Ctrl Pts',(0.646690324066575,0.45578240030646,-3.2251246887011));
#54941=CARTESIAN_POINT('Ctrl Pts',(0.722311844989655,0.348486230381356,
-3.23040781213276));
#54942=CARTESIAN_POINT('Ctrl Pts',(0.770654836212026,0.221964361105069,
-3.23569093556442));
#54943=CARTESIAN_POINT('Ctrl Pts',(0.785849327417509,0.0915795079037739,
-3.24097405899608));
#54944=CARTESIAN_POINT('Ctrl Pts',(0.801043818622993,-0.0388053452975232,
-3.24625718242774));
#54945=CARTESIAN_POINT('Ctrl Pts',(0.783089809811589,-0.173053182423831,
-3.2515403058594));
#54946=CARTESIAN_POINT('Ctrl Pts',(0.734167337760388,-0.294863174771408,
-3.25682342929106));
#54947=CARTESIAN_POINT('Ctrl Pts',(0.685244865709187,-0.416673167118983,
-3.26210655272272));
#54948=CARTESIAN_POINT('Ctrl Pts',(0.605353930418191,-0.526045314687827,
-3.26738967615438));
#54949=CARTESIAN_POINT('Ctrl Pts',(0.504195160806543,-0.609699279554858,
-3.27267279958604));
#54950=CARTESIAN_POINT('Ctrl Pts',(0.403036391194895,-0.693353244421891,
-3.2779559230177));
#54951=CARTESIAN_POINT('Ctrl Pts',(0.280609787262598,-0.75128902658711,
-3.28323904644936));
#54952=CARTESIAN_POINT('Ctrl Pts',(0.151780803397594,-0.776471866451342,
-3.28852216988102));
#54953=CARTESIAN_POINT('Ctrl Pts',(0.0229518195325914,-0.801654706315574,
-3.29380529331268));
#54954=CARTESIAN_POINT('Ctrl Pts',(-0.112279544265117,-0.79408460387882,
-3.29908841674434));
#54955=CARTESIAN_POINT('Ctrl Pts',(-0.237493036140256,-0.754680746710377,
-3.304371540176));
#54956=CARTESIAN_POINT('Ctrl Pts',(-0.362706528015396,-0.715276889541934,
-3.30965466360766));
#54957=CARTESIAN_POINT('Ctrl Pts',(-0.477902147967967,-0.644039277641801,
-3.31493778703932));
#54958=CARTESIAN_POINT('Ctrl Pts',(-0.569092452263575,-0.549617823989616,
-3.32022091047098));
#54959=CARTESIAN_POINT('Ctrl Pts',(-0.660282756559183,-0.455196370337432,
-3.32550403390264));
#54960=CARTESIAN_POINT('Ctrl Pts',(-0.727467745197829,-0.337591074933195,
-3.3307871573343));
#54961=CARTESIAN_POINT('Ctrl Pts',(-0.762489588491491,-0.211081972495344,
-3.33607028076596));
#54962=CARTESIAN_POINT('Ctrl Pts',(-0.781485148953939,-0.142464473288981,
-3.33893580356941));
#54963=CARTESIAN_POINT('Ctrl Pts',(-0.791018670362246,-0.0712275732442067,
-3.34180132637285));
#54964=CARTESIAN_POINT('Ctrl Pts',(-0.791034765442454,5.10246101870227E-6,
-3.3446668491763));
#54965=CARTESIAN_POINT('Ctrl Pts',(-0.791032851165218,6.96852469137922E-7,
-3.3731331508237));
#54966=CARTESIAN_POINT('Ctrl Pts',(-0.791030807612638,-0.0664177612599439,
-3.37046131112932));
#54967=CARTESIAN_POINT('Ctrl Pts',(-0.78275632457385,-0.13283671943135,
-3.36778947143493));
#54968=CARTESIAN_POINT('Ctrl Pts',(-0.766215472424178,-0.19712893829106,
-3.36511763174055));
#54969=CARTESIAN_POINT('Ctrl Pts',(-0.733508658555371,-0.324256223900637,
-3.35983450830889));
#54970=CARTESIAN_POINT('Ctrl Pts',(-0.668481535036233,-0.443068265879359,
-3.35455138487723));
#54971=CARTESIAN_POINT('Ctrl Pts',(-0.579029916237292,-0.539138502238536,
-3.34926826144557));
#54972=CARTESIAN_POINT('Ctrl Pts',(-0.48957829743835,-0.635208738597713,
-3.34398513801391));
#54973=CARTESIAN_POINT('Ctrl Pts',(-0.375702183359603,-0.708537169337344,
-3.33870201458225));
#54974=CARTESIAN_POINT('Ctrl Pts',(-0.251228798847089,-0.750220007147094,
-3.33341889115059));
#54975=CARTESIAN_POINT('Ctrl Pts',(-0.126755414334578,-0.791902844956843,
-3.32813576771893));
#54976=CARTESIAN_POINT('Ctrl Pts',(0.00831524061170164,-0.801940089836712,
-3.32285264428727));
#54977=CARTESIAN_POINT('Ctrl Pts',(0.137582427951453,-0.779112985396101,
-3.31756952085561));
#54978=CARTESIAN_POINT('Ctrl Pts',(0.266849615291207,-0.756285880955491,
-3.31228639742395));
#54979=CARTESIAN_POINT('Ctrl Pts',(0.390313335024435,-0.700594427194401,
-3.30700327399229));
#54980=CARTESIAN_POINT('Ctrl Pts',(0.492982202637408,-0.618800869728425,
-3.30172015056063));
#54981=CARTESIAN_POINT('Ctrl Pts',(0.595651070250382,-0.537007312262449,
-3.29643702712897));
#54982=CARTESIAN_POINT('Ctrl Pts',(0.6775250857431,-0.42911165109159,-3.29115390369731));
#54983=CARTESIAN_POINT('Ctrl Pts',(0.728662827857662,-0.308214944141823,
-3.28587078026565));
#54984=CARTESIAN_POINT('Ctrl Pts',(0.779800569972224,-0.187318237192056,
-3.28058765683399));
#54985=CARTESIAN_POINT('Ctrl Pts',(0.800202038708627,-0.0534204844633812,
-3.27530453340233));
#54986=CARTESIAN_POINT('Ctrl Pts',(0.787390018386567,0.0772199937780057,
-3.27002140997067));
#54987=CARTESIAN_POINT('Ctrl Pts',(0.774577998064506,0.207860472019394,
-3.26473828653901));
#54988=CARTESIAN_POINT('Ctrl Pts',(0.728552488683982,0.335243675773492,
-3.25945516310735));
#54989=CARTESIAN_POINT('Ctrl Pts',(0.654902064038613,0.443902303454082,
-3.25417203967569));
#54990=CARTESIAN_POINT('Ctrl Pts',(0.581251639393244,0.552560931134673,
-3.24888891624403));
#54991=CARTESIAN_POINT('Ctrl Pts',(0.479976299483027,0.642494982741753,
-3.24360579281237));
#54992=CARTESIAN_POINT('Ctrl Pts',(0.363373240323399,0.70278436003567,-3.23832266938071));
#54993=CARTESIAN_POINT('Ctrl Pts',(0.246770181163772,0.763073737329586,
-3.23303954594905));
#54994=CARTESIAN_POINT('Ctrl Pts',(0.114839402754731,0.793718440310342,
-3.22775642251739));
#54995=CARTESIAN_POINT('Ctrl Pts',(-0.0163996113453126,0.790997484978048,
-3.22247329908573));
#54996=CARTESIAN_POINT('Ctrl Pts',(-0.147638625445356,0.788276529645754,
-3.21719017565407));
#54997=CARTESIAN_POINT('Ctrl Pts',(-0.278185875236402,0.752189916000409,
-3.21190705222241));
#54998=CARTESIAN_POINT('Ctrl Pts',(-0.392189869907569,0.687119403332316,
-3.20662392879075));
#54999=CARTESIAN_POINT('Ctrl Pts',(-0.506193864578736,0.622048890664222,
-3.20134080535909));
#55000=CARTESIAN_POINT('Ctrl Pts',(-0.603654604130024,0.52799447897338,
-3.19605768192743));
#55001=CARTESIAN_POINT('Ctrl Pts',(-0.672738074287734,0.416376574626269,
-3.19077455849577));
#55002=CARTESIAN_POINT('Ctrl Pts',(-0.741821544445445,0.304758670279158,
-3.18549143506411));
#55003=CARTESIAN_POINT('Ctrl Pts',(-0.782527745209579,0.17557727327578,
-3.18020831163244));
#55004=CARTESIAN_POINT('Ctrl Pts',(-0.789913991319501,0.0445180279388877,
-3.17492518820079));
#55005=CARTESIAN_POINT('Ctrl Pts',(-0.790749130436005,0.0296995801466835,
-3.17432784240843));
#55006=CARTESIAN_POINT('Ctrl Pts',(-0.791158303975227,0.0148571257566993,
-3.17373049661607));
#55007=CARTESIAN_POINT('Ctrl Pts',(-0.791146063621827,1.39968631027903E-5,
-3.17313315082371));
#55008=CARTESIAN_POINT('Origin',(0.,0.,-1.94));
#55009=CARTESIAN_POINT('',(-0.791071031963789,-1.87933227643877E-5,-2.9446668491763));
#55010=CARTESIAN_POINT('',(-0.791084859053011,-2.00741357560715E-5,-2.97313315082371));
#55011=CARTESIAN_POINT('',(-0.7911,-9.68818082805471E-17,-1.94));
#55012=CARTESIAN_POINT('Ctrl Pts',(-0.791071031963789,-1.87933227643877E-5,
-2.9446668491763));
#55013=CARTESIAN_POINT('Ctrl Pts',(-0.790990147666244,0.0912708088080257,
-2.94833969734634));
#55014=CARTESIAN_POINT('Ctrl Pts',(-0.7752003893603,0.182587668557959,-2.95201254551639));
#55015=CARTESIAN_POINT('Ctrl Pts',(-0.744238000845016,0.268432058012198,
-2.95568539368643));
#55016=CARTESIAN_POINT('Ctrl Pts',(-0.69970086979795,0.39191293290954,-2.96096851711809));
#55017=CARTESIAN_POINT('Ctrl Pts',(-0.623770477316596,0.504070873792558,
-2.96625164054975));
#55018=CARTESIAN_POINT('Ctrl Pts',(-0.525666549749928,0.591287282244812,
-2.97153476398141));
#55019=CARTESIAN_POINT('Ctrl Pts',(-0.427562622183257,0.678503690697069,
-2.97681788741307));
#55020=CARTESIAN_POINT('Ctrl Pts',(-0.307285159531272,0.740778566718563,
-2.98210101084473));
#55021=CARTESIAN_POINT('Ctrl Pts',(-0.179438660142546,0.770550283185138,
-2.98738413427639));
#55022=CARTESIAN_POINT('Ctrl Pts',(-0.0515921607538247,0.800321999651714,
-2.99266725770805));
#55023=CARTESIAN_POINT('Ctrl Pts',(0.0838233753716368,0.797590556563374,
-2.99795038113971));
#55024=CARTESIAN_POINT('Ctrl Pts',(0.210365333548509,0.762687615024313,
-3.00323350457137));
#55025=CARTESIAN_POINT('Ctrl Pts',(0.336907291725384,0.727784673485251,
-3.00851662800303));
#55026=CARTESIAN_POINT('Ctrl Pts',(0.45457567195367,0.660710233495468,-3.01379975143469));
#55027=CARTESIAN_POINT('Ctrl Pts',(0.549082779541173,0.569608701550274,
-3.01908287486635));
#55028=CARTESIAN_POINT('Ctrl Pts',(0.643589887128676,0.47850716960508,-3.02436599829801));
#55029=CARTESIAN_POINT('Ctrl Pts',(0.714935722075396,0.363378545704475,
-3.02964912172967));
#55030=CARTESIAN_POINT('Ctrl Pts',(0.754457230591514,0.238202138694498,
-3.03493224516133));
#55031=CARTESIAN_POINT('Ctrl Pts',(0.793978739107632,0.113025731684523,
-3.04021536859299));
#55032=CARTESIAN_POINT('Ctrl Pts',(0.801675921193149,-0.0221984584348243,
-3.04549849202465));
#55033=CARTESIAN_POINT('Ctrl Pts',(0.776614158835862,-0.151051050860679,
-3.05078161545631));
#55034=CARTESIAN_POINT('Ctrl Pts',(0.751552396478576,-0.279903643286535,
-3.05606473888798));
#55035=CARTESIAN_POINT('Ctrl Pts',(0.693731689678487,-0.402384638018896,
-3.06134786231963));
#55036=CARTESIAN_POINT('Ctrl Pts',(0.610172825192782,-0.503621976354,-3.06663098575129));
#55037=CARTESIAN_POINT('Ctrl Pts',(0.526613960707075,-0.604859314689106,
-3.07191410918295));
#55038=CARTESIAN_POINT('Ctrl Pts',(0.417316938535751,-0.684852996626952,
-3.07719723261461));
#55039=CARTESIAN_POINT('Ctrl Pts',(0.295552974620768,-0.733889917401286,
-3.08248035604627));
#55040=CARTESIAN_POINT('Ctrl Pts',(0.173789010705789,-0.782926838175618,
-3.08776347947793));
#55041=CARTESIAN_POINT('Ctrl Pts',(0.0395581050471505,-0.801006997786439,
-3.09304660290959));
#55042=CARTESIAN_POINT('Ctrl Pts',(-0.0908409695277596,-0.785935041797798,
-3.09832972634125));
#55043=CARTESIAN_POINT('Ctrl Pts',(-0.221240044102672,-0.770863085809156,
-3.10361284977292));
#55044=CARTESIAN_POINT('Ctrl Pts',(-0.347807287593856,-0.722639014221051,
-3.10889597320458));
#55045=CARTESIAN_POINT('Ctrl Pts',(-0.455174475083741,-0.647118357723447,
-3.11417909663624));
#55046=CARTESIAN_POINT('Ctrl Pts',(-0.562541662573625,-0.571597701225844,
-3.11946222006789));
#55047=CARTESIAN_POINT('Ctrl Pts',(-0.65070879406221,-0.468780459818742,
-3.12474534349956));
#55048=CARTESIAN_POINT('Ctrl Pts',(-0.708970316756539,-0.35115105243838,
-3.13002846693122));
#55049=CARTESIAN_POINT('Ctrl Pts',(-0.762780305639831,-0.242509245448644,
-3.13490792767958));
#55050=CARTESIAN_POINT('Ctrl Pts',(-0.791080040064552,-0.121232279427034,
-3.13978738842794));
#55051=CARTESIAN_POINT('Ctrl Pts',(-0.791156898220181,1.00405986563634E-5,
-3.1446668491763));
#55052=CARTESIAN_POINT('Ctrl Pts',(-0.791146063621827,1.39968631027903E-5,
-3.17313315082371));
#55053=CARTESIAN_POINT('Ctrl Pts',(-0.791050046247981,-0.116420407390624,
-3.16844737318441));
#55054=CARTESIAN_POINT('Ctrl Pts',(-0.765022950244057,-0.232896316223373,
-3.16376159554511));
#55055=CARTESIAN_POINT('Ctrl Pts',(-0.715261824728976,-0.33815157929433,
-3.15907581790581));
#55056=CARTESIAN_POINT('Ctrl Pts',(-0.659157120572815,-0.456824847520252,
-3.15379269447415));
#55057=CARTESIAN_POINT('Ctrl Pts',(-0.57288142080478,-0.561234290301691,
-3.14850957104249));
#55058=CARTESIAN_POINT('Ctrl Pts',(-0.466910614149181,-0.638702158199507,
-3.14322644761082));
#55059=CARTESIAN_POINT('Ctrl Pts',(-0.360939807493583,-0.716170026097323,
-3.13794332417916));
#55060=CARTESIAN_POINT('Ctrl Pts',(-0.235273893950421,-0.766696319111518,
-3.13266020074751));
#55061=CARTESIAN_POINT('Ctrl Pts',(-0.105171655891279,-0.784145963001124,
-3.12737707731584));
#55062=CARTESIAN_POINT('Ctrl Pts',(0.0249305821678641,-0.80159560689073,
-3.12209395388418));
#55063=CARTESIAN_POINT('Ctrl Pts',(0.159469144742986,-0.785968601655745,
-3.11681083045252));
#55064=CARTESIAN_POINT('Ctrl Pts',(0.28210790225815,-0.739162431389326,
-3.11152770702086));
#55065=CARTESIAN_POINT('Ctrl Pts',(0.404746659773314,-0.692356261122907,
-3.1062445835892));
#55066=CARTESIAN_POINT('Ctrl Pts',(0.515485612228519,-0.614370925825055,
-3.10096146015754));
#55067=CARTESIAN_POINT('Ctrl Pts',(0.600878459605494,-0.514675669986451,
-3.09567833672588));
#55068=CARTESIAN_POINT('Ctrl Pts',(0.686271306982469,-0.414980414147849,
-3.09039521329422));
#55069=CARTESIAN_POINT('Ctrl Pts',(0.746318049281215,-0.293575237768495,
-3.08511208986256));
#55070=CARTESIAN_POINT('Ctrl Pts',(0.773727606947812,-0.165201570030935,
-3.0798289664309));
#55071=CARTESIAN_POINT('Ctrl Pts',(0.801137164614409,-0.0368279022933761,
-3.07454584299924));
#55072=CARTESIAN_POINT('Ctrl Pts',(0.795909537648858,0.0985142568023888,
-3.06926271956758));
#55073=CARTESIAN_POINT('Ctrl Pts',(0.758679482286466,0.224391202259391,
-3.06397959613592));
#55074=CARTESIAN_POINT('Ctrl Pts',(0.721449426924073,0.350268147716393,
-3.05869647270426));
#55075=CARTESIAN_POINT('Ctrl Pts',(0.652216943164838,0.466679879534633,
-3.0534133492726));
#55076=CARTESIAN_POINT('Ctrl Pts',(0.559388474513935,0.559491289543318,
-3.04813022584094));
#55077=CARTESIAN_POINT('Ctrl Pts',(0.466560005863032,0.652302699552004,
-3.04284710240928));
#55078=CARTESIAN_POINT('Ctrl Pts',(0.350135552320461,0.721513787751136,
-3.03756397897762));
#55079=CARTESIAN_POINT('Ctrl Pts',(0.224251766772022,0.758720708557174,
-3.03228085554596));
#55080=CARTESIAN_POINT('Ctrl Pts',(0.0983679812235839,0.795927629363212,
-3.0269977321143));
#55081=CARTESIAN_POINT('Ctrl Pts',(-0.0369751363307216,0.801130382776156,
-3.02171460868264));
#55082=CARTESIAN_POINT('Ctrl Pts',(-0.165343764514632,0.773697232792003,
-3.01643148525098));
#55083=CARTESIAN_POINT('Ctrl Pts',(-0.293712392698542,0.746264082807851,
-3.01114836181932));
#55084=CARTESIAN_POINT('Ctrl Pts',(-0.415106531512058,0.686195029426602,
-3.00586523838766));
#55085=CARTESIAN_POINT('Ctrl Pts',(-0.514786091991394,0.600783861289651,
-3.000582114956));
#55086=CARTESIAN_POINT('Ctrl Pts',(-0.614465652470729,0.5153726931527,-2.99529899152434));
#55087=CARTESIAN_POINT('Ctrl Pts',(-0.692430634615885,0.404619410260047,
-2.99001586809268));
#55088=CARTESIAN_POINT('Ctrl Pts',(-0.739214265285162,0.281972052680388,
-2.98473274466102));
#55089=CARTESIAN_POINT('Ctrl Pts',(-0.773453550751941,0.192210787301005,
-2.98086621338191));
#55090=CARTESIAN_POINT('Ctrl Pts',(-0.790991297852172,0.0960787478750471,
-2.97699968210281));
#55091=CARTESIAN_POINT('Ctrl Pts',(-0.791084859053011,-2.00741357560715E-5,
-2.97313315082371));
#55092=CARTESIAN_POINT('Origin',(0.,0.,-1.94));
#55093=CARTESIAN_POINT('',(-0.791067783107607,1.83219459327505E-5,-2.7446668491763));
#55094=CARTESIAN_POINT('',(-0.79105596750504,1.59022465970799E-5,-2.77313315082371));
#55095=CARTESIAN_POINT('',(-0.7911,-9.68818082805471E-17,-1.94));
#55096=CARTESIAN_POINT('Ctrl Pts',(-0.791067783107607,1.83219459327505E-5,
-2.7446668491763));
#55097=CARTESIAN_POINT('Ctrl Pts',(-0.791103178687645,0.0412514554789803,
-2.74632575940143));
#55098=CARTESIAN_POINT('Ctrl Pts',(-0.787935332404873,0.0824792023563481,
-2.74798466962656));
#55099=CARTESIAN_POINT('Ctrl Pts',(-0.7815171568035,0.1231945830474,-2.74964357985169));
#55100=CARTESIAN_POINT('Ctrl Pts',(-0.761077223771279,0.252860660511613,
-2.75492670328335));
#55101=CARTESIAN_POINT('Ctrl Pts',(-0.707671529260795,0.377330174848837,
-2.76020982671501));
#55102=CARTESIAN_POINT('Ctrl Pts',(-0.62778477423003,0.481489614545734,
-2.76549295014667));
#55103=CARTESIAN_POINT('Ctrl Pts',(-0.547898019199265,0.585649054242631,
-2.77077607357833));
#55104=CARTESIAN_POINT('Ctrl Pts',(-0.441530203648218,0.669498419299202,
-2.77605919700999));
#55105=CARTESIAN_POINT('Ctrl Pts',(-0.321596869294389,0.722856434799122,
-2.78134232044165));
#55106=CARTESIAN_POINT('Ctrl Pts',(-0.201663534940562,0.776214450299041,
-2.78662544387331));
#55107=CARTESIAN_POINT('Ctrl Pts',(-0.0681646817839529,0.799081116242312,
-2.79190856730497));
#55108=CARTESIAN_POINT('Ctrl Pts',(0.0626898056511569,0.78867988432435,
-2.79719169073663));
#55109=CARTESIAN_POINT('Ctrl Pts',(0.193544293086269,0.778278652406388,
-2.80247481416829));
#55110=CARTESIAN_POINT('Ctrl Pts',(0.321754414799881,0.734609522627193,
-2.80775793759995));
#55111=CARTESIAN_POINT('Ctrl Pts',(0.431752462016372,0.662974949159658,
-2.81304106103161));
#55112=CARTESIAN_POINT('Ctrl Pts',(0.541750509232863,0.591340375692123,
-2.81832418446327));
#55113=CARTESIAN_POINT('Ctrl Pts',(0.633536481952231,0.491740358536247,
-2.82360730789493));
#55114=CARTESIAN_POINT('Ctrl Pts',(0.695965415378531,0.376268670324063,
-2.82889043132659));
#55115=CARTESIAN_POINT('Ctrl Pts',(0.758394348804829,0.260796982111881,
-2.83417355475825));
#55116=CARTESIAN_POINT('Ctrl Pts',(0.79146624293806,0.129453622843392,-2.83945667818991));
#55117=CARTESIAN_POINT('Ctrl Pts',(0.791165395978371,-0.00181325035172657,
-2.84473980162157));
#55118=CARTESIAN_POINT('Ctrl Pts',(0.790864549018682,-0.133080123546847,
-2.85002292505323));
#55119=CARTESIAN_POINT('Ctrl Pts',(0.757190960966073,-0.264270510668598,
-2.85530604848489));
#55120=CARTESIAN_POINT('Ctrl Pts',(0.694233393341295,-0.379454828985322,
-2.86058917191655));
#55121=CARTESIAN_POINT('Ctrl Pts',(0.631275825716517,-0.494639147302047,
-2.86587229534821));
#55122=CARTESIAN_POINT('Ctrl Pts',(0.53903427851957,-0.593817396813745,
-2.87115541877987));
#55123=CARTESIAN_POINT('Ctrl Pts',(0.428709033948005,-0.664947017349366,
-2.87643854221153));
#55124=CARTESIAN_POINT('Ctrl Pts',(0.31838378937644,-0.736076637884986,
-2.88172166564319));
#55125=CARTESIAN_POINT('Ctrl Pts',(0.189974847430256,-0.779157629444529,
-2.88700478907485));
#55126=CARTESIAN_POINT('Ctrl Pts',(0.0590740583135238,-0.788958951596863,
-2.89228791250651));
#55127=CARTESIAN_POINT('Ctrl Pts',(-0.0718267308032067,-0.798760273749196,
-2.89757103593817));
#55128=CARTESIAN_POINT('Ctrl Pts',(-0.205219367090492,-0.77528192649432,
-2.90285415936983));
#55129=CARTESIAN_POINT('Ctrl Pts',(-0.324906863237354,-0.721374730560832,
-2.90813728280149));
#55130=CARTESIAN_POINT('Ctrl Pts',(-0.444594359384217,-0.667467534627343,
-2.91342040623315));
#55131=CARTESIAN_POINT('Ctrl Pts',(-0.550576715390659,-0.583131490015245,
-2.91870352966481));
#55132=CARTESIAN_POINT('Ctrl Pts',(-0.629985193347303,-0.478606965926751,
-2.92398665309647));
#55133=CARTESIAN_POINT('Ctrl Pts',(-0.709393671303948,-0.374082441838257,
-2.92926977652813));
#55134=CARTESIAN_POINT('Ctrl Pts',(-0.762228271210791,-0.249369438273371,
-2.93455289995979));
#55135=CARTESIAN_POINT('Ctrl Pts',(-0.782073636357824,-0.119611032035093,
-2.93983602339145));
#55136=CARTESIAN_POINT('Ctrl Pts',(-0.788122425671071,-0.0800611797072125,
-2.94144629865307));
#55137=CARTESIAN_POINT('Ctrl Pts',(-0.79110649381175,-0.0400426062189334,
-2.94305657391468));
#55138=CARTESIAN_POINT('Ctrl Pts',(-0.791071031963789,-1.87933227643877E-5,
-2.9446668491763));
#55139=CARTESIAN_POINT('Ctrl Pts',(-0.791084859053011,-2.00741357560715E-5,
-2.97313315082371));
#55140=CARTESIAN_POINT('Ctrl Pts',(-0.791119137338463,-0.0352280751329303,
-2.97171655867115));
#55141=CARTESIAN_POINT('Ctrl Pts',(-0.788811898631655,-0.0704316173870898,
-2.9702999665186));
#55142=CARTESIAN_POINT('Ctrl Pts',(-0.784126621092215,-0.105315766095962,
-2.96888337436604));
#55143=CARTESIAN_POINT('Ctrl Pts',(-0.766653067036593,-0.235414795025995,
-2.96360025093438));
#55144=CARTESIAN_POINT('Ctrl Pts',(-0.71610367973195,-0.361071420619393,
-2.95831712750272));
#55145=CARTESIAN_POINT('Ctrl Pts',(-0.638616337606501,-0.467027988279004,
-2.95303400407106));
#55146=CARTESIAN_POINT('Ctrl Pts',(-0.561128995481052,-0.572984555938614,
-2.9477508806394));
#55147=CARTESIAN_POINT('Ctrl Pts',(-0.456703698534796,-0.659241065664438,
-2.94246775720774));
#55148=CARTESIAN_POINT('Ctrl Pts',(-0.338020121273455,-0.715323958852318,
-2.93718463377608));
#55149=CARTESIAN_POINT('Ctrl Pts',(-0.219336544012115,-0.771406852040197,
-2.93190151034442));
#55150=CARTESIAN_POINT('Ctrl Pts',(-0.0863946864356892,-0.797316128690136,
-2.92661838691276));
#55151=CARTESIAN_POINT('Ctrl Pts',(0.0446631992281643,-0.789905796363452,
-2.9213352634811));
#55152=CARTESIAN_POINT('Ctrl Pts',(0.17572108489202,-0.782495464036769,
-2.91605214004944));
#55153=CARTESIAN_POINT('Ctrl Pts',(0.304894998643301,-0.741765522733463,
-2.91076901661778));
#55154=CARTESIAN_POINT('Ctrl Pts',(0.416500204801163,-0.672661540371131,
-2.90548589318612));
#55155=CARTESIAN_POINT('Ctrl Pts',(0.528105410959024,-0.6035575580088,-2.90020276975446));
#55156=CARTESIAN_POINT('Ctrl Pts',(0.622141909523464,-0.506079534587444,
-2.8949196463228));
#55157=CARTESIAN_POINT('Ctrl Pts',(0.687191469200697,-0.392063583047012,
-2.88963652289114));
#55158=CARTESIAN_POINT('Ctrl Pts',(0.75224102887793,-0.27804763150658,-2.88435339945948));
#55159=CARTESIAN_POINT('Ctrl Pts',(0.788303649667956,-0.147493751847073,
-2.87907027602782));
#55160=CARTESIAN_POINT('Ctrl Pts',(0.791000485574522,-0.0162542399005356,
-2.87378715259616));
#55161=CARTESIAN_POINT('Ctrl Pts',(0.793697321481088,0.114985272046,-2.8685040291645));
#55162=CARTESIAN_POINT('Ctrl Pts',(0.763028372504193,0.246910416279567,
-2.86322090573284));
#55163=CARTESIAN_POINT('Ctrl Pts',(0.702717566674989,0.363502393362486,
-2.85793778230118));
#55164=CARTESIAN_POINT('Ctrl Pts',(0.642406760845787,0.480094370445405,
-2.85265465886952));
#55165=CARTESIAN_POINT('Ctrl Pts',(0.552454098164276,0.581353180377678,
-2.84737153543785));
#55166=CARTESIAN_POINT('Ctrl Pts',(0.443781936690031,0.654983634269986,
-2.84208841200619));
#55167=CARTESIAN_POINT('Ctrl Pts',(0.335109775215785,0.728614088162294,
-2.83680528857453));
#55168=CARTESIAN_POINT('Ctrl Pts',(0.207718114948804,0.774616186014636,
-2.83152216514288));
#55169=CARTESIAN_POINT('Ctrl Pts',(0.0770752842938398,0.787404196740719,
-2.82623904171122));
#55170=CARTESIAN_POINT('Ctrl Pts',(-0.0535675463611245,0.800192207466803,
-2.82095591827956));
#55171=CARTESIAN_POINT('Ctrl Pts',(-0.187461547404071,0.779766131066627,
-2.8156727948479));
#55172=CARTESIAN_POINT('Ctrl Pts',(-0.308348854111219,0.728606171166682,
-2.81038967141623));
#55173=CARTESIAN_POINT('Ctrl Pts',(-0.429236160818364,0.677446211266737,
-2.80510654798457));
#55174=CARTESIAN_POINT('Ctrl Pts',(-0.537116773189712,0.595552367867022,
-2.79982342455292));
#55175=CARTESIAN_POINT('Ctrl Pts',(-0.618891460575715,0.4928684697973,-2.79454030112126));
#55176=CARTESIAN_POINT('Ctrl Pts',(-0.700666147961719,0.390184571727577,
-2.7892571776896));
#55177=CARTESIAN_POINT('Ctrl Pts',(-0.756334910362378,0.266710618987845,
-2.78397405425794));
#55178=CARTESIAN_POINT('Ctrl Pts',(-0.779138257424125,0.137439238618277,
-2.77869093082627));
#55179=CARTESIAN_POINT('Ctrl Pts',(-0.787134536388695,0.0921086116374632,
-2.77683833749209));
#55180=CARTESIAN_POINT('Ctrl Pts',(-0.791089545934546,0.0460651086212764,
-2.7749857441579));
#55181=CARTESIAN_POINT('Ctrl Pts',(-0.79105596750504,1.59022465970799E-5,
-2.77313315082371));
#55182=CARTESIAN_POINT('Origin',(0.,0.,-1.94));
#55183=CARTESIAN_POINT('',(-0.791159134504794,-8.93421506220626E-6,-2.5446668491763));
#55184=CARTESIAN_POINT('',(-0.791165616430847,-4.19399107163473E-6,-2.57313315082371));
#55185=CARTESIAN_POINT('',(-0.7911,-9.68818082805471E-17,-1.94));
#55186=CARTESIAN_POINT('Ctrl Pts',(-0.791159134504794,-8.93421506220626E-6,
-2.5446668491763));
#55187=CARTESIAN_POINT('Ctrl Pts',(-0.791088724556594,0.12244083710649,
-2.54959494488817));
#55188=CARTESIAN_POINT('Ctrl Pts',(-0.762201994881393,0.244922676356341,
-2.55452304060005));
#55189=CARTESIAN_POINT('Ctrl Pts',(-0.70735329025823,0.354397085810968,
-2.55945113631192));
#55190=CARTESIAN_POINT('Ctrl Pts',(-0.64855319920225,0.47175820287759,-2.56473425974358));
#55191=CARTESIAN_POINT('Ctrl Pts',(-0.559915708359819,0.574170230602118,
-2.57001738317524));
#55192=CARTESIAN_POINT('Ctrl Pts',(-0.452203483155427,0.649197952471008,
-2.5753005066069));
#55193=CARTESIAN_POINT('Ctrl Pts',(-0.344491257951037,0.724225674339897,
-2.58058363003856));
#55194=CARTESIAN_POINT('Ctrl Pts',(-0.217704298384688,0.771869090353149,
-2.58586675347022));
#55195=CARTESIAN_POINT('Ctrl Pts',(-0.0872375080466301,0.786343174994394,
-2.59114987690188));
#55196=CARTESIAN_POINT('Ctrl Pts',(0.0432292822914291,0.800817259635639,
-2.59643300033354));
#55197=CARTESIAN_POINT('Ctrl Pts',(0.177375903401196,0.782122012904877,
-2.6017161237652));
#55198=CARTESIAN_POINT('Ctrl Pts',(0.298913816571699,0.732527475206897,
-2.60699924719686));
#55199=CARTESIAN_POINT('Ctrl Pts',(0.420451729742201,0.682932937508916,
-2.61228237062852));
#55200=CARTESIAN_POINT('Ctrl Pts',(0.52938093497344,0.602439108843718,-2.61756549406018));
#55201=CARTESIAN_POINT('Ctrl Pts',(0.612474877906563,0.50081982349323,-2.62284861749184));
#55202=CARTESIAN_POINT('Ctrl Pts',(0.695568820839685,0.399200538142744,
-2.6281317409235));
#55203=CARTESIAN_POINT('Ctrl Pts',(0.752827501474693,0.276455796106968,
-2.63341486435516));
#55204=CARTESIAN_POINT('Ctrl Pts',(0.777298376181737,0.14748968118375,-2.63869798778682));
#55205=CARTESIAN_POINT('Ctrl Pts',(0.801769250888782,0.018523566260528,
-2.64398111121848));
#55206=CARTESIAN_POINT('Ctrl Pts',(0.793452319667862,-0.116663921550136,
-2.64926423465014));
#55207=CARTESIAN_POINT('Ctrl Pts',(0.75335745257778,-0.241657857964453,
-2.6545473580818));
#55208=CARTESIAN_POINT('Ctrl Pts',(0.713262585487699,-0.366651794378766,
-2.65983048151346));
#55209=CARTESIAN_POINT('Ctrl Pts',(0.641389782528459,-0.481452179396731,
-2.66511360494513));
#55210=CARTESIAN_POINT('Ctrl Pts',(0.546466083737166,-0.572119560053153,
-2.67039672837679));
#55211=CARTESIAN_POINT('Ctrl Pts',(0.451542384945872,-0.662786940709577,
-2.67567985180845));
#55212=CARTESIAN_POINT('Ctrl Pts',(0.333567790322526,-0.729321317004456,
-2.6809629752401));
#55213=CARTESIAN_POINT('Ctrl Pts',(0.206867176152018,-0.763643858812038,
-2.68624609867176));
#55214=CARTESIAN_POINT('Ctrl Pts',(0.0801665619815108,-0.79796640061962,
-2.69152922210342));
#55215=CARTESIAN_POINT('Ctrl Pts',(-0.055260071736158,-0.800077107939904,
-2.69681234553509));
#55216=CARTESIAN_POINT('Ctrl Pts',(-0.182968762808292,-0.769719691515588,
-2.70209546896675));
#55217=CARTESIAN_POINT('Ctrl Pts',(-0.310677453880424,-0.739362275091273,
-2.70737859239841));
#55218=CARTESIAN_POINT('Ctrl Pts',(-0.430668202307021,-0.676536734922358,
-2.71266171583007));
#55219=CARTESIAN_POINT('Ctrl Pts',(-0.528371323555323,-0.588871561645531,
-2.71794483926173));
#55220=CARTESIAN_POINT('Ctrl Pts',(-0.626074444803625,-0.501206388368703,
-2.72322796269339));
#55221=CARTESIAN_POINT('Ctrl Pts',(-0.701489938873631,-0.388701581983963,
-2.72851108612505));
#55222=CARTESIAN_POINT('Ctrl Pts',(-0.745460600131655,-0.265017858495993,
-2.73379420955671));
#55223=CARTESIAN_POINT('Ctrl Pts',(-0.77562439495731,-0.180171045829891,
-2.73741842276324));
#55224=CARTESIAN_POINT('Ctrl Pts',(-0.790990454553786,-0.0900635069760673,
-2.74104263596977));
#55225=CARTESIAN_POINT('Ctrl Pts',(-0.791067783107607,1.83219459327505E-5,
-2.7446668491763));
#55226=CARTESIAN_POINT('Ctrl Pts',(-0.79105596750504,1.59022465970799E-5,
-2.77313315082371));
#55227=CARTESIAN_POINT('Ctrl Pts',(-0.790993788822369,-0.0852554768075867,
-2.76970262072624));
#55228=CARTESIAN_POINT('Ctrl Pts',(-0.777254906090452,-0.170546412443365,
-2.76627209062877));
#55229=CARTESIAN_POINT('Ctrl Pts',(-0.750173823124674,-0.251366671602233,
-2.7628415605313));
#55230=CARTESIAN_POINT('Ctrl Pts',(-0.70846811004064,-0.375832393453771,
-2.75755843709963));
#55231=CARTESIAN_POINT('Ctrl Pts',(-0.635118752149737,-0.489695029157441,
-2.75227531366797));
#55232=CARTESIAN_POINT('Ctrl Pts',(-0.539032077807812,-0.579128990457279,
-2.74699219023631));
#55233=CARTESIAN_POINT('Ctrl Pts',(-0.442945403465885,-0.668562951757118,
-2.74170906680465));
#55234=CARTESIAN_POINT('Ctrl Pts',(-0.324121412672936,-0.733568238653124,
-2.73642594337299));
#55235=CARTESIAN_POINT('Ctrl Pts',(-0.196988118283939,-0.766251688251861,
-2.73114281994133));
#55236=CARTESIAN_POINT('Ctrl Pts',(-0.0698548238949439,-0.798935137850597,
-2.72585969650967));
#55237=CARTESIAN_POINT('Ctrl Pts',(0.0655877740900931,-0.799296750152065,
-2.72057657307801));
#55238=CARTESIAN_POINT('Ctrl Pts',(0.192893775042879,-0.76729261696147,
-2.71529344964635));
#55239=CARTESIAN_POINT('Ctrl Pts',(0.320199775995663,-0.735288483770875,
-2.71001032621469));
#55240=CARTESIAN_POINT('Ctrl Pts',(0.439369179916195,-0.670918605088214,
-2.70472720278303));
#55241=CARTESIAN_POINT('Ctrl Pts',(0.535932032713452,-0.581998990381858,
-2.69944407935137));
#55242=CARTESIAN_POINT('Ctrl Pts',(0.632494885510708,-0.493079375675501,
-2.69416095591971));
#55243=CARTESIAN_POINT('Ctrl Pts',(0.706451187184694,-0.379610024945445,
-2.68887783248805));
#55244=CARTESIAN_POINT('Ctrl Pts',(0.748820912202367,-0.255368772449351,
-2.68359470905639));
#55245=CARTESIAN_POINT('Ctrl Pts',(0.791190637220041,-0.131127519953255,
-2.67831158562473));
#55246=CARTESIAN_POINT('Ctrl Pts',(0.801973785581401,0.0038856343088754,
-2.67302846219307));
#55247=CARTESIAN_POINT('Ctrl Pts',(0.77986103075957,0.133276934225298,-2.66774533876141));
#55248=CARTESIAN_POINT('Ctrl Pts',(0.757748275937739,0.26266823414172,-2.66246221532975));
#55249=CARTESIAN_POINT('Ctrl Pts',(0.702739617932715,0.38643767971243,-2.65717909189809));
#55250=CARTESIAN_POINT('Ctrl Pts',(0.621514394978597,0.489556764153312,
-2.65189596846643));
#55251=CARTESIAN_POINT('Ctrl Pts',(0.540289172024479,0.592675848594195,
-2.64661284503477));
#55252=CARTESIAN_POINT('Ctrl Pts',(0.432847384121266,0.67514457190525,-2.64132972160311));
#55253=CARTESIAN_POINT('Ctrl Pts',(0.312234978359981,0.726949301383814,
-2.63604659817145));
#55254=CARTESIAN_POINT('Ctrl Pts',(0.191622572598698,0.778754030862378,
-2.63076347473979));
#55255=CARTESIAN_POINT('Ctrl Pts',(0.0578395489793438,0.799894766508452,
-2.62548035130813));
#55256=CARTESIAN_POINT('Ctrl Pts',(-0.0728697030302944,0.787804528340724,
-2.62019722787647));
#55257=CARTESIAN_POINT('Ctrl Pts',(-0.203578955039934,0.775714290172996,
-2.61491410444481));
#55258=CARTESIAN_POINT('Ctrl Pts',(-0.331214435439859,0.730393078191463,
-2.60963098101315));
#55259=CARTESIAN_POINT('Ctrl Pts',(-0.440278210356008,0.657343948005596,
-2.60434785758149));
#55260=CARTESIAN_POINT('Ctrl Pts',(-0.549341985272158,0.584294817819729,
-2.59906473414983));
#55261=CARTESIAN_POINT('Ctrl Pts',(-0.639834054704532,0.483517769429526,
-2.59378161071817));
#55262=CARTESIAN_POINT('Ctrl Pts',(-0.700766563992376,0.367249494600322,
-2.58849848728651));
#55263=CARTESIAN_POINT('Ctrl Pts',(-0.759838217269807,0.254532009334278,
-2.58337670846557));
#55264=CARTESIAN_POINT('Ctrl Pts',(-0.79112821691516,0.127255041952799,
-2.57825492964464));
#55265=CARTESIAN_POINT('Ctrl Pts',(-0.791165616430847,-4.19399107163473E-6,
-2.57313315082371));
#55266=CARTESIAN_POINT('Origin',(0.,0.,-1.94));
#55267=CARTESIAN_POINT('',(-0.791035698195336,-6.17953886133949E-6,-2.3446668491763));
#55268=CARTESIAN_POINT('',(-0.791041154687578,-1.02586427583964E-5,-2.3731331508237));
#55269=CARTESIAN_POINT('',(-0.7911,-9.68818082805471E-17,-1.94));
#55270=CARTESIAN_POINT('Ctrl Pts',(-0.791035698195336,-6.17953886133949E-6,
-2.3446668491763));
#55271=CARTESIAN_POINT('Ctrl Pts',(-0.791015846145582,0.0724352453097401,
-2.34758100694326));
#55272=CARTESIAN_POINT('Ctrl Pts',(-0.7811516579661,0.144881969211618,-2.35049516471022));
#55273=CARTESIAN_POINT('Ctrl Pts',(-0.761514037378075,0.214574794760694,
-2.35340932247718));
#55274=CARTESIAN_POINT('Ctrl Pts',(-0.725912679535712,0.340922037813706,
-2.35869244590884));
#55275=CARTESIAN_POINT('Ctrl Pts',(-0.65818932680173,0.458218140476839,
-2.3639755693405));
#55276=CARTESIAN_POINT('Ctrl Pts',(-0.566567178862551,0.552220611265262,
-2.36925869277216));
#55277=CARTESIAN_POINT('Ctrl Pts',(-0.474945030923373,0.646223082053685,
-2.37454181620382));
#55278=CARTESIAN_POINT('Ctrl Pts',(-0.359424087778997,0.716931920967397,
-2.37982493963548));
#55279=CARTESIAN_POINT('Ctrl Pts',(-0.234031295011568,0.755761420440113,
-2.38510806306714));
#55280=CARTESIAN_POINT('Ctrl Pts',(-0.108638502244139,0.794590919912829,
-2.3903911864988));
#55281=CARTESIAN_POINT('Ctrl Pts',(0.0266261401463434,0.801541079944549,
-2.39567430993046));
#55282=CARTESIAN_POINT('Ctrl Pts',(0.155338339504752,0.775767988480032,
-2.40095743336212));
#55283=CARTESIAN_POINT('Ctrl Pts',(0.284050538863158,0.749994897015517,
-2.40624055679378));
#55284=CARTESIAN_POINT('Ctrl Pts',(0.406210295189492,0.691498554054766,
-2.41152368022544));
#55285=CARTESIAN_POINT('Ctrl Pts',(0.506984555639162,0.607381784394141,
-2.4168068036571));
#55286=CARTESIAN_POINT('Ctrl Pts',(0.607758816088832,0.523265014733517,
-2.42208992708876));
#55287=CARTESIAN_POINT('Ctrl Pts',(0.687147580661839,0.413527818373018,
-2.42737305052042));
#55288=CARTESIAN_POINT('Ctrl Pts',(0.735511195714536,0.291494858700841,
-2.43265617395208));
#55289=CARTESIAN_POINT('Ctrl Pts',(0.783874810767234,0.16946189902866,-2.43793929738374));
#55290=CARTESIAN_POINT('Ctrl Pts',(0.80121327629962,0.035133176044802,-2.4432224208154));
#55291=CARTESIAN_POINT('Ctrl Pts',(0.785421296891827,-0.0951806601112308,
-2.44850554424706));
#55292=CARTESIAN_POINT('Ctrl Pts',(0.769629317484034,-0.22549449626726,
-2.45378866767872));
#55293=CARTESIAN_POINT('Ctrl Pts',(0.720706893136064,-0.351793445595463,
-2.45907179111038));
#55294=CARTESIAN_POINT('Ctrl Pts',(0.644594350903746,-0.458741860367493,
-2.46435491454204));
#55295=CARTESIAN_POINT('Ctrl Pts',(0.568481808671427,-0.565690275139524,
-2.4696380379737));
#55296=CARTESIAN_POINT('Ctrl Pts',(0.465179148554758,-0.653288155355381,
-2.47492116140536));
#55297=CARTESIAN_POINT('Ctrl Pts',(0.347229730679673,-0.710899068646577,
-2.48020428483702));
#55298=CARTESIAN_POINT('Ctrl Pts',(0.229280312804588,-0.768509981937773,
-2.48548740826868));
#55299=CARTESIAN_POINT('Ctrl Pts',(0.0966841371710874,-0.796133928304308,
-2.49077053170034));
#55300=CARTESIAN_POINT('Ctrl Pts',(-0.0344585178696828,-0.790416714282204,
-2.496053655132));
#55301=CARTESIAN_POINT('Ctrl Pts',(-0.165601172910451,-0.784699500260099,
-2.50133677856366));
#55302=CARTESIAN_POINT('Ctrl Pts',(-0.295290307358489,-0.745641125849356,
-2.50661990199532));
#55303=CARTESIAN_POINT('Ctrl Pts',(-0.407778625684669,-0.677984191633678,
-2.51190302542698));
#55304=CARTESIAN_POINT('Ctrl Pts',(-0.520266944010852,-0.610327257417999,
-2.51718614885864));
#55305=CARTESIAN_POINT('Ctrl Pts',(-0.615554446215177,-0.514071763397382,
-2.5224692722903));
#55306=CARTESIAN_POINT('Ctrl Pts',(-0.682070999889633,-0.40090537883646,
-2.52775239572196));
#55307=CARTESIAN_POINT('Ctrl Pts',(-0.748587553564088,-0.28773899427554,
-2.53303551915362));
#55308=CARTESIAN_POINT('Ctrl Pts',(-0.786333158708677,-0.157661719174315,
-2.53831864258528));
#55309=CARTESIAN_POINT('Ctrl Pts',(-0.790724615646208,-0.0264679784193449,
-2.54360176601694));
#55310=CARTESIAN_POINT('Ctrl Pts',(-0.79101972306954,-0.017651713716691,
-2.54395679373673));
#55311=CARTESIAN_POINT('Ctrl Pts',(-0.791164206947543,-0.00883040718193987,
-2.54431182145651));
#55312=CARTESIAN_POINT('Ctrl Pts',(-0.791159134504794,-8.93421506220626E-6,
-2.5446668491763));
#55313=CARTESIAN_POINT('Ctrl Pts',(-0.791165616430847,-4.19399107163473E-6,
-2.57313315082371));
#55314=CARTESIAN_POINT('Ctrl Pts',(-0.791166794578228,-0.00401307305485152,
-2.57297180621298));
#55315=CARTESIAN_POINT('Ctrl Pts',(-0.791136959035539,-0.00802193452274154,
-2.57281046160226));
#55316=CARTESIAN_POINT('Ctrl Pts',(-0.791076001298007,-0.0120303226984998,
-2.57264911699153));
#55317=CARTESIAN_POINT('Ctrl Pts',(-0.789079980172478,-0.143282363899915,
-2.56736599355987));
#55318=CARTESIAN_POINT('Ctrl Pts',(-0.753714988778105,-0.274026945034545,
-2.56208287012821));
#55319=CARTESIAN_POINT('Ctrl Pts',(-0.689275164578622,-0.388388614649023,
-2.55679974669655));
#55320=CARTESIAN_POINT('Ctrl Pts',(-0.624835340379137,-0.502750284263503,
-2.55151662326489));
#55321=CARTESIAN_POINT('Ctrl Pts',(-0.531320683374539,-0.600729042357833,
-2.54623349983323));
#55322=CARTESIAN_POINT('Ctrl Pts',(-0.420086061082635,-0.670427975086027,
-2.54095037640157));
#55323=CARTESIAN_POINT('Ctrl Pts',(-0.308851438790733,-0.74012690781422,
-2.53566725296991));
#55324=CARTESIAN_POINT('Ctrl Pts',(-0.179896851211523,-0.781546015176281,
-2.53038412953825));
#55325=CARTESIAN_POINT('Ctrl Pts',(-0.0488804026965334,-0.789656048369224,
-2.52510100610659));
#55326=CARTESIAN_POINT('Ctrl Pts',(0.0821360458184596,-0.797766081562167,
-2.51981788267493));
#55327=CARTESIAN_POINT('Ctrl Pts',(0.215214355269229,-0.772567040585991,
-2.51453475924327));
#55328=CARTESIAN_POINT('Ctrl Pts',(0.334195704977728,-0.717118678649715,
-2.50925163581161));
#55329=CARTESIAN_POINT('Ctrl Pts',(0.453177054686225,-0.66167031671344,
-2.50396851237995));
#55330=CARTESIAN_POINT('Ctrl Pts',(0.558061444652449,-0.575972633817065,
-2.49868538894829));
#55331=CARTESIAN_POINT('Ctrl Pts',(0.636113455735699,-0.470431333911614,
-2.49340226551663));
#55332=CARTESIAN_POINT('Ctrl Pts',(0.714165466818948,-0.364890034006163,
-2.48811914208497));
#55333=CARTESIAN_POINT('Ctrl Pts',(0.765385099019224,-0.239505117091636,
-2.48283601865331));
#55334=CARTESIAN_POINT('Ctrl Pts',(0.783553090494863,-0.109501245973838,
-2.47755289522165));
#55335=CARTESIAN_POINT('Ctrl Pts',(0.801721081970502,0.0205026251439623,
-2.47226977178999));
#55336=CARTESIAN_POINT('Ctrl Pts',(0.786837432721503,0.155125450465034,
-2.46698664835833));
#55337=CARTESIAN_POINT('Ctrl Pts',(0.740709366030476,0.278020868944409,
-2.46170352492667));
#55338=CARTESIAN_POINT('Ctrl Pts',(0.69458129933945,0.40091628742378,-2.45642040149501));
#55339=CARTESIAN_POINT('Ctrl Pts',(0.617208815206396,0.512084299061456,
-2.45113727806335));
#55340=CARTESIAN_POINT('Ctrl Pts',(0.517986743650434,0.59802650601482,-2.44585415463169));
#55341=CARTESIAN_POINT('Ctrl Pts',(0.418764672094471,0.683968712968185,
-2.44057103120003));
#55342=CARTESIAN_POINT('Ctrl Pts',(0.297693013115599,0.74468511523724,-2.43528790776837));
#55343=CARTESIAN_POINT('Ctrl Pts',(0.169472699079944,0.772803320878238,
-2.43000478433671));
#55344=CARTESIAN_POINT('Ctrl Pts',(0.0412523850442884,0.800921526519236,
-2.42472166090505));
#55345=CARTESIAN_POINT('Ctrl Pts',(-0.0941165840481511,0.796441535532177,
-2.41943853747339));
#55346=CARTESIAN_POINT('Ctrl Pts',(-0.220197247839481,0.759907323650583,
-2.41415541404173));
#55347=CARTESIAN_POINT('Ctrl Pts',(-0.346277911630814,0.723373111768988,
-2.40887229061007));
#55348=CARTESIAN_POINT('Ctrl Pts',(-0.463070270121033,0.654784678992858,
-2.40358916717841));
#55349=CARTESIAN_POINT('Ctrl Pts',(-0.55639299815506,0.562470265967808,
-2.39830604374674));
#55350=CARTESIAN_POINT('Ctrl Pts',(-0.649715726189086,0.47015585294276,
-2.39302292031508));
#55351=CARTESIAN_POINT('Ctrl Pts',(-0.719568823766917,0.354115459668794,
-2.38773979688343));
#55352=CARTESIAN_POINT('Ctrl Pts',(-0.757470490344006,0.228439105128446,
-2.38245667345177));
#55353=CARTESIAN_POINT('Ctrl Pts',(-0.779766457905857,0.154508954367816,
-2.37934883257575));
#55354=CARTESIAN_POINT('Ctrl Pts',(-0.791005704550203,0.0772443008585653,
-2.37624099169973));
#55355=CARTESIAN_POINT('Ctrl Pts',(-0.791041154687578,-1.02586427583964E-5,
-2.3731331508237));
#55356=CARTESIAN_POINT('Origin',(0.,0.,-1.94));
#55357=CARTESIAN_POINT('',(-0.791124794068662,1.84093985718808E-5,-2.1446668491763));
#55358=CARTESIAN_POINT('',(-0.791109792329072,1.99241595253492E-5,-2.17313315082371));
#55359=CARTESIAN_POINT('',(-0.7911,-9.68818082805471E-17,-1.94));
#55360=CARTESIAN_POINT('Ctrl Pts',(-0.791124794068662,1.84093985718808E-5,
-2.1446668491763));
#55361=CARTESIAN_POINT('Ctrl Pts',(-0.791147010981146,0.0223892334141203,
-2.14556706899834));
#55362=CARTESIAN_POINT('Ctrl Pts',(-0.790217040500928,0.0447582160969252,
-2.14646728882039));
#55363=CARTESIAN_POINT('Ctrl Pts',(-0.788321589215395,0.0670450866757845,
-2.14736750864243));
#55364=CARTESIAN_POINT('Ctrl Pts',(-0.777197747177103,0.197840127276048,
-2.15265063207409));
#55365=CARTESIAN_POINT('Ctrl Pts',(-0.732821120792358,0.325807088778621,
-2.15793375550575));
#55366=CARTESIAN_POINT('Ctrl Pts',(-0.660580070876739,0.435407787747225,
-2.16321687893741));
#55367=CARTESIAN_POINT('Ctrl Pts',(-0.58833902096112,0.545008486715829,
-2.16850000236907));
#55368=CARTESIAN_POINT('Ctrl Pts',(-0.488233547514627,0.636242923150465,
-2.17378312580073));
#55369=CARTESIAN_POINT('Ctrl Pts',(-0.372418797390191,0.698033101665596,
-2.17906624923239));
#55370=CARTESIAN_POINT('Ctrl Pts',(-0.256604047265758,0.759823280180726,
-2.18434937266405));
#55371=CARTESIAN_POINT('Ctrl Pts',(-0.125080020463381,0.792169200776354,
-2.18963249609571));
#55372=CARTESIAN_POINT('Ctrl Pts',(0.00618318862119299,0.791143311827209,
-2.19491561952737));
#55373=CARTESIAN_POINT('Ctrl Pts',(0.13744639770577,0.790117422878065,-2.20019874295903));
#55374=CARTESIAN_POINT('Ctrl Pts',(0.26844878907254,0.755719724384149,-2.20548186639069));
#55375=CARTESIAN_POINT('Ctrl Pts',(0.383283607073439,0.692126901817306,
-2.21076498982235));
#55376=CARTESIAN_POINT('Ctrl Pts',(0.498118425074332,0.628534079250467,
-2.21604811325401));
#55377=CARTESIAN_POINT('Ctrl Pts',(0.596785669709354,0.535746132610701,
-2.22133123668567));
#55378=CARTESIAN_POINT('Ctrl Pts',(0.667304828756521,0.425029689773172,
-2.22661436011733));
#55379=CARTESIAN_POINT('Ctrl Pts',(0.737823987803694,0.314313246935636,
-2.23189748354899));
#55380=CARTESIAN_POINT('Ctrl Pts',(0.780195061263012,0.185668307900335,
-2.23718060698065));
#55381=CARTESIAN_POINT('Ctrl Pts',(0.789273209372148,0.0547153784400642,
-2.24246373041231));
#55382=CARTESIAN_POINT('Ctrl Pts',(0.798351357481284,-0.0762375510202047,
-2.24774685384397));
#55383=CARTESIAN_POINT('Ctrl Pts',(0.774136580240238,-0.209498470905439,
-2.25302997727563));
#55384=CARTESIAN_POINT('Ctrl Pts',(0.719569118209714,-0.32888638735792,
-2.25831310070729));
#55385=CARTESIAN_POINT('Ctrl Pts',(0.665001656179192,-0.448274303810399,
-2.26359622413895));
#55386=CARTESIAN_POINT('Ctrl Pts',(0.580081509359193,-0.553789216830127,
-2.26887934757061));
#55387=CARTESIAN_POINT('Ctrl Pts',(0.475119970627436,-0.632619147024047,
-2.27416247100227));
#55388=CARTESIAN_POINT('Ctrl Pts',(0.370158431895679,-0.711449077217968,
-2.27944559443393));
#55389=CARTESIAN_POINT('Ctrl Pts',(0.245155501252162,-0.763594024586081,
-2.2847287178656));
#55390=CARTESIAN_POINT('Ctrl Pts',(0.115289459431262,-0.782722372373818,
-2.29001184129726));
#55391=CARTESIAN_POINT('Ctrl Pts',(-0.0145765823896404,-0.801850720161556,
-2.29529496472892));
#55392=CARTESIAN_POINT('Ctrl Pts',(-0.149305735387928,-0.787962468368917,
-2.30057808816058));
#55393=CARTESIAN_POINT('Ctrl Pts',(-0.272538727850647,-0.74274397573592,
-2.30586121159224));
#55394=CARTESIAN_POINT('Ctrl Pts',(-0.395771720313366,-0.697525483102923,
-2.3111443350239));
#55395=CARTESIAN_POINT('Ctrl Pts',(-0.507508552240518,-0.620976749629566,
-2.31642745845556));
#55396=CARTESIAN_POINT('Ctrl Pts',(-0.59418175769647,-0.522392582729869,
-2.32171058188722));
#55397=CARTESIAN_POINT('Ctrl Pts',(-0.680854963152421,-0.423808415830174,
-2.32699370531888));
#55398=CARTESIAN_POINT('Ctrl Pts',(-0.742464542137174,-0.303188815504138,
-2.33227682875054));
#55399=CARTESIAN_POINT('Ctrl Pts',(-0.771529650154178,-0.175179823619676,
-2.3375599521822));
#55400=CARTESIAN_POINT('Ctrl Pts',(-0.784562516757381,-0.11778027381361,
-2.3399289178469));
#55401=CARTESIAN_POINT('Ctrl Pts',(-0.791051836245505,-0.0588949775696238,
-2.3422978835116));
#55402=CARTESIAN_POINT('Ctrl Pts',(-0.791035698195336,-6.17953886133949E-6,
-2.3446668491763));
#55403=CARTESIAN_POINT('Ctrl Pts',(-0.791041154687578,-1.02586427583964E-5,
-2.3731331508237));
#55404=CARTESIAN_POINT('Ctrl Pts',(-0.791065967433308,-0.0540833281243991,
-2.37095786826806));
#55405=CARTESIAN_POINT('Ctrl Pts',(-0.785601959816742,-0.108151452479073,
-2.36878258571242));
#55406=CARTESIAN_POINT('Ctrl Pts',(-0.774598699244007,-0.161067760968372,
-2.36660730315678));
#55407=CARTESIAN_POINT('Ctrl Pts',(-0.747875005990574,-0.289585956718112,
-2.36132417972512));
#55408=CARTESIAN_POINT('Ctrl Pts',(-0.68847738390736,-0.411310032410861,
-2.35604105629347));
#55409=CARTESIAN_POINT('Ctrl Pts',(-0.6036180941653,-0.511459837025474,
-2.35075793286181));
#55410=CARTESIAN_POINT('Ctrl Pts',(-0.518758804423239,-0.611609641640088,
-2.34547480943015));
#55411=CARTESIAN_POINT('Ctrl Pts',(-0.408437847022332,-0.690185175176567,
-2.34019168599848));
#55412=CARTESIAN_POINT('Ctrl Pts',(-0.286050767600555,-0.737645529267958,
-2.33490856256682));
#55413=CARTESIAN_POINT('Ctrl Pts',(-0.163663688178782,-0.785105883359348,
-2.32962543913516));
#55414=CARTESIAN_POINT('Ctrl Pts',(-0.0292104867361406,-0.801451058005654,
-2.32434231570351));
#55415=CARTESIAN_POINT('Ctrl Pts',(0.100983071990288,-0.784696366542676,
-2.31905919227185));
#55416=CARTESIAN_POINT('Ctrl Pts',(0.231176630716716,-0.767941675079698,
-2.31377606884019));
#55417=CARTESIAN_POINT('Ctrl Pts',(0.357110546726931,-0.718087117507435,
-2.30849294540852));
#55418=CARTESIAN_POINT('Ctrl Pts',(0.463493495878834,-0.641186203666213,
-2.30320982197686));
#55419=CARTESIAN_POINT('Ctrl Pts',(0.569876445030741,-0.564285289824989,
-2.2979266985452));
#55420=CARTESIAN_POINT('Ctrl Pts',(0.656708427324334,-0.460338019714802,
-2.29264357511354));
#55421=CARTESIAN_POINT('Ctrl Pts',(0.713446008320202,-0.341966024198084,
-2.28736045168189));
#55422=CARTESIAN_POINT('Ctrl Pts',(0.770183589316067,-0.223594028681369,
-2.28207732825022));
#55423=CARTESIAN_POINT('Ctrl Pts',(0.796826769014208,-0.0907973077581235,
-2.27679420481856));
#55424=CARTESIAN_POINT('Ctrl Pts',(0.790140441973232,0.040299509329755,
-2.2715110813869));
#55425=CARTESIAN_POINT('Ctrl Pts',(0.783454114932256,0.171396326417634,
-2.26622795795524));
#55426=CARTESIAN_POINT('Ctrl Pts',(0.743438281152164,0.300793239670145,
-2.26094483452358));
#55427=CARTESIAN_POINT('Ctrl Pts',(0.674951799187771,0.412778436049007,
-2.25566171109192));
#55428=CARTESIAN_POINT('Ctrl Pts',(0.606465317223377,0.524763632427871,
-2.25037858766026));
#55429=CARTESIAN_POINT('Ctrl Pts',(0.509508187074682,0.619337111933087,
-2.2450954642286));
#55430=CARTESIAN_POINT('Ctrl Pts',(0.395853273049907,0.685015441219794,
-2.23981234079694));
#55431=CARTESIAN_POINT('Ctrl Pts',(0.282198359025133,0.750693770506501,
-2.23452921736528));
#55432=CARTESIAN_POINT('Ctrl Pts',(0.151845661124279,0.787476949574701,
-2.22924609393362));
#55433=CARTESIAN_POINT('Ctrl Pts',(0.0206230470064235,0.790898639792764,
-2.22396297050196));
#55434=CARTESIAN_POINT('Ctrl Pts',(-0.110599567111434,0.794320330010827,
-2.2186798470703));
#55435=CARTESIAN_POINT('Ctrl Pts',(-0.242692097446293,0.764380531378753,
-2.21339672363864));
#55436=CARTESIAN_POINT('Ctrl Pts',(-0.359615419971102,0.704714636014381,
-2.20811360020698));
#55437=CARTESIAN_POINT('Ctrl Pts',(-0.476538742495907,0.64504874065001,
-2.20283047677532));
#55438=CARTESIAN_POINT('Ctrl Pts',(-0.578292857210662,0.555656748553344,
-2.19754735334366));
#55439=CARTESIAN_POINT('Ctrl Pts',(-0.652522433635772,0.447392939255776,
-2.192264229912));
#55440=CARTESIAN_POINT('Ctrl Pts',(-0.726752010060884,0.339129129958207,
-2.18698110648034));
#55441=CARTESIAN_POINT('Ctrl Pts',(-0.773457048196351,0.211993503459735,
-2.18169798304868));
#55442=CARTESIAN_POINT('Ctrl Pts',(-0.786966463557351,0.0814232996746597,
-2.17641485961702));
#55443=CARTESIAN_POINT('Ctrl Pts',(-0.789763670408956,0.0543879425638447,
-2.17532095668592));
#55444=CARTESIAN_POINT('Ctrl Pts',(-0.791137706940641,0.0272053374713011,
-2.17422705375481));
#55445=CARTESIAN_POINT('Ctrl Pts',(-0.791109792329072,1.99241595253492E-5,
-2.17313315082371));
#55446=CARTESIAN_POINT('Origin',(0.,0.,-1.94));
#55447=CARTESIAN_POINT('',(-0.791108239651095,-2.00188069073848E-5,-1.9446668491763));
#55448=CARTESIAN_POINT('',(-0.791123285936247,-1.86130038508075E-5,-1.97313315082371));
#55449=CARTESIAN_POINT('',(-0.7911,-9.68818082805471E-17,-1.94));
#55450=CARTESIAN_POINT('Ctrl Pts',(-0.791108239651095,-2.00188069073848E-5,
-1.9446668491763));
#55451=CARTESIAN_POINT('Ctrl Pts',(-0.791001791698214,0.10359762893025,
-1.94883625448509));
#55452=CARTESIAN_POINT('Ctrl Pts',(-0.770534133686574,0.207256088513461,
-1.95300565979388));
#55453=CARTESIAN_POINT('Ctrl Pts',(-0.73086526413353,0.302955338876006,
-1.95717506510267));
#55454=CARTESIAN_POINT('Ctrl Pts',(-0.680600173857629,0.42421746489593,
-1.96245818853433));
#55455=CARTESIAN_POINT('Ctrl Pts',(-0.599505907586774,0.53270040449236,
-1.96774131196599));
#55456=CARTESIAN_POINT('Ctrl Pts',(-0.497429206777909,0.615231790396717,
-1.97302443539765));
#55457=CARTESIAN_POINT('Ctrl Pts',(-0.395352505969043,0.697763176301074,
-1.97830755882931));
#55458=CARTESIAN_POINT('Ctrl Pts',(-0.272293370622168,0.754343008513358,
-1.98359068226097));
#55459=CARTESIAN_POINT('Ctrl Pts',(-0.143194059239612,0.778101171486672,
-1.98887380569263));
#55460=CARTESIAN_POINT('Ctrl Pts',(-0.0140947478570534,0.801859334459987,
-1.99415692912429));
#55461=CARTESIAN_POINT('Ctrl Pts',(0.121044739561186,0.792795828194329,
-1.99944005255595));
#55462=CARTESIAN_POINT('Ctrl Pts',(0.245815307102121,0.752011174428106,
-2.00472317598761));
#55463=CARTESIAN_POINT('Ctrl Pts',(0.370585874643055,0.711226520661884,
-2.01000629941927));
#55464=CARTESIAN_POINT('Ctrl Pts',(0.484987522306685,0.638720719395097,
-2.01528942285093));
#55465=CARTESIAN_POINT('Ctrl Pts',(0.575129213172718,0.543297671470971,
-2.02057254628259));
#55466=CARTESIAN_POINT('Ctrl Pts',(0.665270904038749,0.447874623546849,
-2.02585566971425));
#55467=CARTESIAN_POINT('Ctrl Pts',(0.731152638107186,0.329534328965388,
-2.03113879314591));
#55468=CARTESIAN_POINT('Ctrl Pts',(0.764774831289796,0.202646068543442,
-2.03642191657757));
#55469=CARTESIAN_POINT('Ctrl Pts',(0.798397024472407,0.0757578081214934,
-2.04170504000923));
#55470=CARTESIAN_POINT('Ctrl Pts',(0.799759676769191,-0.0596784181409368,
-2.04698816344089));
#55471=CARTESIAN_POINT('Ctrl Pts',(0.768697330306502,-0.187217483291771,
-2.05227128687255));
#55472=CARTESIAN_POINT('Ctrl Pts',(0.737634983843813,-0.314756548442608,
-2.05755441030421));
#55473=CARTESIAN_POINT('Ctrl Pts',(0.674147638621649,-0.434398452481844,
-2.06283753373587));
#55474=CARTESIAN_POINT('Ctrl Pts',(0.585944143895796,-0.531615868747983,
-2.06812065716753));
#55475=CARTESIAN_POINT('Ctrl Pts',(0.497740649169944,-0.628833285014119,
-2.07340378059919));
#55476=CARTESIAN_POINT('Ctrl Pts',(0.384821004940404,-0.70362621350716,
-2.07868690403085));
#55477=CARTESIAN_POINT('Ctrl Pts',(0.260896298233043,-0.746913042621927,
-2.08397002746251));
#55478=CARTESIAN_POINT('Ctrl Pts',(0.136971591525681,-0.790199871736694,
-2.08925315089417));
#55479=CARTESIAN_POINT('Ctrl Pts',(0.00204182234049846,-0.801980601473188,
-2.09453627432583));
#55480=CARTESIAN_POINT('Ctrl Pts',(-0.127509378110229,-0.780824775583096,
-2.09981939775749));
#55481=CARTESIAN_POINT('Ctrl Pts',(-0.25706057856096,-0.759668949693004,
-2.10510252118915));
#55482=CARTESIAN_POINT('Ctrl Pts',(-0.381233210277237,-0.705576568176324,
-2.11038564462081));
#55483=CARTESIAN_POINT('Ctrl Pts',(-0.484949810242685,-0.625115711861438,
-2.11566876805247));
#55484=CARTESIAN_POINT('Ctrl Pts',(-0.588666410208131,-0.544654855546555,
-2.12095189148413));
#55485=CARTESIAN_POINT('Ctrl Pts',(-0.671926978422749,-0.437825524433467,
-2.12623501491579));
#55486=CARTESIAN_POINT('Ctrl Pts',(-0.724621733684138,-0.317599299027947,
-2.13151813834745));
#55487=CARTESIAN_POINT('Ctrl Pts',(-0.768337546125482,-0.217859066925389,
-2.13590104195707));
#55488=CARTESIAN_POINT('Ctrl Pts',(-0.791016626503881,-0.108898505033576,
-2.14028394556668));
#55489=CARTESIAN_POINT('Ctrl Pts',(-0.791124794068662,1.84093985718808E-5,
-2.1446668491763));
#55490=CARTESIAN_POINT('Ctrl Pts',(-0.791109792329072,1.99241595253492E-5,
-2.17313315082371));
#55491=CARTESIAN_POINT('Ctrl Pts',(-0.791002890281618,-0.104089579091132,
-2.16894393032315));
#55492=CARTESIAN_POINT('Ctrl Pts',(-0.770335105915875,-0.208240267418343,
-2.1647547098226));
#55493=CARTESIAN_POINT('Ctrl Pts',(-0.730298207536194,-0.304319727528954,
-2.16056548932204));
#55494=CARTESIAN_POINT('Ctrl Pts',(-0.679806743567504,-0.425487769875812,
-2.15528236589038));
#55495=CARTESIAN_POINT('Ctrl Pts',(-0.598510023043591,-0.533819073497853,
-2.14999924245872));
#55496=CARTESIAN_POINT('Ctrl Pts',(-0.496279370104967,-0.616159683281932,
-2.14471611902706));
#55497=CARTESIAN_POINT('Ctrl Pts',(-0.394048717166343,-0.698500293066012,
-2.1394329955954));
#55498=CARTESIAN_POINT('Ctrl Pts',(-0.270884131813007,-0.754850209012131,
-2.13414987216374));
#55499=CARTESIAN_POINT('Ctrl Pts',(-0.141740676645508,-0.778367232787935,
-2.12886674873208));
#55500=CARTESIAN_POINT('Ctrl Pts',(-0.012597221478007,-0.801884256563738,
-2.12358362530042));
#55501=CARTESIAN_POINT('Ctrl Pts',(0.122525103503658,-0.792568388169225,
-2.11830050186876));
#55502=CARTESIAN_POINT('Ctrl Pts',(0.247219286307887,-0.751550792010289,
-2.1130173784371));
#55503=CARTESIAN_POINT('Ctrl Pts',(0.371913469112115,-0.710533195851353,
-2.10773425500544));
#55504=CARTESIAN_POINT('Ctrl Pts',(0.486179509738909,-0.637813871927994,
-2.10245113157378));
#55505=CARTESIAN_POINT('Ctrl Pts',(0.576142837135329,-0.542222647730181,
-2.09716800814212));
#55506=CARTESIAN_POINT('Ctrl Pts',(0.666106164531748,-0.446631423532368,
-2.09188488471046));
#55507=CARTESIAN_POINT('Ctrl Pts',(0.731766778697792,-0.328168299060104,
-2.0866017612788));
#55508=CARTESIAN_POINT('Ctrl Pts',(0.765151944675387,-0.201217469553084,
-2.08131863784714));
#55509=CARTESIAN_POINT('Ctrl Pts',(0.798537110652983,-0.0742666400460645,
-2.07603551441548));
#55510=CARTESIAN_POINT('Ctrl Pts',(0.799646828442127,0.0611718944957136,
-2.07075239098382));
#55511=CARTESIAN_POINT('Ctrl Pts',(0.768346352336834,0.188652726841028,
-2.06546926755216));
#55512=CARTESIAN_POINT('Ctrl Pts',(0.737045876231541,0.316133559186346,
-2.0601861441205));
#55513=CARTESIAN_POINT('Ctrl Pts',(0.673335206231814,0.4356566893352,-2.05490302068884));
#55514=CARTESIAN_POINT('Ctrl Pts',(0.584950308447026,0.532709212555596,
-2.04961989725718));
#55515=CARTESIAN_POINT('Ctrl Pts',(0.496565410662241,0.629761735775988,
-2.04433677382552));
#55516=CARTESIAN_POINT('Ctrl Pts',(0.383506285092399,0.704343652067918,
-2.03905365039386));
#55517=CARTESIAN_POINT('Ctrl Pts',(0.259500955061815,0.747398971644917,
-2.0337705269622));
#55518=CARTESIAN_POINT('Ctrl Pts',(0.135495625031231,0.790454291221916,
-2.02848740353054));
#55519=CARTESIAN_POINT('Ctrl Pts',(0.000544090539904729,0.801983014083983,
-2.02320428009888));
#55520=CARTESIAN_POINT('Ctrl Pts',(-0.128967374382433,0.780585283514092,
-2.01792115666722));
#55521=CARTESIAN_POINT('Ctrl Pts',(-0.25847883930477,0.759187552944201,
-2.01263803323556));
#55522=CARTESIAN_POINT('Ctrl Pts',(-0.38255023465812,0.704863368942352,
-2.0073549098039));
#55523=CARTESIAN_POINT('Ctrl Pts',(-0.486116389889406,0.624208958582592,
-2.00207178637224));
#55524=CARTESIAN_POINT('Ctrl Pts',(-0.589682545120693,0.543554548222831,
-1.99678866294058));
#55525=CARTESIAN_POINT('Ctrl Pts',(-0.672743460229917,0.43656991150516,
-1.99150553950892));
#55526=CARTESIAN_POINT('Ctrl Pts',(-0.72521359657337,0.316245486669755,
-1.98622241607726));
#55527=CARTESIAN_POINT('Ctrl Pts',(-0.768546266560072,0.216875083692276,
-1.98185932765941));
#55528=CARTESIAN_POINT('Ctrl Pts',(-0.791014961891894,0.108406481439749,
-1.97749623924156));
#55529=CARTESIAN_POINT('Ctrl Pts',(-0.791123285936247,-1.86130038508075E-5,
-1.97313315082371));
#55530=CARTESIAN_POINT('Origin',(0.,0.,-1.94));
#55531=CARTESIAN_POINT('',(-0.791041867722209,1.06520765539853E-5,-1.74466684917629));
#55532=CARTESIAN_POINT('',(-0.791036127465933,6.61336014326832E-6,-1.77313315082371));
#55533=CARTESIAN_POINT('',(-0.7911,-9.68818082805471E-17,-1.94));
#55534=CARTESIAN_POINT('Ctrl Pts',(-0.791041867722209,1.06520765539853E-5,
-1.74466684917629));
#55535=CARTESIAN_POINT('Ctrl Pts',(-0.791067426481375,0.0535910187405824,
-1.74682231654017));
#55536=CARTESIAN_POINT('Ctrl Pts',(-0.785703237583341,0.107166337835382,
-1.74897778390405));
#55537=CARTESIAN_POINT('Ctrl Pts',(-0.774898150389007,0.159620888965527,
-1.75113325126792));
#55538=CARTESIAN_POINT('Ctrl Pts',(-0.74841451612285,0.288188768404265,
-1.75641637469958));
#55539=CARTESIAN_POINT('Ctrl Pts',(-0.689244321653519,0.410023559379395,
-1.76169949813124));
#55540=CARTESIAN_POINT('Ctrl Pts',(-0.604572213118025,0.510331667443853,
-1.7669826215629));
#55541=CARTESIAN_POINT('Ctrl Pts',(-0.519900104582533,0.610639775508309,
-1.77226574499456));
#55542=CARTESIAN_POINT('Ctrl Pts',(-0.40972608198088,0.689421200662094,
-1.77754886842622));
#55543=CARTESIAN_POINT('Ctrl Pts',(-0.287427849628273,0.737110034478243,
-1.78283199185788));
#55544=CARTESIAN_POINT('Ctrl Pts',(-0.165129617275666,0.784798868294392,
-1.78811511528954));
#55545=CARTESIAN_POINT('Ctrl Pts',(-0.0307071751721049,0.801395110772904,
-1.7933982387212));
#55546=CARTESIAN_POINT('Ctrl Pts',(0.0995174468488339,0.784883589739994,
-1.79868136215286));
#55547=CARTESIAN_POINT('Ctrl Pts',(0.229742068869776,0.768372068707083,
-1.80396448558452));
#55548=CARTESIAN_POINT('Ctrl Pts',(0.355768870808095,0.718752784162747,
-1.80924760901618));
#55549=CARTESIAN_POINT('Ctrl Pts',(0.462295249996574,0.642050678296546,
-1.81453073244784));
#55550=CARTESIAN_POINT('Ctrl Pts',(0.568821629185048,0.565348572430349,
-1.8198138558795));
#55551=CARTESIAN_POINT('Ctrl Pts',(0.655847585623682,0.461563645242291,
-1.82509697931116));
#55552=CARTESIAN_POINT('Ctrl Pts',(0.712806131873042,0.343297815365377,
-1.83038010274282));
#55553=CARTESIAN_POINT('Ctrl Pts',(0.769764678122405,0.225031985488458,
-1.83566322617448));
#55554=CARTESIAN_POINT('Ctrl Pts',(0.796655814182489,0.0922852529226771,
-1.84094634960614));
#55555=CARTESIAN_POINT('Ctrl Pts',(0.790214326907609,-0.0388238228463354,
-1.8462294730378));
#55556=CARTESIAN_POINT('Ctrl Pts',(0.78377283963273,-0.16993289861535,-1.85151259646946));
#55557=CARTESIAN_POINT('Ctrl Pts',(0.743998729022887,-0.2994043175876,-1.85679571990112));
#55558=CARTESIAN_POINT('Ctrl Pts',(0.675721502783927,-0.411517219987063,
-1.86207884333278));
#55559=CARTESIAN_POINT('Ctrl Pts',(0.60744427654497,-0.523630122386523,
-1.86736196676444));
#55560=CARTESIAN_POINT('Ctrl Pts',(0.510663934676898,-0.618384508213195,
-1.87264509019611));
#55561=CARTESIAN_POINT('Ctrl Pts',(0.397131875253981,-0.684274977861756,
-1.87792821362777));
#55562=CARTESIAN_POINT('Ctrl Pts',(0.283599815831065,-0.750165447510315,
-1.88321133705943));
#55563=CARTESIAN_POINT('Ctrl Pts',(0.153316038853301,-0.787192000980764,
-1.88849446049108));
#55564=CARTESIAN_POINT('Ctrl Pts',(0.0221000433670234,-0.790858748294299,
-1.89377758392274));
#55565=CARTESIAN_POINT('Ctrl Pts',(-0.10911595211926,-0.794525495607834,
-1.8990607073544));
#55566=CARTESIAN_POINT('Ctrl Pts',(-0.24126416611406,-0.764832436764455,
-1.90434383078606));
#55567=CARTESIAN_POINT('Ctrl Pts',(-0.358298713291062,-0.705385003898168,
-1.90962695421773));
#55568=CARTESIAN_POINT('Ctrl Pts',(-0.475333260468061,-0.645937571031883,
-1.91491007764939));
#55569=CARTESIAN_POINT('Ctrl Pts',(-0.57725414082726,-0.556735764142692,
-1.92019320108105));
#55570=CARTESIAN_POINT('Ctrl Pts',(-0.65168577463767,-0.448610769827642,
-1.92547632451271));
#55571=CARTESIAN_POINT('Ctrl Pts',(-0.726117408448082,-0.340485775512588,
-1.93075944794437));
#55572=CARTESIAN_POINT('Ctrl Pts',(-0.773059795709701,-0.213437593771675,
-1.93604257137603));
#55573=CARTESIAN_POINT('Ctrl Pts',(-0.786813032200038,-0.0828928466795056,
-1.94132569480769));
#55574=CARTESIAN_POINT('Ctrl Pts',(-0.789712307396905,-0.055373131767919,
-1.94243941293056));
#55575=CARTESIAN_POINT('Ctrl Pts',(-0.791136673685564,-0.0276980312780681,
-1.94355313105343));
#55576=CARTESIAN_POINT('Ctrl Pts',(-0.791108239651095,-2.00188069073848E-5,
-1.9446668491763));
#55577=CARTESIAN_POINT('Ctrl Pts',(-0.791123285936247,-1.86130038508075E-5,
-1.97313315082371));
#55578=CARTESIAN_POINT('Ctrl Pts',(-0.791146127993088,-0.0228819780586756,
-1.9722131158099));
#55579=CARTESIAN_POINT('Ctrl Pts',(-0.790174710677041,-0.0457434085281455,
-1.97129308079609));
#55580=CARTESIAN_POINT('Ctrl Pts',(-0.788195003339531,-0.0685171891168216,
-1.97037304578228));
#55581=CARTESIAN_POINT('Ctrl Pts',(-0.776826916184554,-0.199291227114849,
-1.96508992235062));
#55582=CARTESIAN_POINT('Ctrl Pts',(-0.732211384296917,-0.32717509015776,
-1.95980679891896));
#55583=CARTESIAN_POINT('Ctrl Pts',(-0.659765777210421,-0.436640684906712,
-1.9545236754873));
#55584=CARTESIAN_POINT('Ctrl Pts',(-0.587320170123928,-0.54610627965566,
-1.94924055205564));
#55585=CARTESIAN_POINT('Ctrl Pts',(-0.487044487838577,-0.637153606110648,
-1.94395742862397));
#55586=CARTESIAN_POINT('Ctrl Pts',(-0.371114544543066,-0.698727388415873,
-1.93867430519231));
#55587=CARTESIAN_POINT('Ctrl Pts',(-0.255184601247555,-0.760301170721097,
-1.93339118176065));
#55588=CARTESIAN_POINT('Ctrl Pts',(-0.123600396941884,-0.792401408876558,
-1.92810805832899));
#55589=CARTESIAN_POINT('Ctrl Pts',(0.00766066702120217,-0.791130382853967,
-1.92282493489733));
#55590=CARTESIAN_POINT('Ctrl Pts',(0.138921730984293,-0.789859356831376,
-1.91754181146567));
#55591=CARTESIAN_POINT('Ctrl Pts',(0.269859654604797,-0.755217066630731,
-1.91225868803401));
#55592=CARTESIAN_POINT('Ctrl Pts',(0.384575510127528,-0.691409896880299,
-1.90697556460235));
#55593=CARTESIAN_POINT('Ctrl Pts',(0.499291365650253,-0.62760272712987,
-1.90169244117069));
#55594=CARTESIAN_POINT('Ctrl Pts',(0.597785153075204,-0.534630677829657,
-1.89640931773903));
#55595=CARTESIAN_POINT('Ctrl Pts',(0.66809742194445,-0.423782731225629,
-1.89112619430737));
#55596=CARTESIAN_POINT('Ctrl Pts',(0.738409690813698,-0.312934784621595,
-1.88584307087571));
#55597=CARTESIAN_POINT('Ctrl Pts',(0.780540441127239,-0.18421094071374,
-1.88055994744405));
#55598=CARTESIAN_POINT('Ctrl Pts',(0.789374013975979,-0.0532412861727047,
-1.87527682401239));
#55599=CARTESIAN_POINT('Ctrl Pts',(0.79820758682472,0.0777283683683321,
-1.86999370058073));
#55600=CARTESIAN_POINT('Ctrl Pts',(0.773743982208662,0.210943833542553,
-1.86471057714907));
#55601=CARTESIAN_POINT('Ctrl Pts',(0.718953654154168,0.330229634757758,
-1.85942745371741));
#55602=CARTESIAN_POINT('Ctrl Pts',(0.664163326099674,0.449515435972964,
-1.85414433028575));
#55603=CARTESIAN_POINT('Ctrl Pts',(0.579046274606745,0.554871573229153,
-1.84886120685409));
#55604=CARTESIAN_POINT('Ctrl Pts',(0.473937701387782,0.63350534622617,-1.84357808342243));
#55605=CARTESIAN_POINT('Ctrl Pts',(0.368829128168824,0.712139119223182,
-1.83829495999077));
#55606=CARTESIAN_POINT('Ctrl Pts',(0.243729033223835,0.764050527961024,
-1.83301183655911));
#55607=CARTESIAN_POINT('Ctrl Pts',(0.113827495306941,0.782936312739435,
-1.82772871312745));
#55608=CARTESIAN_POINT('Ctrl Pts',(-0.0160740426099603,0.801822097517847,
-1.82244558969579));
#55609=CARTESIAN_POINT('Ctrl Pts',(-0.150777023498765,0.787682258336824,
-1.81716246626413));
#55610=CARTESIAN_POINT('Ctrl Pts',(-0.273925353553017,0.742233702532247,
-1.81187934283247));
#55611=CARTESIAN_POINT('Ctrl Pts',(-0.397073683607268,0.696785146727671,
-1.80659621940081));
#55612=CARTESIAN_POINT('Ctrl Pts',(-0.508667362826965,0.620027874299541,
-1.80131309596915));
#55613=CARTESIAN_POINT('Ctrl Pts',(-0.595156307364805,0.521282014170606,
-1.79602997253749));
#55614=CARTESIAN_POINT('Ctrl Pts',(-0.681645251902642,0.422536154041674,
-1.79074684910583));
#55615=CARTESIAN_POINT('Ctrl Pts',(-0.743029461758622,0.30180170621194,
-1.78546372567417));
#55616=CARTESIAN_POINT('Ctrl Pts',(-0.771855457521859,0.17373865772359,
-1.78018060224251));
#55617=CARTESIAN_POINT('Ctrl Pts',(-0.784672989130951,0.116795189562486,
-1.77783145176958));
#55618=CARTESIAN_POINT('Ctrl Pts',(-0.79105326546298,0.0584027453264418,
-1.77548230129664));
#55619=CARTESIAN_POINT('Ctrl Pts',(-0.791036127465933,6.61336014326832E-6,
-1.77313315082371));
#55620=CARTESIAN_POINT('Origin',(0.,0.,-1.94));
#55621=CARTESIAN_POINT('',(-0.791166035532024,3.68633254679493E-6,-1.5446668491763));
#55622=CARTESIAN_POINT('',(-0.791159979474253,8.47231515970201E-6,-1.5731331508237));
#55623=CARTESIAN_POINT('',(-0.7911,-9.68818082805471E-17,-1.94));
#55624=CARTESIAN_POINT('Ctrl Pts',(-0.791166035532024,3.68633254679493E-6,
-1.5446668491763));
#55625=CARTESIAN_POINT('Ctrl Pts',(-0.791166952605422,0.00352021813421264,
-1.54480837859526));
#55626=CARTESIAN_POINT('Ctrl Pts',(-0.79114399565106,0.007036737919245,
-1.54494990801422));
#55627=CARTESIAN_POINT('Ctrl Pts',(-0.791097090858486,0.0105529382491046,
-1.54509143743318));
#55628=CARTESIAN_POINT('Ctrl Pts',(-0.789346191218509,0.141808478542717,
-1.55037456086484));
#55629=CARTESIAN_POINT('Ctrl Pts',(-0.754225431715114,0.272618877431325,
-1.5556576842965));
#55630=CARTESIAN_POINT('Ctrl Pts',(-0.689999294345667,0.387100691646154,
-1.56094080772816));
#55631=CARTESIAN_POINT('Ctrl Pts',(-0.625773156976222,0.501582505860979,
-1.56622393115982));
#55632=CARTESIAN_POINT('Ctrl Pts',(-0.532441641740725,0.599735735402025,
-1.57150705459148));
#55633=CARTESIAN_POINT('Ctrl Pts',(-0.421337378460864,0.669642281507206,
-1.57679017802314));
#55634=CARTESIAN_POINT('Ctrl Pts',(-0.310233115181003,0.739548827612388,
-1.5820733014548));
#55635=CARTESIAN_POINT('Ctrl Pts',(-0.181356103856777,0.781208690281705,
-1.58735642488646));
#55636=CARTESIAN_POINT('Ctrl Pts',(-0.0503550292671448,0.789563387384417,
-1.59263954831812));
#55637=CARTESIAN_POINT('Ctrl Pts',(0.0806460453224916,0.797918084487129,
-1.59792267174978));
#55638=CARTESIAN_POINT('Ctrl Pts',(0.213771183177535,0.772967616023235,
-1.60320579518144));
#55639=CARTESIAN_POINT('Ctrl Pts',(0.33285587755591,0.717741552682394,-1.6084889186131));
#55640=CARTESIAN_POINT('Ctrl Pts',(0.451940571934281,0.662515489341555,
-1.61377204204476));
#55641=CARTESIAN_POINT('Ctrl Pts',(0.556984822835985,0.577013831123771,
-1.61905516547642));
#55642=CARTESIAN_POINT('Ctrl Pts',(0.635233800262155,0.471618479997285,
-1.62433828890808));
#55643=CARTESIAN_POINT('Ctrl Pts',(0.713482777688325,0.366223128870799,
-1.62962141233974));
#55644=CARTESIAN_POINT('Ctrl Pts',(0.764936481638961,0.240934084835611,
-1.6349045357714));
#55645=CARTESIAN_POINT('Ctrl Pts',(0.783347228484842,0.110964369486637,
-1.64018765920306));
#55646=CARTESIAN_POINT('Ctrl Pts',(0.801757975330723,-0.0190053458623417,
-1.64547078263472));
#55647=CARTESIAN_POINT('Ctrl Pts',(0.787125765071846,-0.153655732525106,
-1.65075390606638));
#55648=CARTESIAN_POINT('Ctrl Pts',(0.741227290413978,-0.276637082864898,
-1.65603702949804));
#55649=CARTESIAN_POINT('Ctrl Pts',(0.695328815756111,-0.39961843320469,
-1.6613201529297));
#55650=CARTESIAN_POINT('Ctrl Pts',(0.618164076699251,-0.510930747221509,
-1.66660327636136));
#55651=CARTESIAN_POINT('Ctrl Pts',(0.519102678149224,-0.597058105387367,
-1.67188639979302));
#55652=CARTESIAN_POINT('Ctrl Pts',(0.4200412795992,-0.683185463553224,-1.67716952322468));
#55653=CARTESIAN_POINT('Ctrl Pts',(0.299083221556008,-0.744127865868122,
-1.68245264665634));
#55654=CARTESIAN_POINT('Ctrl Pts',(0.170915642574026,-0.772485478694556,
-1.687735770088));
#55655=CARTESIAN_POINT('Ctrl Pts',(0.0427480635920437,-0.80084309152099,
-1.69301889351966));
#55656=CARTESIAN_POINT('Ctrl Pts',(-0.092629036328729,-0.79661591485896,
-1.69830201695132));
#55657=CARTESIAN_POINT('Ctrl Pts',(-0.218777709557586,-0.760317226867303,
-1.70358514038298));
#55658=CARTESIAN_POINT('Ctrl Pts',(-0.344926382786443,-0.724018538875647,
-1.70886826381464));
#55659=CARTESIAN_POINT('Ctrl Pts',(-0.461846629323384,-0.655648339554364,
-1.7141513872463));
#55660=CARTESIAN_POINT('Ctrl Pts',(-0.555341595411988,-0.563508370901193,
-1.71943451067796));
#55661=CARTESIAN_POINT('Ctrl Pts',(-0.648836561500592,-0.471368402248023,
-1.72471763410962));
#55662=CARTESIAN_POINT('Ctrl Pts',(-0.71890624714086,-0.355458664262964,
-1.73000075754128));
#55663=CARTESIAN_POINT('Ctrl Pts',(-0.757042552929503,-0.229853311319263,
-1.73528388097294));
#55664=CARTESIAN_POINT('Ctrl Pts',(-0.779619585199458,-0.155493825049006,
-1.73841153704073));
#55665=CARTESIAN_POINT('Ctrl Pts',(-0.791004781097966,-0.0777362726597893,
-1.74153919310851));
#55666=CARTESIAN_POINT('Ctrl Pts',(-0.791041867722209,1.06520765539853E-5,
-1.74466684917629));
#55667=CARTESIAN_POINT('Ctrl Pts',(-0.791036127465933,6.61336014326832E-6,
-1.77313315082371));
#55668=CARTESIAN_POINT('Ctrl Pts',(-0.791014722953756,-0.0729272723390494,
-1.77019917786498));
#55669=CARTESIAN_POINT('Ctrl Pts',(-0.781014134674409,-0.145866910446324,
-1.76726520490626));
#55670=CARTESIAN_POINT('Ctrl Pts',(-0.761111981169042,-0.215996575470099,
-1.76433123194753));
#55671=CARTESIAN_POINT('Ctrl Pts',(-0.725274727382491,-0.342277111028477,
-1.75904810851587));
#55672=CARTESIAN_POINT('Ctrl Pts',(-0.657332438138893,-0.459446532998264,
-1.75376498508421));
#55673=CARTESIAN_POINT('Ctrl Pts',(-0.56553489713985,-0.553277731895016,
-1.74848186165255));
#55674=CARTESIAN_POINT('Ctrl Pts',(-0.473737356140807,-0.647108930791767,
-1.74319873822089));
#55675=CARTESIAN_POINT('Ctrl Pts',(-0.358084563386321,-0.717601906615482,
-1.73791561478923));
#55676=CARTESIAN_POINT('Ctrl Pts',(-0.232619474086362,-0.756197162629997,
-1.73263249135757));
#55677=CARTESIAN_POINT('Ctrl Pts',(-0.107154384786411,-0.79479241864451,
-1.72734936792591));
#55678=CARTESIAN_POINT('Ctrl Pts',(0.0281230010590105,-0.801489954849828,
-1.72206624449425));
#55679=CARTESIAN_POINT('Ctrl Pts',(0.156786843441164,-0.775476533634403,
-1.71678312106259));
#55680=CARTESIAN_POINT('Ctrl Pts',(0.285450685823325,-0.749463112418977,
-1.71149999763093));
#55681=CARTESIAN_POINT('Ctrl Pts',(0.407500984742214,-0.690738733782805,
-1.70621687419927));
#55682=CARTESIAN_POINT('Ctrl Pts',(0.50811797804371,-0.606433911389069,
-1.70093375076761));
#55683=CARTESIAN_POINT('Ctrl Pts',(0.608734971345201,-0.522129088995338,
-1.69565062733595));
#55684=CARTESIAN_POINT('Ctrl Pts',(0.687918659029299,-0.412243822844049,
-1.69036750390429));
#55685=CARTESIAN_POINT('Ctrl Pts',(0.736054288585285,-0.290120755460693,
-1.68508438047263));
#55686=CARTESIAN_POINT('Ctrl Pts',(0.784189918141273,-0.167997688077334,
-1.67980125704097));
#55687=CARTESIAN_POINT('Ctrl Pts',(0.801277489569146,-0.0336368194619003,
-1.67451813360931));
#55688=CARTESIAN_POINT('Ctrl Pts',(0.785242171864016,0.096647297014235,
-1.66923501017765));
#55689=CARTESIAN_POINT('Ctrl Pts',(0.769206854158885,0.226931413490374,
-1.66395188674599));
#55690=CARTESIAN_POINT('Ctrl Pts',(0.720048647320751,0.353138777827222,
-1.65866876331433));
#55691=CARTESIAN_POINT('Ctrl Pts',(0.643736507916843,0.459944862857389,
-1.65338563988267));
#55692=CARTESIAN_POINT('Ctrl Pts',(0.567424368512935,0.566750947887556,
-1.64810251645101));
#55693=CARTESIAN_POINT('Ctrl Pts',(0.463958296543255,0.65415575361104,-1.64281939301935));
#55694=CARTESIAN_POINT('Ctrl Pts',(0.345901494156378,0.711546291420495,
-1.63753626958769));
#55695=CARTESIAN_POINT('Ctrl Pts',(0.227844691769501,0.768936829229949,
-1.63225314615603));
#55696=CARTESIAN_POINT('Ctrl Pts',(0.095197158965428,0.796313099125374,
-1.62697002272437));
#55697=CARTESIAN_POINT('Ctrl Pts',(-0.0359345899424767,0.790350981361787,
-1.62168689929271));
#55698=CARTESIAN_POINT('Ctrl Pts',(-0.167066338850374,0.7843888635982,-1.61640377586105));
#55699=CARTESIAN_POINT('Ctrl Pts',(-0.296682303862101,0.745088358175606,
-1.61112065242939));
#55700=CARTESIAN_POINT('Ctrl Pts',(-0.4090440739302,0.67722146604819,-1.60583752899773));
#55701=CARTESIAN_POINT('Ctrl Pts',(-0.521405843998305,0.609354573920769,
-1.60055440556607));
#55702=CARTESIAN_POINT('Ctrl Pts',(-0.616513419122778,0.512921295088524,
-1.59527128213441));
#55703=CARTESIAN_POINT('Ctrl Pts',(-0.682818514253234,0.399630886052217,
-1.58998815870275));
#55704=CARTESIAN_POINT('Ctrl Pts',(-0.749123609383688,0.286340477015913,
-1.58470503527108));
#55705=CARTESIAN_POINT('Ctrl Pts',(-0.786626224520126,0.15619293777555,
-1.57942191183943));
#55706=CARTESIAN_POINT('Ctrl Pts',(-0.790772664658091,0.0249912249282936,
-1.57413878840777));
#55707=CARTESIAN_POINT('Ctrl Pts',(-0.79103575498693,0.0166665173167768,
-1.57380357587975));
#55708=CARTESIAN_POINT('Ctrl Pts',(-0.791164557932427,0.00833756574697465,
-1.57346836335172));
#55709=CARTESIAN_POINT('Ctrl Pts',(-0.791159979474253,8.47231515970201E-6,
-1.5731331508237));
#55710=CARTESIAN_POINT('Origin',(0.,0.,-1.94));
#55711=CARTESIAN_POINT('',(-0.791054873532962,-1.56092113809958E-5,-1.34466684917629));
#55712=CARTESIAN_POINT('',(-0.791066487406845,-1.81135318691069E-5,-1.3731331508237));
#55713=CARTESIAN_POINT('',(-0.7911,-9.68818082805471E-17,-1.94));
#55714=CARTESIAN_POINT('Ctrl Pts',(-0.791054873532962,-1.56092113809958E-5,
-1.34466684917629));
#55715=CARTESIAN_POINT('Ctrl Pts',(-0.790994308958492,0.0847635680099431,
-1.348077564082));
#55716=CARTESIAN_POINT('Ctrl Pts',(-0.777416502544745,0.169561683102478,
-1.35148827898771));
#55717=CARTESIAN_POINT('Ctrl Pts',(-0.750641953334654,0.249965256714577,
-1.35489899389341));
#55718=CARTESIAN_POINT('Ctrl Pts',(-0.709168757182336,0.37450864878428,
-1.36018211732507));
#55719=CARTESIAN_POINT('Ctrl Pts',(-0.636032169671575,0.488508068838821,
-1.36546524075673));
#55720=CARTESIAN_POINT('Ctrl Pts',(-0.540112683855437,0.578121319801412,
-1.37074836418839));
#55721=CARTESIAN_POINT('Ctrl Pts',(-0.444193198039299,0.667734570764002,
-1.37603148762005));
#55722=CARTESIAN_POINT('Ctrl Pts',(-0.325490813917783,0.732961652634642,
-1.38131461105171));
#55723=CARTESIAN_POINT('Ctrl Pts',(-0.198418778450467,0.765882471420174,
-1.38659773448337));
#55724=CARTESIAN_POINT('Ctrl Pts',(-0.0713467429831482,0.798803290205708,
-1.39188085791503));
#55725=CARTESIAN_POINT('Ctrl Pts',(0.0640949438299711,0.799417845906132,
-1.39716398134669));
#55726=CARTESIAN_POINT('Ctrl Pts',(0.191460491998178,0.767651517079374,
-1.40244710477835));
#55727=CARTESIAN_POINT('Ctrl Pts',(0.318826040166385,0.735885188252617,
-1.40773022821001));
#55728=CARTESIAN_POINT('Ctrl Pts',(0.43811544968968,0.671737974898678,-1.41301335164167));
#55729=CARTESIAN_POINT('Ctrl Pts',(0.53484419498885,0.58299884970485,-1.41829647507333));
#55730=CARTESIAN_POINT('Ctrl Pts',(0.631572940288017,0.494259724511026,
-1.42357959850499));
#55731=CARTESIAN_POINT('Ctrl Pts',(0.705741021363061,0.380928687477314,
-1.42886272193665));
#55732=CARTESIAN_POINT('Ctrl Pts',(0.748342697706208,0.256766778342223,
-1.43414584536831));
#55733=CARTESIAN_POINT('Ctrl Pts',(0.790944374049354,0.132604869207133,
-1.43942896879997));
#55734=CARTESIAN_POINT('Ctrl Pts',(0.801979645660603,-0.00238791202933467,
-1.44471209223163));
#55735=CARTESIAN_POINT('Ctrl Pts',(0.780108572351085,-0.131820283017454,
-1.44999521566329));
#55736=CARTESIAN_POINT('Ctrl Pts',(0.758237499041567,-0.261252654005574,
-1.45527833909495));
#55737=CARTESIAN_POINT('Ctrl Pts',(0.703460080811282,-0.385124614745345,
-1.46056146252661));
#55738=CARTESIAN_POINT('Ctrl Pts',(0.622427577974875,-0.488395210712369,
-1.46584458595827));
#55739=CARTESIAN_POINT('Ctrl Pts',(0.541395075138469,-0.591665806679393,
-1.47112770938993));
#55740=CARTESIAN_POINT('Ctrl Pts',(0.434107487695941,-0.674335037873671,
-1.47641083282159));
#55741=CARTESIAN_POINT('Ctrl Pts',(0.313592039194238,-0.726364925243813,
-1.48169395625325));
#55742=CARTESIAN_POINT('Ctrl Pts',(0.193076590692534,-0.778394812613955,
-1.48697707968491));
#55743=CARTESIAN_POINT('Ctrl Pts',(0.059333281131654,-0.799785356159962,
-1.49226020311657));
#55744=CARTESIAN_POINT('Ctrl Pts',(-0.0713983222365862,-0.787939243376194,
-1.49754332654823));
#55745=CARTESIAN_POINT('Ctrl Pts',(-0.202129925604834,-0.776093130592426,
-1.50282644997989));
#55746=CARTESIAN_POINT('Ctrl Pts',(-0.329849822780441,-0.731010361478878,
-1.50810957341156));
#55747=CARTESIAN_POINT('Ctrl Pts',(-0.439049829717504,-0.658165039101501,
-1.51339269684322));
#55748=CARTESIAN_POINT('Ctrl Pts',(-0.54824983665456,-0.585319716724129,
-1.51867582027488));
#55749=CARTESIAN_POINT('Ctrl Pts',(-0.638929953353074,-0.48471184108293,
-1.52395894370654));
#55750=CARTESIAN_POINT('Ctrl Pts',(-0.70007949181405,-0.368557562413024,
-1.5292420671382));
#55751=CARTESIAN_POINT('Ctrl Pts',(-0.759590897310686,-0.25551493687456,
-1.5343836611509));
#55752=CARTESIAN_POINT('Ctrl Pts',(-0.791132719355588,-0.127747695604292,
-1.5395252551636));
#55753=CARTESIAN_POINT('Ctrl Pts',(-0.791166035532024,3.68633254679493E-6,
-1.5446668491763));
#55754=CARTESIAN_POINT('Ctrl Pts',(-0.791159979474253,8.47231515970201E-6,
-1.5731331508237));
#55755=CARTESIAN_POINT('Ctrl Pts',(-0.791092399055183,-0.122933269904619,
-1.56818523992006));
#55756=CARTESIAN_POINT('Ctrl Pts',(-0.761964622417966,-0.245905920015694,
-1.56323732901642));
#55757=CARTESIAN_POINT('Ctrl Pts',(-0.706690205369702,-0.355717475151843,
-1.55828941811278));
#55758=CARTESIAN_POINT('Ctrl Pts',(-0.647671040803863,-0.472968575930565,
-1.55300629468112));
#55759=CARTESIAN_POINT('Ctrl Pts',(-0.558842446532696,-0.57521489103386,
-1.54772317124947));
#55760=CARTESIAN_POINT('Ctrl Pts',(-0.450990292408587,-0.650041325337929,
-1.5424400478178));
#55761=CARTESIAN_POINT('Ctrl Pts',(-0.343138138284478,-0.724867759641997,
-1.53715692438614));
#55762=CARTESIAN_POINT('Ctrl Pts',(-0.216262424307427,-0.772274313146837,
-1.53187380095448));
#55763=CARTESIAN_POINT('Ctrl Pts',(-0.0857688309299165,-0.786504720986968,
-1.52659067752282));
#55764=CARTESIAN_POINT('Ctrl Pts',(0.0447247624475942,-0.800735128827099,
-1.52130755409116));
#55765=CARTESIAN_POINT('Ctrl Pts',(0.178836235225564,-0.781789391002521,
-1.5160244306595));
#55766=CARTESIAN_POINT('Ctrl Pts',(0.300281316522941,-0.731967963398073,
-1.51074130722784));
#55767=CARTESIAN_POINT('Ctrl Pts',(0.421726397820321,-0.682146535793625,
-1.50545818379618));
#55768=CARTESIAN_POINT('Ctrl Pts',(0.530505087637106,-0.601449418409306,
-1.50017506036452));
#55769=CARTESIAN_POINT('Ctrl Pts',(0.613409107707684,-0.499675129534317,
-1.49489193693286));
#55770=CARTESIAN_POINT('Ctrl Pts',(0.696313127778262,-0.397900840659328,
-1.4896088135012));
#55771=CARTESIAN_POINT('Ctrl Pts',(0.753342478102633,-0.275049380293668,
-1.48432569006954));
#55772=CARTESIAN_POINT('Ctrl Pts',(0.777572461116777,-0.146037790337545,
-1.47904256663788));
#55773=CARTESIAN_POINT('Ctrl Pts',(0.80180244413092,-0.0170262003814258,
-1.47375944320622));
#55774=CARTESIAN_POINT('Ctrl Pts',(0.793233059834839,0.118145519165157,
-1.46847631977456));
#55775=CARTESIAN_POINT('Ctrl Pts',(0.752904831997833,0.243064358654635,
-1.4631931963429));
#55776=CARTESIAN_POINT('Ctrl Pts',(0.712576604160826,0.367983198144114,
-1.45791007291124));
#55777=CARTESIAN_POINT('Ctrl Pts',(0.640489532782895,0.482649157576488,
-1.45262694947958));
#55778=CARTESIAN_POINT('Ctrl Pts',(0.545396675100861,0.573139106398089,
-1.44734382604792));
#55779=CARTESIAN_POINT('Ctrl Pts',(0.450303817418827,0.663629055219689,
-1.44206070261626));
#55780=CARTESIAN_POINT('Ctrl Pts',(0.332205173432689,0.729942993430516,
-1.4367775791846));
#55781=CARTESIAN_POINT('Ctrl Pts',(0.205440681922623,0.76402885724627,-1.43149445575294));
#55782=CARTESIAN_POINT('Ctrl Pts',(0.0786761904125578,0.798114721062024,
-1.42621133232128));
#55783=CARTESIAN_POINT('Ctrl Pts',(-0.0567541486214352,0.799972510482705,
-1.42092820888962));
#55784=CARTESIAN_POINT('Ctrl Pts',(-0.184405923074557,0.769376646402069,
-1.41564508545796));
#55785=CARTESIAN_POINT('Ctrl Pts',(-0.312057697527683,0.738780782321432,
-1.4103619620263));
#55786=CARTESIAN_POINT('Ctrl Pts',(-0.431930907399938,0.675731264739476,
-1.40507883859464));
#55787=CARTESIAN_POINT('Ctrl Pts',(-0.529470140089352,0.587883780391699,
-1.39979571516298));
#55788=CARTESIAN_POINT('Ctrl Pts',(-0.627009372778766,0.500036296043922,
-1.39451259173132));
#55789=CARTESIAN_POINT('Ctrl Pts',(-0.702214628285339,0.387390844930324,
-1.38922946829966));
#55790=CARTESIAN_POINT('Ctrl Pts',(-0.745954228856374,0.263625220616629,
-1.383946344868));
#55791=CARTESIAN_POINT('Ctrl Pts',(-0.775795464160492,0.179186426720742,
-1.38034194685324));
#55792=CARTESIAN_POINT('Ctrl Pts',(-0.790990641636737,0.0895716178943466,
-1.37673754883847));
#55793=CARTESIAN_POINT('Ctrl Pts',(-0.791066487406845,-1.81135318691069E-5,
-1.3731331508237));
#55794=CARTESIAN_POINT('Origin',(0.,0.,-1.94));
#55795=CARTESIAN_POINT('',(-0.791086342131762,2.01490389672293E-5,-1.1446668491763));
#55796=CARTESIAN_POINT('',(-0.79107238223822,1.89686955811942E-5,-1.1731331508237));
#55797=CARTESIAN_POINT('',(-0.7911,-9.68818082805471E-17,-1.94));
#55798=CARTESIAN_POINT('Ctrl Pts',(-0.791086342131762,2.01490389672293E-5,
-1.1446668491763));
#55799=CARTESIAN_POINT('Ctrl Pts',(-0.791120376438806,0.0347354763001229,
-1.14606362613709));
#55800=CARTESIAN_POINT('Ctrl Pts',(-0.788877432756344,0.0694464381092138,
-1.14746040309788));
#55801=CARTESIAN_POINT('Ctrl Pts',(-0.784321936747084,0.103851197430517,
-1.14885718005867));
#55802=CARTESIAN_POINT('Ctrl Pts',(-0.767091377835423,0.233982632321972,
-1.15414030349033));
#55803=CARTESIAN_POINT('Ctrl Pts',(-0.716776746918577,0.35973344194638,
-1.15942342692199));
#55804=CARTESIAN_POINT('Ctrl Pts',(-0.6394874175062,0.465834535561396,-1.16470655035365));
#55805=CARTESIAN_POINT('Ctrl Pts',(-0.562198088093824,0.571935629176409,
-1.16998967378531));
#55806=CARTESIAN_POINT('Ctrl Pts',(-0.457934060185918,0.658387006782034,
-1.17527279721697));
#55807=CARTESIAN_POINT('Ctrl Pts',(-0.339355426453396,0.714691448253778,
-1.18055592064863));
#55808=CARTESIAN_POINT('Ctrl Pts',(-0.220776792720872,0.770995889725524,
-1.18583904408029));
#55809=CARTESIAN_POINT('Ctrl Pts',(-0.0878835531637302,0.797153395063388,
-1.19112216751195));
#55810=CARTESIAN_POINT('Ctrl Pts',(0.0431879433555249,0.78998783105765,
-1.19640529094361));
#55811=CARTESIAN_POINT('Ctrl Pts',(0.174259439874776,0.782822267051912,
-1.20168841437527));
#55812=CARTESIAN_POINT('Ctrl Pts',(0.303509193356143,0.742333633702575,
-1.20697153780693));
#55813=CARTESIAN_POINT('Ctrl Pts',(0.415243259400964,0.673438198495239,
-1.21225466123859));
#55814=CARTESIAN_POINT('Ctrl Pts',(0.52697732544578,0.604542763287905,-1.21753778467025));
#55815=CARTESIAN_POINT('Ctrl Pts',(0.621195704054054,0.507240526222574,
-1.22282090810191));
#55816=CARTESIAN_POINT('Ctrl Pts',(0.686458079438849,0.393346255662332,
-1.22810403153357));
#55817=CARTESIAN_POINT('Ctrl Pts',(0.751720454823647,0.279451985102084,
-1.23338715496523));
#55818=CARTESIAN_POINT('Ctrl Pts',(0.788026826984966,0.148965681046922,
-1.23867027839689));
#55819=CARTESIAN_POINT('Ctrl Pts',(0.790968752806516,0.017731434069321,
-1.24395340182855));
#55820=CARTESIAN_POINT('Ctrl Pts',(0.793910678628066,-0.113502812908284,
-1.24923652526021));
#55821=CARTESIAN_POINT('Ctrl Pts',(0.763488158109848,-0.245485002808319,
-1.25451964869187));
#55822=CARTESIAN_POINT('Ctrl Pts',(0.703395197101927,-0.362189409514402,
-1.25980277212353));
#55823=CARTESIAN_POINT('Ctrl Pts',(0.643302236094011,-0.478893816220475,
-1.26508589555519));
#55824=CARTESIAN_POINT('Ctrl Pts',(0.553538834596398,-0.58032043973259,
-1.27036901898685));
#55825=CARTESIAN_POINT('Ctrl Pts',(0.445004369932397,-0.654153714666148,
-1.27565214241851));
#55826=CARTESIAN_POINT('Ctrl Pts',(0.33646990526839,-0.727986989599709,
-1.28093526585017));
#55827=CARTESIAN_POINT('Ctrl Pts',(0.209164377437992,-0.774226915954711,
-1.28621838928183));
#55828=CARTESIAN_POINT('Ctrl Pts',(0.0785456563527366,-0.787258884699669,
-1.29150151271349));
#55829=CARTESIAN_POINT('Ctrl Pts',(-0.0520730647325192,-0.800290853444627,
-1.29678463614515));
#55830=CARTESIAN_POINT('Ctrl Pts',(-0.186004979072635,-0.780114864579541,
-1.30206775957681));
#55831=CARTESIAN_POINT('Ctrl Pts',(-0.306987618382414,-0.729180755252319,
-1.30735088300847));
#55832=CARTESIAN_POINT('Ctrl Pts',(-0.42797025769219,-0.678246645925099,
-1.31263400644013));
#55833=CARTESIAN_POINT('Ctrl Pts',(-0.536003621971631,-0.596554416135744,
-1.31791712987179));
#55834=CARTESIAN_POINT('Ctrl Pts',(-0.617969932915293,-0.494023414104147,
-1.32320025330345));
#55835=CARTESIAN_POINT('Ctrl Pts',(-0.699936243858955,-0.39149241207255,
-1.32848337673511));
#55836=CARTESIAN_POINT('Ctrl Pts',(-0.755835501466839,-0.268122637798709,
-1.33376650016677));
#55837=CARTESIAN_POINT('Ctrl Pts',(-0.778880227873844,-0.138894068619357,
-1.33904962359843));
#55838=CARTESIAN_POINT('Ctrl Pts',(-0.787047582424787,-0.0930937616876116,
-1.34092203212439));
#55839=CARTESIAN_POINT('Ctrl Pts',(-0.791088122171075,-0.0465575391707168,
-1.34279444065034));
#55840=CARTESIAN_POINT('Ctrl Pts',(-0.791054873532962,-1.56092113809958E-5,
-1.34466684917629));
#55841=CARTESIAN_POINT('Ctrl Pts',(-0.791066487406845,-1.81135318691069E-5,
-1.3731331508237));
#55842=CARTESIAN_POINT('Ctrl Pts',(-0.791101812091168,-0.0417439602951441,
-1.37145442540681));
#55843=CARTESIAN_POINT('Ctrl Pts',(-0.787857494745136,-0.0834643673407622,
-1.36977569998991));
#55844=CARTESIAN_POINT('Ctrl Pts',(-0.781285721563619,-0.124653879902264,
-1.36809697457302));
#55845=CARTESIAN_POINT('Ctrl Pts',(-0.760603668064331,-0.254281558593677,
-1.36281385114136));
#55846=CARTESIAN_POINT('Ctrl Pts',(-0.706965615430256,-0.378651118462714,
-1.3575307277097));
#55847=CARTESIAN_POINT('Ctrl Pts',(-0.626884478332546,-0.48266118480732,
-1.35224760427804));
#55848=CARTESIAN_POINT('Ctrl Pts',(-0.546803341234833,-0.586671251151929,
-1.34696448084638));
#55849=CARTESIAN_POINT('Ctrl Pts',(-0.440279119673483,-0.670321823972104,
-1.34168135741472));
#55850=CARTESIAN_POINT('Ctrl Pts',(-0.320246346715405,-0.723455766380578,
-1.33639823398306));
#55851=CARTESIAN_POINT('Ctrl Pts',(-0.200213573757331,-0.776589708789051,
-1.3311151105514));
#55852=CARTESIAN_POINT('Ctrl Pts',(-0.0666722494025287,-0.799207020785824,
-1.32583198711974));
#55853=CARTESIAN_POINT('Ctrl Pts',(0.0641625848274726,-0.788561431470073,
-1.32054886368808));
#55854=CARTESIAN_POINT('Ctrl Pts',(0.194997419057474,-0.777915842154323,
-1.31526574025642));
#55855=CARTESIAN_POINT('Ctrl Pts',(0.323125763162674,-0.734007351526049,
-1.30998261682476));
#55856=CARTESIAN_POINT('Ctrl Pts',(0.432989838082634,-0.662167477766046,
-1.3046994933931));
#55857=CARTESIAN_POINT('Ctrl Pts',(0.542853913002597,-0.590327604006042,
-1.29941636996144));
#55858=CARTESIAN_POINT('Ctrl Pts',(0.634453718737318,-0.490556347114309,
-1.29413324652978));
#55859=CARTESIAN_POINT('Ctrl Pts',(0.696666895518923,-0.374968272233665,
-1.28885012309812));
#55860=CARTESIAN_POINT('Ctrl Pts',(0.758880072300526,-0.259380197353024,
-1.28356699966646));
#55861=CARTESIAN_POINT('Ctrl Pts',(0.791706620129014,-0.127975304483475,
-1.2782838762348));
#55862=CARTESIAN_POINT('Ctrl Pts',(0.791160627986813,0.00329077762630802,
-1.27300075280314));
#55863=CARTESIAN_POINT('Ctrl Pts',(0.790614635844611,0.134556859736091,
-1.26771762937148));
#55864=CARTESIAN_POINT('Ctrl Pts',(0.75669610373172,0.265684131086106,-1.26243450593982));
#55865=CARTESIAN_POINT('Ctrl Pts',(0.693523535109274,0.38075067267624,-1.25715138250816));
#55866=CARTESIAN_POINT('Ctrl Pts',(0.630350966486827,0.495817214266377,
-1.2518682590765));
#55867=CARTESIAN_POINT('Ctrl Pts',(0.537924361354823,0.59482302609663,-1.24658513564484));
#55868=CARTESIAN_POINT('Ctrl Pts',(0.427466472274317,0.665746485965359,
-1.24130201221318));
#55869=CARTESIAN_POINT('Ctrl Pts',(0.317008583193811,0.736669945834088,
-1.23601888878152));
#55870=CARTESIAN_POINT('Ctrl Pts',(0.188519410164803,0.779511053741293,
-1.23073576534986));
#55871=CARTESIAN_POINT('Ctrl Pts',(0.0576005453221517,0.789067896744294,
-1.2254526419182));
#55872=CARTESIAN_POINT('Ctrl Pts',(-0.0733183195204963,0.798624739747296,
-1.22016951848654));
#55873=CARTESIAN_POINT('Ctrl Pts',(-0.206666876176788,0.774897317846096,
-1.21488639505488));
#55874=CARTESIAN_POINT('Ctrl Pts',(-0.326253489634383,0.720766695259472,
-1.20960327162322));
#55875=CARTESIAN_POINT('Ctrl Pts',(-0.445840103091977,0.666636072672849,
-1.20432014819156));
#55876=CARTESIAN_POINT('Ctrl Pts',(-0.551664773350874,0.582102249400802,
-1.1990370247599));
#55877=CARTESIAN_POINT('Ctrl Pts',(-0.630877909241144,0.47742960960271,
-1.19375390132824));
#55878=CARTESIAN_POINT('Ctrl Pts',(-0.710091045131417,0.372756969804615,
-1.18847077789658));
#55879=CARTESIAN_POINT('Ctrl Pts',(-0.762692646653061,0.247945513480473,
-1.18318765446492));
#55880=CARTESIAN_POINT('Ctrl Pts',(-0.782295648551982,0.118150271901965,
-1.17790453103326));
#55881=CARTESIAN_POINT('Ctrl Pts',(-0.788197042334037,0.0790760099322191,
-1.17631407096341));
#55882=CARTESIAN_POINT('Ctrl Pts',(-0.791107827808171,0.0395500757776835,
-1.17472361089355));
#55883=CARTESIAN_POINT('Ctrl Pts',(-0.79107238223822,1.89686955811942E-5,
-1.1731331508237));
#55884=CARTESIAN_POINT('Origin',(0.,0.,-1.94));
#55885=CARTESIAN_POINT('',(-0.791144809354952,-1.43559245109892E-5,-0.944666849176295));
#55886=CARTESIAN_POINT('',(-0.791155923841092,-1.04795641788954E-5,-0.973133150823705));
#55887=CARTESIAN_POINT('',(-0.7911,-9.68818082805471E-17,-1.94));
#55888=CARTESIAN_POINT('Ctrl Pts',(-0.791144809354952,-1.43559245109892E-5,
-0.944666849176295));
#55889=CARTESIAN_POINT('Ctrl Pts',(-0.791047376981328,0.115928204571859,
-0.949332811623831));
#55890=CARTESIAN_POINT('Ctrl Pts',(-0.76524696255707,0.231912697319003,
-0.953998774071366));
#55891=CARTESIAN_POINT('Ctrl Pts',(-0.715892089735664,0.336815212727028,
-0.958664736518902));
#55892=CARTESIAN_POINT('Ctrl Pts',(-0.660009109964346,0.455593051902503,
-0.963947859950562));
#55893=CARTESIAN_POINT('Ctrl Pts',(-0.573928548900091,0.5601634359142,-0.969230983382222));
#55894=CARTESIAN_POINT('Ctrl Pts',(-0.468102600862498,0.637829073291751,
-0.974514106813882));
#55895=CARTESIAN_POINT('Ctrl Pts',(-0.362276652824905,0.715494710669303,
-0.979797230245542));
#55896=CARTESIAN_POINT('Ctrl Pts',(-0.236705317813976,0.766255601412707,
-0.985080353677203));
#55897=CARTESIAN_POINT('Ctrl Pts',(-0.106635894154431,0.783948185627299,
-0.990363477108863));
#55898=CARTESIAN_POINT('Ctrl Pts',(0.0234335295051176,0.801640769841891,
-0.995646600540523));
#55899=CARTESIAN_POINT('Ctrl Pts',(0.158001041813281,0.786265047527667,
-1.00092972397218));
#55900=CARTESIAN_POINT('Ctrl Pts',(0.280726998019134,0.739687991151414,
-1.00621284740384));
#55901=CARTESIAN_POINT('Ctrl Pts',(0.403452954224987,0.693110934775161,
-1.0114959708355));
#55902=CARTESIAN_POINT('Ctrl Pts',(0.514337354328528,0.615332544336879,
-1.01677909426716));
#55903=CARTESIAN_POINT('Ctrl Pts',(0.599916237563637,0.515796936378977,
-1.02206221769882));
#55904=CARTESIAN_POINT('Ctrl Pts',(0.685495120798745,0.416261328421078,
-1.02734534113048));
#55905=CARTESIAN_POINT('Ctrl Pts',(0.74576848716542,0.294968502943563,-1.03262846456214));
#55906=CARTESIAN_POINT('Ctrl Pts',(0.773417739645104,0.166646247100582,
-1.0379115879938));
#55907=CARTESIAN_POINT('Ctrl Pts',(0.801066992124787,0.0383239912576011,
-1.04319471142546));
#55908=CARTESIAN_POINT('Ctrl Pts',(0.796092130717476,-0.0970276949508529,
-1.04847783485713));
#55909=CARTESIAN_POINT('Ctrl Pts',(0.759097220005225,-0.222973949713388,
-1.05376095828878));
#55910=CARTESIAN_POINT('Ctrl Pts',(0.722102309292974,-0.348920204475926,
-1.05904408172044));
#55911=CARTESIAN_POINT('Ctrl Pts',(0.653087349275782,-0.465461027792553,
-1.0643272051521));
#55912=CARTESIAN_POINT('Ctrl Pts',(0.560432370986682,-0.558445636763952,
-1.06961032858377));
#55913=CARTESIAN_POINT('Ctrl Pts',(0.467777392697587,-0.651430245735346,
-1.07489345201542));
#55914=CARTESIAN_POINT('Ctrl Pts',(0.351482396136587,-0.720858640361512,
-1.08017657544709));
#55915=CARTESIAN_POINT('Ctrl Pts',(0.225668315082744,-0.758300588973901,
-1.08545969887875));
#55916=CARTESIAN_POINT('Ctrl Pts',(0.0998542340288942,-0.795742537586291,
-1.09074282231041));
#55917=CARTESIAN_POINT('Ctrl Pts',(-0.0354789315177982,-0.801198040184898,
-1.09602594574207));
#55918=CARTESIAN_POINT('Ctrl Pts',(-0.163898568587665,-0.774004671100481,
-1.10130906917373));
#55919=CARTESIAN_POINT('Ctrl Pts',(-0.292318205657531,-0.746811302016064,
-1.10659219260539));
#55920=CARTESIAN_POINT('Ctrl Pts',(-0.41382431425057,-0.686969061248622,
-1.11187531603705));
#55921=CARTESIAN_POINT('Ctrl Pts',(-0.513663209651773,-0.601744197081025,
-1.11715843946871));
#55922=CARTESIAN_POINT('Ctrl Pts',(-0.613502105052971,-0.516519332913434,
-1.12244156290037));
#55923=CARTESIAN_POINT('Ctrl Pts',(-0.691673787262334,-0.405911845345692,
-1.12772468633203));
#55924=CARTESIAN_POINT('Ctrl Pts',(-0.738686384913777,-0.283352071482572,
-1.13300780976369));
#55925=CARTESIAN_POINT('Ctrl Pts',(-0.773269571419359,-0.193195225672542,
-1.13689415623456));
#55926=CARTESIAN_POINT('Ctrl Pts',(-0.790991646190477,-0.0965706405958467,
-1.14078050270543));
#55927=CARTESIAN_POINT('Ctrl Pts',(-0.791086342131762,2.01490389672293E-5,
-1.1446668491763));
#55928=CARTESIAN_POINT('Ctrl Pts',(-0.79107238223822,1.89686955811942E-5,
-1.1731331508237));
#55929=CARTESIAN_POINT('Ctrl Pts',(-0.790990086203271,-0.0917626946992069,
-1.1694404874619));
#55930=CARTESIAN_POINT('Ctrl Pts',(-0.775025954580806,-0.183572243071071,
-1.16574782410009));
#55931=CARTESIAN_POINT('Ctrl Pts',(-0.743735394388986,-0.269821481033168,
-1.16205516073828));
#55932=CARTESIAN_POINT('Ctrl Pts',(-0.698967736050869,-0.393218965556938,
-1.15677203730662));
#55933=CARTESIAN_POINT('Ctrl Pts',(-0.622828017098433,-0.505234907771603,
-1.15148891387496));
#55934=CARTESIAN_POINT('Ctrl Pts',(-0.524561381012293,-0.5922679512217,
-1.1462057904433));
#55935=CARTESIAN_POINT('Ctrl Pts',(-0.426294744926152,-0.679300994671797,
-1.14092266701163));
#55936=CARTESIAN_POINT('Ctrl Pts',(-0.305901191706306,-0.741351139357328,
-1.13563954357997));
#55937=CARTESIAN_POINT('Ctrl Pts',(-0.177999315812682,-0.770884045796831,
-1.13035642014831));
#55938=CARTESIAN_POINT('Ctrl Pts',(-0.0500974399190584,-0.800416952236334,
-1.12507329671665));
#55939=CARTESIAN_POINT('Ctrl Pts',(0.0853127586483453,-0.797432620429811,
-1.11979017328499));
#55940=CARTESIAN_POINT('Ctrl Pts',(0.21178931330864,-0.762293418089208,
-1.11450704985333));
#55941=CARTESIAN_POINT('Ctrl Pts',(0.338265867968928,-0.727154215748607,
-1.10922392642167));
#55942=CARTESIAN_POINT('Ctrl Pts',(0.455808778722111,-0.659860142873929,
-1.10394080299001));
#55943=CARTESIAN_POINT('Ctrl Pts',(0.55014558580614,-0.568582274531921,
-1.09865767955835));
#55944=CARTESIAN_POINT('Ctrl Pts',(0.644482392890175,-0.477304406189908,
-1.09337455612669));
#55945=CARTESIAN_POINT('Ctrl Pts',(0.715613096305057,-0.362042742380558,
-1.08809143269503));
#55946=CARTESIAN_POINT('Ctrl Pts',(0.754900764262811,-0.236792746107849,
-1.08280830926337));
#55947=CARTESIAN_POINT('Ctrl Pts',(0.794188432220566,-0.11154274983514,
-1.07752518583171));
#55948=CARTESIAN_POINT('Ctrl Pts',(0.801633064721195,0.0236955789009309,
-1.07224206240005));
#55949=CARTESIAN_POINT('Ctrl Pts',(0.776330709181529,0.152501142538597,
-1.06695893896839));
#55950=CARTESIAN_POINT('Ctrl Pts',(0.751028353641863,0.281306706176263,
-1.06167581553673));
#55951=CARTESIAN_POINT('Ctrl Pts',(0.692979010061908,0.403679504715515,
-1.05639269210507));
#55952=CARTESIAN_POINT('Ctrl Pts',(0.609231227053811,0.504760617002139,
-1.05110956867341));
#55953=CARTESIAN_POINT('Ctrl Pts',(0.525483444045717,0.605841729288761,
-1.04582644524175));
#55954=CARTESIAN_POINT('Ctrl Pts',(0.416037221609485,0.685631155322747,
-1.04054332181009));
#55955=CARTESIAN_POINT('Ctrl Pts',(0.294181892090384,0.734440591783975,
-1.03526019837843));
#55956=CARTESIAN_POINT('Ctrl Pts',(0.172326562571282,0.783250028245203,
-1.02997707494677));
#55957=CARTESIAN_POINT('Ctrl Pts',(0.0380621259693093,0.801079475133673,
-1.02469395151511));
#55958=CARTESIAN_POINT('Ctrl Pts',(-0.0923085734470331,0.785764020404375,
-1.01941082808345));
#55959=CARTESIAN_POINT('Ctrl Pts',(-0.222679272863376,0.770448565675077,
-1.01412770465179));
#55960=CARTESIAN_POINT('Ctrl Pts',(-0.349156235094089,0.72198820932801,
-1.00884458122013));
#55961=CARTESIAN_POINT('Ctrl Pts',(-0.456382197479121,0.646267172551726,
-1.00356145778847));
#55962=CARTESIAN_POINT('Ctrl Pts',(-0.563608159864155,0.570546135775441,
-0.998278334356811));
#55963=CARTESIAN_POINT('Ctrl Pts',(-0.651583122403507,0.467564418569935,
-0.992995210925151));
#55964=CARTESIAN_POINT('Ctrl Pts',(-0.709624866111236,0.349826411081959,
-0.987712087493491));
#55965=CARTESIAN_POINT('Ctrl Pts',(-0.763014173696973,0.241525896749369,
-0.982852441936896));
#55966=CARTESIAN_POINT('Ctrl Pts',(-0.791076636121826,0.12073991330517,
-0.9779927963803));
#55967=CARTESIAN_POINT('Ctrl Pts',(-0.791155923841092,-1.04795641788954E-5,
-0.973133150823705));
#55968=CARTESIAN_POINT('Origin',(0.,0.,-1.94));
#55969=CARTESIAN_POINT('',(-0.791032821705865,-2.40842565418786E-7,-0.744666849176295));
#55970=CARTESIAN_POINT('',(-0.791034434997536,-4.6591721334828E-6,-0.773133150823704));
#55971=CARTESIAN_POINT('',(-0.7911,-9.68818082805471E-17,-1.94));
#55972=CARTESIAN_POINT('Ctrl Pts',(-0.791032821705865,-2.40842565418786E-7,
-0.744666849176295));
#55973=CARTESIAN_POINT('Ctrl Pts',(-0.791032120695214,0.065925645056054,
-0.747318873678916));
#55974=CARTESIAN_POINT('Ctrl Pts',(-0.782881257592987,0.13185170122012,
-0.749970898181537));
#55975=CARTESIAN_POINT('Ctrl Pts',(-0.766582283740692,0.19569765947848,
-0.752622922684158));
#55976=CARTESIAN_POINT('Ctrl Pts',(-0.734112941701818,0.322885804896515,
-0.757906046115818));
#55977=CARTESIAN_POINT('Ctrl Pts',(-0.669307817269351,0.441819080529466,
-0.763189169547478));
#55978=CARTESIAN_POINT('Ctrl Pts',(-0.580035768930037,0.538056203785618,
-0.768472292979138));
#55979=CARTESIAN_POINT('Ctrl Pts',(-0.490763720590723,0.634293327041769,
-0.773755416410798));
#55980=CARTESIAN_POINT('Ctrl Pts',(-0.377024748344561,0.707834297921121,
-0.779038539842458));
#55981=CARTESIAN_POINT('Ctrl Pts',(-0.252629424810162,0.749749521767461,
-0.784321663274118));
#55982=CARTESIAN_POINT('Ctrl Pts',(-0.128234101275767,0.791664745613799,
-0.789604786705778));
#55983=CARTESIAN_POINT('Ctrl Pts',(0.00681757354686521,0.801954222427127,
-0.794887910137438));
#55984=CARTESIAN_POINT('Ctrl Pts',(0.136127166248591,0.77936856895796,-0.800171033569098));
#55985=CARTESIAN_POINT('Ctrl Pts',(0.265436758950324,0.756782915488791,
-0.805454157000758));
#55986=CARTESIAN_POINT('Ctrl Pts',(0.389004269531151,0.701322131737123,
-0.810737280432419));
#55987=CARTESIAN_POINT('Ctrl Pts',(0.491825710839823,0.619720454582025,
-0.816020403864079));
#55988=CARTESIAN_POINT('Ctrl Pts',(0.594647152148495,0.538118777426927,
-0.821303527295739));
#55989=CARTESIAN_POINT('Ctrl Pts',(0.676722524185013,0.4303762068684,-0.826586650727399));
#55990=CARTESIAN_POINT('Ctrl Pts',(0.728085956295501,0.30957521204986,-0.831869774159059));
#55991=CARTESIAN_POINT('Ctrl Pts',(0.779449388405989,0.18877421723132,-0.837152897590719));
#55992=CARTESIAN_POINT('Ctrl Pts',(0.800100880590446,0.0549147981527687,
-0.84243602102238));
#55993=CARTESIAN_POINT('Ctrl Pts',(0.787532858471651,-0.0757493795216767,
-0.84771914445404));
#55994=CARTESIAN_POINT('Ctrl Pts',(0.774964836352857,-0.206413557196118,
-0.8530022678857));
#55995=CARTESIAN_POINT('Ctrl Pts',(0.729177299930812,-0.333882493466454,
-0.85828539131736));
#55996=CARTESIAN_POINT('Ctrl Pts',(0.655729927513629,-0.442678476812936,
-0.86356851474902));
#55997=CARTESIAN_POINT('Ctrl Pts',(0.582282555096445,-0.551474460159418,
-0.86885163818068));
#55998=CARTESIAN_POINT('Ctrl Pts',(0.481175346684122,-0.641597490582047,
-0.87413476161234));
#55999=CARTESIAN_POINT('Ctrl Pts',(0.364685083194123,-0.702104523391029,
-0.879417885044));
#56000=CARTESIAN_POINT('Ctrl Pts',(0.248194819704125,-0.762611556200011,
-0.88470100847566));
#56001=CARTESIAN_POINT('Ctrl Pts',(0.11632150113645,-0.793502591395346,
-0.88998413190732));
#56002=CARTESIAN_POINT('Ctrl Pts',(-0.0149223659197404,-0.791026734482348,
-0.89526725533898));
#56003=CARTESIAN_POINT('Ctrl Pts',(-0.146166232975938,-0.78855087756935,
-0.90055037877064));
#56004=CARTESIAN_POINT('Ctrl Pts',(-0.276780648520651,-0.752708128548016,
-0.905833502202301));
#56005=CARTESIAN_POINT('Ctrl Pts',(-0.390905966248882,-0.687850635837082,
-0.911116625633962));
#56006=CARTESIAN_POINT('Ctrl Pts',(-0.505031283977106,-0.622993143126152,
-0.916399749065622));
#56007=CARTESIAN_POINT('Ctrl Pts',(-0.602667503888851,-0.529120906725625,
-0.921682872497282));
#56008=CARTESIAN_POINT('Ctrl Pts',(-0.671959304288581,-0.417632212659005,
-0.926965995928942));
#56009=CARTESIAN_POINT('Ctrl Pts',(-0.74125110468831,-0.306143518592384,
-0.932249119360602));
#56010=CARTESIAN_POINT('Ctrl Pts',(-0.782198485576025,-0.177038366859669,
-0.937532242792262));
#56011=CARTESIAN_POINT('Ctrl Pts',(-0.789829476780693,-0.0459931438236847,
-0.942815366223922));
#56012=CARTESIAN_POINT('Ctrl Pts',(-0.790720909680688,-0.0306847756093432,
-0.943432527208046));
#56013=CARTESIAN_POINT('Ctrl Pts',(-0.791157696612461,-0.0153499325697136,
-0.94404968819217));
#56014=CARTESIAN_POINT('Ctrl Pts',(-0.791144809354952,-1.43559245109892E-5,
-0.944666849176295));
#56015=CARTESIAN_POINT('Ctrl Pts',(-0.791155923841092,-1.04795641788954E-5,
-0.973133150823705));
#56016=CARTESIAN_POINT('Ctrl Pts',(-0.791162833109368,-0.0105328765558965,
-0.97270967294864));
#56017=CARTESIAN_POINT('Ctrl Pts',(-0.790957247118644,-0.0210550032841967,
-0.972286195073575));
#56018=CARTESIAN_POINT('Ctrl Pts',(-0.790537408105818,-0.031568574234663,
-0.971862717198511));
#56019=CARTESIAN_POINT('Ctrl Pts',(-0.785299681516566,-0.162731254292855,
-0.96657959376685));
#56020=CARTESIAN_POINT('Ctrl Pts',(-0.746715703461958,-0.292562316638795,
-0.96129647033519));
#56021=CARTESIAN_POINT('Ctrl Pts',(-0.679470471707622,-0.405297232375568,
-0.95601334690353));
#56022=CARTESIAN_POINT('Ctrl Pts',(-0.612225239953286,-0.518032148112341,
-0.95073022347187));
#56023=CARTESIAN_POINT('Ctrl Pts',(-0.516318754499222,-0.613670917239946,
-0.94544710004021));
#56024=CARTESIAN_POINT('Ctrl Pts',(-0.4033963068036,-0.680600755326564,
-0.94016397660855));
#56025=CARTESIAN_POINT('Ctrl Pts',(-0.290473859107974,-0.747530593413184,
-0.93488085317689));
#56026=CARTESIAN_POINT('Ctrl Pts',(-0.160535449170788,-0.785751500458815,
-0.92959772974523));
#56027=CARTESIAN_POINT('Ctrl Pts',(-0.0293586403983704,-0.790622564013849,
-0.924314606313569));
#56028=CARTESIAN_POINT('Ctrl Pts',(0.101818168374047,-0.795493627568883,
-0.919031482881909));
#56029=CARTESIAN_POINT('Ctrl Pts',(0.234233375981696,-0.767014847633319,
-0.913748359450248));
#56030=CARTESIAN_POINT('Ctrl Pts',(0.351808677826252,-0.70864421446874,
-0.908465236018588));
#56031=CARTESIAN_POINT('Ctrl Pts',(0.469383979670803,-0.650273581304164,
-0.903182112586928));
#56032=CARTESIAN_POINT('Ctrl Pts',(0.572119375752263,-0.562011094910577,
-0.897898989155269));
#56033=CARTESIAN_POINT('Ctrl Pts',(0.647540385072036,-0.454573886397616,
-0.892615865723609));
#56034=CARTESIAN_POINT('Ctrl Pts',(0.722961394391813,-0.34713667788465,
-0.887332742291949));
#56035=CARTESIAN_POINT('Ctrl Pts',(0.7710680169499,-0.220524747252309,-0.882049618860289));
#56036=CARTESIAN_POINT('Ctrl Pts',(0.786018983116774,-0.0901117454827402,
-0.876766495428628));
#56037=CARTESIAN_POINT('Ctrl Pts',(0.800969949283647,0.040301256286821,
-0.871483371996968));
#56038=CARTESIAN_POINT('Ctrl Pts',(0.782765259059311,0.17451532919361,-0.866200248565308));
#56039=CARTESIAN_POINT('Ctrl Pts',(0.733615387810102,0.296233744300185,
-0.860917125133648));
#56040=CARTESIAN_POINT('Ctrl Pts',(0.68446551656089,0.417952159406768,-0.855634001701988));
#56041=CARTESIAN_POINT('Ctrl Pts',(0.604370464286801,0.527174916713137,
-0.850350878270329));
#56042=CARTESIAN_POINT('Ctrl Pts',(0.50305564448488,0.61063981776967,-0.845067754838668));
#56043=CARTESIAN_POINT('Ctrl Pts',(0.401740824682959,0.694104718826203,
-0.839784631407008));
#56044=CARTESIAN_POINT('Ctrl Pts',(0.279206237353206,0.7518117636329,-0.834501507975347));
#56045=CARTESIAN_POINT('Ctrl Pts',(0.15033044859473,0.776753966658157,-0.829218384543687));
#56046=CARTESIAN_POINT('Ctrl Pts',(0.0214546598362535,0.801696169683414,
-0.823935261112027));
#56047=CARTESIAN_POINT('Ctrl Pts',(-0.113762330350946,0.79387353092723,
-0.818652137680367));
#56048=CARTESIAN_POINT('Ctrl Pts',(-0.238902015404239,0.7542359017772,-0.813369014248707));
#56049=CARTESIAN_POINT('Ctrl Pts',(-0.364041700457527,0.714598272627171,
-0.808085890817047));
#56050=CARTESIAN_POINT('Ctrl Pts',(-0.479104080376909,0.643145653083297,
-0.802802767385386));
#56051=CARTESIAN_POINT('Ctrl Pts',(-0.570117889885716,0.548554063084152,
-0.797519643953726));
#56052=CARTESIAN_POINT('Ctrl Pts',(-0.661131699394522,0.453962473085008,
-0.792236520522066));
#56053=CARTESIAN_POINT('Ctrl Pts',(-0.728096938492752,0.336231912630593,
-0.786953397090406));
#56054=CARTESIAN_POINT('Ctrl Pts',(-0.762882460228531,0.209657626547513,
-0.781670273658746));
#56055=CARTESIAN_POINT('Ctrl Pts',(-0.7816193732044,0.141479509187784,-0.778824566047066));
#56056=CARTESIAN_POINT('Ctrl Pts',(-0.791019847233727,0.0707355239100122,
-0.775978858435385));
#56057=CARTESIAN_POINT('Ctrl Pts',(-0.791034434997536,-4.65917213348279E-6,
-0.773133150823704));
#56058=CARTESIAN_POINT('Origin',(0.,0.,-1.94));
#56059=CARTESIAN_POINT('',(-0.791143457346284,1.47250900771681E-5,-0.544666849176294));
#56060=CARTESIAN_POINT('',(-0.791129915139071,1.76226913310852E-5,-0.573133150823703));
#56061=CARTESIAN_POINT('',(-0.7911,-9.68818082805471E-17,-1.94));
#56062=CARTESIAN_POINT('Ctrl Pts',(-0.791143457346284,1.47250900771681E-5,
-0.544666849176294));
#56063=CARTESIAN_POINT('Ctrl Pts',(-0.791157032798385,0.0158703510580344,
-0.545304935734));
#56064=CARTESIAN_POINT('Ctrl Pts',(-0.790690104471727,0.0317251781600011,
-0.545943022291706));
#56065=CARTESIAN_POINT('Ctrl Pts',(-0.789737233642478,0.0475507462532112,
-0.546581108849412));
#56066=CARTESIAN_POINT('Ctrl Pts',(-0.781847811518544,0.178580664691211,
-0.551864232281072));
#56067=CARTESIAN_POINT('Ctrl Pts',(-0.740645890688464,0.307604809429334,
-0.557147355712733));
#56068=CARTESIAN_POINT('Ctrl Pts',(-0.671134348428437,0.418956630249429,
-0.562430479144392));
#56069=CARTESIAN_POINT('Ctrl Pts',(-0.601622806168408,0.530308451069527,
-0.567713602576053));
#56070=CARTESIAN_POINT('Ctrl Pts',(-0.50380164247843,0.623987947971596,
-0.572996726007712));
#56071=CARTESIAN_POINT('Ctrl Pts',(-0.38954863555615,0.688620238017154,
-0.578279849439373));
#56072=CARTESIAN_POINT('Ctrl Pts',(-0.27529562863387,0.753252528062712,
-0.583562972871033));
#56073=CARTESIAN_POINT('Ctrl Pts',(-0.144610778479288,0.78883761125176,
-0.588846096302693));
#56074=CARTESIAN_POINT('Ctrl Pts',(-0.0133622838071854,0.791054625826753,
-0.594129219734354));
#56075=CARTESIAN_POINT('Ctrl Pts',(0.117886210864914,0.793271640401747,
-0.599412343166014));
#56076=CARTESIAN_POINT('Ctrl Pts',(0.249698350054534,0.762120586362689,
-0.604695466597674));
#56077=CARTESIAN_POINT('Ctrl Pts',(0.366069055780573,0.701383930576091,
-0.609978590029334));
#56078=CARTESIAN_POINT('Ctrl Pts',(0.482439761506612,0.640647274789494,
-0.615261713460994));
#56079=CARTESIAN_POINT('Ctrl Pts',(0.583369033769069,0.550325017255357,
-0.620544836892654));
#56080=CARTESIAN_POINT('Ctrl Pts',(0.656601697262608,0.441384393496546,
-0.625827960324314));
#56081=CARTESIAN_POINT('Ctrl Pts',(0.729834360756149,0.332443769737732,
-0.631111083755974));
#56082=CARTESIAN_POINT('Ctrl Pts',(0.775370415480771,0.204884779754242,
-0.636394207187635));
#56083=CARTESIAN_POINT('Ctrl Pts',(0.787680718890875,0.0741960696937758,
-0.641677330619295));
#56084=CARTESIAN_POINT('Ctrl Pts',(0.799991022300978,-0.0564926403666832,
-0.646960454050955));
#56085=CARTESIAN_POINT('Ctrl Pts',(0.779075574396567,-0.190311070504119,
-0.652243577482614));
#56086=CARTESIAN_POINT('Ctrl Pts',(0.727473999955588,-0.311010532070969,
-0.657526700914274));
#56087=CARTESIAN_POINT('Ctrl Pts',(0.675872425514605,-0.431709993637826,
-0.662809824345935));
#56088=CARTESIAN_POINT('Ctrl Pts',(0.59358472453705,-0.539290486634097,
-0.668092947777595));
#56089=CARTESIAN_POINT('Ctrl Pts',(0.490602549378544,-0.620689221924888,
-0.673376071209255));
#56090=CARTESIAN_POINT('Ctrl Pts',(0.387620374220037,-0.702087957215679,
-0.678659194640915));
#56091=CARTESIAN_POINT('Ctrl Pts',(0.263943724880579,-0.75730493480099,
-0.683942318072575));
#56092=CARTESIAN_POINT('Ctrl Pts',(0.134589840510463,-0.779635521575189,
-0.689225441504236));
#56093=CARTESIAN_POINT('Ctrl Pts',(0.00523595614035394,-0.801966108349387,
-0.694508564935896));
#56094=CARTESIAN_POINT('Ctrl Pts',(-0.129795163260413,-0.791410304312477,
-0.699791688367556));
#56095=CARTESIAN_POINT('Ctrl Pts',(-0.254107580191888,-0.7492498310707,
-0.705074811799216));
#56096=CARTESIAN_POINT('Ctrl Pts',(-0.378419997123371,-0.70708935782892,
-0.710357935230876));
#56097=CARTESIAN_POINT('Ctrl Pts',(-0.49201371158556,-0.63332421538227,
-0.715641058662536));
#56098=CARTESIAN_POINT('Ctrl Pts',(-0.581095788653718,-0.536911218060642,
-0.720924182094196));
#56099=CARTESIAN_POINT('Ctrl Pts',(-0.670177865721877,-0.440498220739014,
-0.726207305525856));
#56100=CARTESIAN_POINT('Ctrl Pts',(-0.734748305396003,-0.321437368542408,
-0.731490428957517));
#56101=CARTESIAN_POINT('Ctrl Pts',(-0.766966745410426,-0.194185434842544,
-0.736773552389177));
#56102=CARTESIAN_POINT('Ctrl Pts',(-0.783012159475383,-0.130811479869343,
-0.739404651318217));
#56103=CARTESIAN_POINT('Ctrl Pts',(-0.791033517185251,-0.0654059441505127,
-0.742035750247256));
#56104=CARTESIAN_POINT('Ctrl Pts',(-0.791032821705865,-2.40842565418786E-7,
-0.744666849176295));
#56105=CARTESIAN_POINT('Ctrl Pts',(-0.791034434997536,-4.65917213348279E-6,
-0.773133150823704));
#56106=CARTESIAN_POINT('Ctrl Pts',(-0.791046929761981,-0.0605952977342058,
-0.770695735003725));
#56107=CARTESIAN_POINT('Ctrl Pts',(-0.784173631136982,-0.12118314688111,
-0.768258319183745));
#56108=CARTESIAN_POINT('Ctrl Pts',(-0.770383467724153,-0.180153493308298,
-0.765820903363765));
#56109=CARTESIAN_POINT('Ctrl Pts',(-0.740493149110667,-0.307972315369276,
-0.760537779932105));
#56110=CARTESIAN_POINT('Ctrl Pts',(-0.678106707510369,-0.428191947779487,
-0.755254656500445));
#56111=CARTESIAN_POINT('Ctrl Pts',(-0.590799316719212,-0.526214914134886,
-0.749971533068785));
#56112=CARTESIAN_POINT('Ctrl Pts',(-0.503491925928054,-0.624237880490285,
-0.744688409637125));
#56113=CARTESIAN_POINT('Ctrl Pts',(-0.391263585946037,-0.700064180790871,
-0.739405286205465));
#56114=CARTESIAN_POINT('Ctrl Pts',(-0.26774144328749,-0.744486727914074,
-0.734122162773805));
#56115=CARTESIAN_POINT('Ctrl Pts',(-0.144219300628944,-0.788909275037278,
-0.728839039342145));
#56116=CARTESIAN_POINT('Ctrl Pts',(-0.00940335529385652,-0.8019280689831,
-0.723555915910484));
#56117=CARTESIAN_POINT('Ctrl Pts',(0.120336582384249,-0.781962323538643,
-0.718272792478824));
#56118=CARTESIAN_POINT('Ctrl Pts',(0.250076520062358,-0.761996578094185,
-0.712989669047164));
#56119=CARTESIAN_POINT('Ctrl Pts',(0.374740450083486,-0.709046293259455,
-0.707706545615504));
#56120=CARTESIAN_POINT('Ctrl Pts',(0.479191254321141,-0.629540872601617,
-0.702423422183844));
#56121=CARTESIAN_POINT('Ctrl Pts',(0.583642058558793,-0.550035451943781,
-0.697140298752184));
#56122=CARTESIAN_POINT('Ctrl Pts',(0.667879737012961,-0.443974895462845,
-0.691857175320524));
#56123=CARTESIAN_POINT('Ctrl Pts',(0.721675864434676,-0.324237436435612,
-0.686574051888864));
#56124=CARTESIAN_POINT('Ctrl Pts',(0.775471991856391,-0.204499977408379,
-0.681290928457204));
#56125=CARTESIAN_POINT('Ctrl Pts',(0.798826568245652,-0.0710856158348409,
-0.676007805025542));
#56126=CARTESIAN_POINT('Ctrl Pts',(0.788903801553075,0.0598060230159138,
-0.670724681593883));
#56127=CARTESIAN_POINT('Ctrl Pts',(0.778981034860496,0.190697661866672,
-0.665441558162223));
#56128=CARTESIAN_POINT('Ctrl Pts',(0.73578092508608,0.319066577994655,-0.660158434730563));
#56129=CARTESIAN_POINT('Ctrl Pts',(0.664548976399496,0.429325781266692,
-0.654875311298903));
#56130=CARTESIAN_POINT('Ctrl Pts',(0.593317027712914,0.539584984538727,
-0.649592187867243));
#56131=CARTESIAN_POINT('Ctrl Pts',(0.494053240114169,0.631734474954815,
-0.644309064435582));
#56132=CARTESIAN_POINT('Ctrl Pts',(0.378810560099591,0.694585148164649,
-0.639025941003921));
#56133=CARTESIAN_POINT('Ctrl Pts',(0.263567880085013,0.757435821374483,
-0.633742817572261));
#56134=CARTESIAN_POINT('Ctrl Pts',(0.132346307654605,0.79098767737806,-0.628459694140602));
#56135=CARTESIAN_POINT('Ctrl Pts',(0.00107921216619798,0.791166735773803,
-0.623176570708942));
#56136=CARTESIAN_POINT('Ctrl Pts',(-0.130187883322209,0.791345794169545,
-0.617893447277282));
#56137=CARTESIAN_POINT('Ctrl Pts',(-0.261500501868612,0.758152054957453,
-0.612610323845622));
#56138=CARTESIAN_POINT('Ctrl Pts',(-0.376914218986303,0.695616014781013,
-0.607327200413961));
#56139=CARTESIAN_POINT('Ctrl Pts',(-0.492327936103994,0.633079974604573,
-0.602044076982301));
#56140=CARTESIAN_POINT('Ctrl Pts',(-0.591842751792971,0.541201633463786,
-0.596760953550642));
#56141=CARTESIAN_POINT('Ctrl Pts',(-0.663375238872918,0.431137171842295,
-0.591477830118981));
#56142=CARTESIAN_POINT('Ctrl Pts',(-0.73490772595287,0.321072710220798,
-0.586194706687321));
#56143=CARTESIAN_POINT('Ctrl Pts',(-0.778457884423789,0.192822128118595,
-0.580911583255661));
#56144=CARTESIAN_POINT('Ctrl Pts',(-0.78873770601343,0.0619580471492215,
-0.575628459824));
#56145=CARTESIAN_POINT('Ctrl Pts',(-0.790356150838471,0.0413549371845394,
-0.574796690157235));
#56146=CARTESIAN_POINT('Ctrl Pts',(-0.791149922541304,0.0206870463227368,
-0.573964920490469));
#56147=CARTESIAN_POINT('Ctrl Pts',(-0.791129915139071,1.76226913310852E-5,
-0.573133150823703));
#56148=CARTESIAN_POINT('Origin',(0.,0.,-1.94));
#56149=CARTESIAN_POINT('',(-0.791087916566115,-2.02165423325296E-5,-0.344666849176295));
#56150=CARTESIAN_POINT('',(-0.791102868091814,-2.02590743034978E-5,-0.373133150823704));
#56151=CARTESIAN_POINT('',(-0.7911,-9.68818082805471E-17,-1.94));
#56152=CARTESIAN_POINT('Ctrl Pts',(-0.791087916566115,-2.02165423325296E-5,
-0.344666849176295));
#56153=CARTESIAN_POINT('Ctrl Pts',(-0.790992060355861,0.097090099215087,
-0.348574121220746));
#56154=CARTESIAN_POINT('Ctrl Pts',(-0.773074216505353,0.194234811893738,
-0.352481393265196));
#56155=CARTESIAN_POINT('Ctrl Pts',(-0.738126125034402,0.284808348566891,
-0.356388665309647));
#56156=CARTESIAN_POINT('Ctrl Pts',(-0.690871908066276,0.407275166449671,
-0.361671788741307));
#56157=CARTESIAN_POINT('Ctrl Pts',(-0.612482238925616,0.517728269629272,
-0.366954912172967));
#56158=CARTESIAN_POINT('Ctrl Pts',(-0.512475458209948,0.602756067010894,
-0.372238035604627));
#56159=CARTESIAN_POINT('Ctrl Pts',(-0.412468677494272,0.687783864392524,
-0.377521159036288));
#56160=CARTESIAN_POINT('Ctrl Pts',(-0.290844785203582,0.747386355976171,
-0.382804282467948));
#56161=CARTESIAN_POINT('Ctrl Pts',(-0.162371767485705,0.774326404571983,
-0.388087405899608));
#56162=CARTESIAN_POINT('Ctrl Pts',(-0.0338987497678321,0.801266453167794,
-0.393370529331269));
#56163=CARTESIAN_POINT('Ctrl Pts',(0.101423393377231,0.795544058775773,
-0.398653652762929));
#56164=CARTESIAN_POINT('Ctrl Pts',(0.227163387222433,0.757854054008525,
-0.403936776194589));
#56165=CARTESIAN_POINT('Ctrl Pts',(0.352903381067629,0.72016404924128,-0.409219899626249));
#56166=CARTESIAN_POINT('Ctrl Pts',(0.469061225612968,0.65050643409881,-0.414503023057909));
#56167=CARTESIAN_POINT('Ctrl Pts',(0.561532640612168,0.557339272966225,
-0.419786146489568));
#56168=CARTESIAN_POINT('Ctrl Pts',(0.654004055611374,0.464172111833635,
-0.425069269921229));
#56169=CARTESIAN_POINT('Ctrl Pts',(0.72278904106444,0.347495404710924,-0.430352393352889));
#56170=CARTESIAN_POINT('Ctrl Pts',(0.75953549019646,0.221476433980054,-0.435635516784549));
#56171=CARTESIAN_POINT('Ctrl Pts',(0.796281939328478,0.0954574632491873,
-0.44091864021621));
#56172=CARTESIAN_POINT('Ctrl Pts',(0.800989852139453,-0.0399037710898398,
-0.44620176364787));
#56173=CARTESIAN_POINT('Ctrl Pts',(0.773087577871225,-0.168171247863792,
-0.45148488707953));
#56174=CARTESIAN_POINT('Ctrl Pts',(0.745185303602996,-0.296438724637747,
-0.45676801051119));
#56175=CARTESIAN_POINT('Ctrl Pts',(0.684672842255569,-0.417612443846618,
-0.46205113394285));
#56176=CARTESIAN_POINT('Ctrl Pts',(0.5988978225636,-0.516979080621905,-0.46733425737451));
#56177=CARTESIAN_POINT('Ctrl Pts',(0.513122802871631,-0.616345717397192,
-0.47261738080617));
#56178=CARTESIAN_POINT('Ctrl Pts',(0.402085224835124,-0.693905271738887,
-0.47790050423783));
#56179=CARTESIAN_POINT('Ctrl Pts',(0.279267648610165,-0.74024019892847,
-0.483183627669491));
#56180=CARTESIAN_POINT('Ctrl Pts',(0.156450072385206,-0.786575126118053,
-0.488466751101151));
#56181=CARTESIAN_POINT('Ctrl Pts',(0.0218524979717924,-0.801685426155526,
-0.493749874532811));
#56182=CARTESIAN_POINT('Ctrl Pts',(-0.108181779638531,-0.783736355048523,
-0.499032997964471));
#56183=CARTESIAN_POINT('Ctrl Pts',(-0.238216057248851,-0.765787283941521,
-0.504316121396131));
#56184=CARTESIAN_POINT('Ctrl Pts',(-0.363687038056083,-0.714778841690045,
-0.509599244827791));
#56185=CARTESIAN_POINT('Ctrl Pts',(-0.469359609082811,-0.636904646734636,
-0.514882368259451));
#56186=CARTESIAN_POINT('Ctrl Pts',(-0.57503218010954,-0.559030451779227,
-0.520165491691111));
#56187=CARTESIAN_POINT('Ctrl Pts',(-0.660906341355765,-0.454290504119883,
-0.525448615122772));
#56188=CARTESIAN_POINT('Ctrl Pts',(-0.716554960269984,-0.335402684221274,
-0.530731738554432));
#56189=CARTESIAN_POINT('Ctrl Pts',(-0.765482434743157,-0.230873930646506,
-0.535376775428386));
#56190=CARTESIAN_POINT('Ctrl Pts',(-0.791044633017785,-0.115408435594574,
-0.54002181230234));
#56191=CARTESIAN_POINT('Ctrl Pts',(-0.791143457346284,1.47250900771681E-5,
-0.544666849176294));
#56192=CARTESIAN_POINT('Ctrl Pts',(-0.791129915139071,1.76226913310852E-5,
-0.573133150823703));
#56193=CARTESIAN_POINT('Ctrl Pts',(-0.791022842197109,-0.110598236934363,
-0.568681797058809));
#56194=CARTESIAN_POINT('Ctrl Pts',(-0.767608864627571,-0.221257995592029,
-0.564230443293914));
#56195=CARTESIAN_POINT('Ctrl Pts',(-0.722557746651952,-0.322267390914949,
-0.55977908952902));
#56196=CARTESIAN_POINT('Ctrl Pts',(-0.669088480992473,-0.442151168173203,
-0.55449596609736));
#56197=CARTESIAN_POINT('Ctrl Pts',(-0.585140464965152,-0.548441142853183,
-0.5492128426657));
#56198=CARTESIAN_POINT('Ctrl Pts',(-0.480906952022514,-0.628231224940537,
-0.54392971923404));
#56199=CARTESIAN_POINT('Ctrl Pts',(-0.37667343907987,-0.708021307027895,
-0.538646595802379));
#56200=CARTESIAN_POINT('Ctrl Pts',(-0.252154429221904,-0.761311496522626,
-0.533363472370719));
#56201=CARTESIAN_POINT('Ctrl Pts',(-0.122469443876305,-0.781631117478379,
-0.528080348939059));
#56202=CARTESIAN_POINT('Ctrl Pts',(0.00721554146929006,-0.801950738434132,
-0.522797225507399));
#56203=CARTESIAN_POINT('Ctrl Pts',(0.142066502302521,-0.789299790850911,
-0.517514102075739));
#56204=CARTESIAN_POINT('Ctrl Pts',(0.265709376589039,-0.745214395785903,
-0.512230978644079));
#56205=CARTESIAN_POINT('Ctrl Pts',(0.389352250875561,-0.701129000720895,
-0.506947855212419));
#56206=CARTESIAN_POINT('Ctrl Pts',(0.501787038615372,-0.625609158174098,
-0.501664731780758));
#56207=CARTESIAN_POINT('Ctrl Pts',(0.589361525705732,-0.527824744125977,
-0.496381608349098));
#56208=CARTESIAN_POINT('Ctrl Pts',(0.676936012796088,-0.430040330077863,
-0.491098484917439));
#56209=CARTESIAN_POINT('Ctrl Pts',(0.739650199236998,-0.309991344528425,
-0.485815361485779));
#56210=CARTESIAN_POINT('Ctrl Pts',(0.769889115339775,-0.182254543359766,
-0.480532238054119));
#56211=CARTESIAN_POINT('Ctrl Pts',(0.800128031442554,-0.0545177421910954,
-0.475249114622459));
#56212=CARTESIAN_POINT('Ctrl Pts',(0.797891677207195,0.0809068745967896,
-0.469965991190798));
#56213=CARTESIAN_POINT('Ctrl Pts',(0.763451598366819,0.207575589713544,
-0.464682867759138));
#56214=CARTESIAN_POINT('Ctrl Pts',(0.729011519526445,0.334244304830287,
-0.459399744327478));
#56215=CARTESIAN_POINT('Ctrl Pts',(0.662367716081058,0.452157118275893,
-0.454116620895818));
#56216=CARTESIAN_POINT('Ctrl Pts',(0.571612305172384,0.546996655446337,
-0.448833497464158));
#56217=CARTESIAN_POINT('Ctrl Pts',(0.480856894263705,0.641836192616787,
-0.443550374032498));
#56218=CARTESIAN_POINT('Ctrl Pts',(0.365989875891734,0.713602453512075,
-0.438267250600838));
#56219=CARTESIAN_POINT('Ctrl Pts',(0.240958793871168,0.753581334794116,
-0.432984127169178));
#56220=CARTESIAN_POINT('Ctrl Pts',(0.115927711850602,0.793560216076158,
-0.427701003737517));
#56221=CARTESIAN_POINT('Ctrl Pts',(-0.0192674338185621,0.801751717744953,
-0.422417880305857));
#56222=CARTESIAN_POINT('Ctrl Pts',(-0.148210789011595,0.777161199825293,
-0.417134756874197));
#56223=CARTESIAN_POINT('Ctrl Pts',(-0.277154144204628,0.752570681905633,
-0.411851633442537));
#56224=CARTESIAN_POINT('Ctrl Pts',(-0.399845708921533,0.695198144397515,
-0.406568510010877));
#56225=CARTESIAN_POINT('Ctrl Pts',(-0.501387856330821,0.612009955817321,
-0.401285386579216));
#56226=CARTESIAN_POINT('Ctrl Pts',(-0.602930003740106,0.528821767237129,
-0.396002263147556));
#56227=CARTESIAN_POINT('Ctrl Pts',(-0.683322733841777,0.419817927584861,
-0.390719139715896));
#56228=CARTESIAN_POINT('Ctrl Pts',(-0.732804488093843,0.298234053588397,
-0.385436016284236));
#56229=CARTESIAN_POINT('Ctrl Pts',(-0.771214049734729,0.203856168782306,
-0.381335061130725));
#56230=CARTESIAN_POINT('Ctrl Pts',(-0.790998398675608,0.101898263967332,
-0.377234105977215));
#56231=CARTESIAN_POINT('Ctrl Pts',(-0.791102868091814,-2.02590743034978E-5,
-0.373133150823704));
#56232=CARTESIAN_POINT('Origin',(0.,0.,-1.94));
#56233=CARTESIAN_POINT('',(-0.791054317571617,1.54395522024842E-5,-0.144666849176294));
#56234=CARTESIAN_POINT('',(-0.791044518748003,1.1964098827608E-5,-0.173133150823703));
#56235=CARTESIAN_POINT('',(-0.7911,-9.68818082805471E-17,-1.94));
#56236=CARTESIAN_POINT('Ctrl Pts',(-0.791054317571617,1.54395522024842E-5,
-0.144666849176294));
#56237=CARTESIAN_POINT('Ctrl Pts',(-0.79108665330085,0.0470775663249256,
-0.14656018327583));
#56238=CARTESIAN_POINT('Ctrl Pts',(-0.786954227878093,0.0941339831305366,
-0.148453517375366));
#56239=CARTESIAN_POINT('Ctrl Pts',(-0.778604014212082,0.140429697846895,
-0.150346851474902));
#56240=CARTESIAN_POINT('Ctrl Pts',(-0.755303736945075,0.269612378950766,
-0.155629974906562));
#56241=CARTESIAN_POINT('Ctrl Pts',(-0.699162807492777,0.392872061722574,
-0.160913098338222));
#56242=CARTESIAN_POINT('Ctrl Pts',(-0.616994819475088,0.495241307414285,
-0.166196221769883));
#56243=CARTESIAN_POINT('Ctrl Pts',(-0.5348268314574,0.597610553105996,-0.171479345201543));
#56244=CARTESIAN_POINT('Ctrl Pts',(-0.426631784874323,0.679089361717608,
-0.176762468633203));
#56245=CARTESIAN_POINT('Ctrl Pts',(-0.305548738351313,0.729784722528592,
-0.182045592064863));
#56246=CARTESIAN_POINT('Ctrl Pts',(-0.184465691828305,0.780480083339574,
-0.187328715496523));
#56247=CARTESIAN_POINT('Ctrl Pts',(-0.0504946453653669,0.800391996349929,
-0.192611838928183));
#56248=CARTESIAN_POINT('Ctrl Pts',(0.0800980227545852,0.787102473350495,
-0.197894962359843));
#56249=CARTESIAN_POINT('Ctrl Pts',(0.210690690874534,0.77381295035106,-0.203178085791503));
#56250=CARTESIAN_POINT('Ctrl Pts',(0.337904980651504,0.727321991341834,
-0.208461209223164));
#56251=CARTESIAN_POINT('Ctrl Pts',(0.446293670933016,0.653274796900439,
-0.213744332654824));
#56252=CARTESIAN_POINT('Ctrl Pts',(0.554682361214537,0.579227602459038,
-0.219027456086484));
#56253=CARTESIAN_POINT('Ctrl Pts',(0.644245452000599,0.477624172585471,
-0.224310579518144));
#56254=CARTESIAN_POINT('Ctrl Pts',(0.704108107756478,0.360801484773388,
-0.229593702949804));
#56255=CARTESIAN_POINT('Ctrl Pts',(0.763970763512355,0.243978796961309,
-0.234876826381464));
#56256=CARTESIAN_POINT('Ctrl Pts',(0.794132984238041,0.111936851210725,
-0.240159949813125));
#56257=CARTESIAN_POINT('Ctrl Pts',(0.790932258558706,-0.0192913418477741,
-0.245443073244785));
#56258=CARTESIAN_POINT('Ctrl Pts',(0.787731532879371,-0.150519534906269,
-0.250726196676446));
#56259=CARTESIAN_POINT('Ctrl Pts',(0.751167860795012,-0.280933975272688,
-0.256009320108106));
#56260=CARTESIAN_POINT('Ctrl Pts',(0.685680984842779,-0.394699312989822,
-0.261292443539766));
#56261=CARTESIAN_POINT('Ctrl Pts',(0.620194108890548,-0.508464650706953,
-0.266575566971426));
#56262=CARTESIAN_POINT('Ctrl Pts',(0.525784029070445,-0.60558088577481,
-0.271858690403086));
#56263=CARTESIAN_POINT('Ctrl Pts',(0.413914308982594,-0.674255827328862,
-0.277141813834746));
#56264=CARTESIAN_POINT('Ctrl Pts',(0.30204458889474,-0.742930768882917,
-0.282424937266406));
#56265=CARTESIAN_POINT('Ctrl Pts',(0.172715228539141,-0.783164416923164,
-0.287708060698066));
#56266=CARTESIAN_POINT('Ctrl Pts',(0.0416298533602581,-0.790071468974327,
-0.292991184129726));
#56267=CARTESIAN_POINT('Ctrl Pts',(-0.0894555218186243,-0.79697852102549,
-0.298274307561386));
#56268=CARTESIAN_POINT('Ctrl Pts',(-0.222296911820787,-0.770558977087567,
-0.303557430993046));
#56269=CARTESIAN_POINT('Ctrl Pts',(-0.34076427114486,-0.71402078603363,
-0.308840554424706));
#56270=CARTESIAN_POINT('Ctrl Pts',(-0.459231630468936,-0.65748259497969,
-0.314123677856367));
#56271=CARTESIAN_POINT('Ctrl Pts',(-0.563324959114919,-0.570825756809734,
-0.319406801288026));
#56272=CARTESIAN_POINT('Ctrl Pts',(-0.640404887410046,-0.464572440366096,
-0.324689924719687));
#56273=CARTESIAN_POINT('Ctrl Pts',(-0.717484815705173,-0.358319123922458,
-0.329973048151347));
#56274=CARTESIAN_POINT('Ctrl Pts',(-0.767551343649444,-0.232469329205139,
-0.335256171583008));
#56275=CARTESIAN_POINT('Ctrl Pts',(-0.784525225223783,-0.102304165553495,
-0.340539295014668));
#56276=CARTESIAN_POINT('Ctrl Pts',(-0.788945628951326,-0.068406051437288,
-0.341915146401877));
#56277=CARTESIAN_POINT('Ctrl Pts',(-0.791121670013111,-0.0342152664715848,
-0.343290997789086));
#56278=CARTESIAN_POINT('Ctrl Pts',(-0.791087916566115,-2.02165423325296E-5,
-0.344666849176295));
#56279=CARTESIAN_POINT('Ctrl Pts',(-0.791102868091814,-2.02590743034978E-5,
-0.373133150823704));
#56280=CARTESIAN_POINT('Ctrl Pts',(-0.791132983132153,-0.0293999621887177,
-0.371950982545555));
#56281=CARTESIAN_POINT('Ctrl Pts',(-0.789527747106607,-0.0587763927716652,
-0.370768814267405));
#56282=CARTESIAN_POINT('Ctrl Pts',(-0.786261896246886,-0.087967033655985,
-0.369586645989256));
#56283=CARTESIAN_POINT('Ctrl Pts',(-0.771666771745399,-0.218420338563246,
-0.364303522557596));
#56284=CARTESIAN_POINT('Ctrl Pts',(-0.723905744339962,-0.345163040037108,
-0.359020399125935));
#56285=CARTESIAN_POINT('Ctrl Pts',(-0.648778120355349,-0.452805608440245,
-0.353737275694275));
#56286=CARTESIAN_POINT('Ctrl Pts',(-0.573650496370737,-0.560448176843381,
-0.348454152262615));
#56287=CARTESIAN_POINT('Ctrl Pts',(-0.471156275806947,-0.648990612175792,
-0.343171028830956));
#56288=CARTESIAN_POINT('Ctrl Pts',(-0.35374065524607,-0.707681791005683,
-0.337887905399295));
#56289=CARTESIAN_POINT('Ctrl Pts',(-0.23632503468519,-0.766372969835576,
-0.332604781967635));
#56290=CARTESIAN_POINT('Ctrl Pts',(-0.103988014127221,-0.795212892162948,
-0.327321658535975));
#56291=CARTESIAN_POINT('Ctrl Pts',(0.0272015954388539,-0.790699716531558,
-0.322038535104315));
#56292=CARTESIAN_POINT('Ctrl Pts',(0.158391205004929,-0.786186540900168,
-0.316755411672654));
#56293=CARTESIAN_POINT('Ctrl Pts',(0.288433403579109,-0.748320267310017,
-0.311472288240994));
#56294=CARTESIAN_POINT('Ctrl Pts',(0.401538025636569,-0.68169874752446,
-0.306189164809334));
#56295=CARTESIAN_POINT('Ctrl Pts',(0.514642647694025,-0.615077227738905,
-0.300906041377674));
#56296=CARTESIAN_POINT('Ctrl Pts',(0.610809693234762,-0.519700461757946,
-0.295622917946014));
#56297=CARTESIAN_POINT('Ctrl Pts',(0.678362232218607,-0.407149420478866,
-0.290339794514354));
#56298=CARTESIAN_POINT('Ctrl Pts',(0.745914771202452,-0.294598379199785,
-0.285056671082694));
#56299=CARTESIAN_POINT('Ctrl Pts',(0.784852803629405,-0.164873062622582,
-0.279773547651034));
#56300=CARTESIAN_POINT('Ctrl Pts',(0.790448342209017,-0.0337251600679334,
-0.274490424219374));
#56301=CARTESIAN_POINT('Ctrl Pts',(0.796043880788629,0.0974227424867189,
-0.269207300787713));
#56302=CARTESIAN_POINT('Ctrl Pts',(0.768296925520898,0.229993231018817,
-0.263924177356053));
#56303=CARTESIAN_POINT('Ctrl Pts',(0.710576604148165,0.34788914704293,-0.258641053924393));
#56304=CARTESIAN_POINT('Ctrl Pts',(0.652856282775432,0.465785063067044,
-0.253357930492733));
#56305=CARTESIAN_POINT('Ctrl Pts',(0.565162595297698,0.569006406583174,
-0.248074807061072));
#56306=CARTESIAN_POINT('Ctrl Pts',(0.458143611008586,0.645019689538202,
-0.242791683629412));
#56307=CARTESIAN_POINT('Ctrl Pts',(0.351124626719476,0.721032972493228,
-0.237508560197752));
#56308=CARTESIAN_POINT('Ctrl Pts',(0.22478034561899,0.769838194887155,-0.232225436766092));
#56309=CARTESIAN_POINT('Ctrl Pts',(0.0944519125651878,0.785509263983989,
-0.226942313334432));
#56310=CARTESIAN_POINT('Ctrl Pts',(-0.0358765204886145,0.801180333080823,
-0.221659189902772));
#56311=CARTESIAN_POINT('Ctrl Pts',(-0.170189105495733,0.783717248880564,
-0.216376066471112));
#56312=CARTESIAN_POINT('Ctrl Pts',(-0.292177137732413,0.735240432042466,
-0.211092943039452));
#56313=CARTESIAN_POINT('Ctrl Pts',(-0.414165169969093,0.686763615204368,
-0.205809819607792));
#56314=CARTESIAN_POINT('Ctrl Pts',(-0.523828649435335,0.60727306572843,
-0.200526696176131));
#56315=CARTESIAN_POINT('Ctrl Pts',(-0.607851891327949,0.506420808823632,
-0.195243572744471));
#56316=CARTESIAN_POINT('Ctrl Pts',(-0.69187513322056,0.405568551918837,
-0.189960449312812));
#56317=CARTESIAN_POINT('Ctrl Pts',(-0.750258137539544,0.283354587585183,
-0.184677325881152));
#56318=CARTESIAN_POINT('Ctrl Pts',(-0.775911787358977,0.15461852632206,
-0.179394202449492));
#56319=CARTESIAN_POINT('Ctrl Pts',(-0.786045869844276,0.103763311845536,
-0.177307185240896));
#56320=CARTESIAN_POINT('Ctrl Pts',(-0.791072456914615,0.0518903082719592,
-0.1752201680323));
#56321=CARTESIAN_POINT('Ctrl Pts',(-0.791044518748003,1.1964098827608E-5,
-0.173133150823703));
#56322=CARTESIAN_POINT('Origin',(0.,0.,-4.178617978381));
#56323=CARTESIAN_POINT('',(-0.676660923651515,1.32068574775878E-5,-0.0786179783809996));
#56324=CARTESIAN_POINT('',(-0.6767,-8.45931892044317E-14,-0.0711000000000004));
#56325=CARTESIAN_POINT('',(-0.6767,-8.45931892044317E-14,-4.178617978381));
#56326=CARTESIAN_POINT('',(-0.657933019064465,-0.158364055658306,-0.0711000000000004));
#56327=CARTESIAN_POINT('Ctrl Pts',(-0.676660923651515,1.32068574776288E-5,
-0.0786179783809996));
#56328=CARTESIAN_POINT('Ctrl Pts',(-0.676624313627597,-0.0532698217775889,
-0.0761119855873332));
#56329=CARTESIAN_POINT('Ctrl Pts',(-0.670346619805526,-0.106561407057785,
-0.0736059927936668));
#56330=CARTESIAN_POINT('Ctrl Pts',(-0.657933019064465,-0.158364055658306,
-0.0711000000000003));
#56331=CARTESIAN_POINT('Origin',(0.,0.,-0.0711000000000004));
#56332=CARTESIAN_POINT('Origin',(0.,0.,-4.178617978381));
#56333=CARTESIAN_POINT('',(-0.676689663936658,-1.72930529912188E-5,-0.278617978381001));
#56334=CARTESIAN_POINT('',(-0.676652541823756,1.02339851014988E-5,-0.239182021618994));
#56335=CARTESIAN_POINT('',(-0.6767,-8.45931892044317E-14,-4.178617978381));
#56336=CARTESIAN_POINT('Ctrl Pts',(-0.676689663936658,-1.72930529912067E-5,
-0.278617978381001));
#56337=CARTESIAN_POINT('Ctrl Pts',(-0.676718536339111,-0.029267438783139,
-0.277242126993792));
#56338=CARTESIAN_POINT('Ctrl Pts',(-0.667709720174263,-0.170817385471675,
-0.270583152174923));
#56339=CARTESIAN_POINT('Ctrl Pts',(-0.570903748360253,-0.414153845586582,
-0.258641053924393));
#56340=CARTESIAN_POINT('Ctrl Pts',(-0.303782187894811,-0.636530343082252,
-0.242791683629414));
#56341=CARTESIAN_POINT('Ctrl Pts',(0.0371118910375575,-0.704327481431854,
-0.226942313334432));
#56342=CARTESIAN_POINT('Ctrl Pts',(0.36899349191975,-0.601080952691479,
-0.211092943039453));
#56343=CARTESIAN_POINT('Ctrl Pts',(0.611266154089886,-0.351863826144559,
-0.195243572744473));
#56344=CARTESIAN_POINT('Ctrl Pts',(0.705094887117879,-0.0171977214955263,
-0.179394202449492));
#56345=CARTESIAN_POINT('Ctrl Pts',(0.627693390094468,0.321644844638033,
-0.163544832154511));
#56346=CARTESIAN_POINT('Ctrl Pts',(0.39785894362146,0.58237689240233,-0.147695461859531));
#56347=CARTESIAN_POINT('Ctrl Pts',(0.071404981194182,0.701680767872716,
-0.13184609156455));
#56348=CARTESIAN_POINT('Ctrl Pts',(-0.272387992417769,0.650583340742987,
-0.11599672126957));
#56349=CARTESIAN_POINT('Ctrl Pts',(-0.550035273505243,0.441494566425662,
-0.100147350974589));
#56350=CARTESIAN_POINT('Ctrl Pts',(-0.663290191377602,0.192838810536258,
-0.0876877700117325));
#56351=CARTESIAN_POINT('Ctrl Pts',(-0.676688583350635,0.0402697372418875,
-0.0805113124805359));
#56352=CARTESIAN_POINT('Ctrl Pts',(-0.676660923651515,1.32068574776288E-5,
-0.0786179783809996));
#56353=CARTESIAN_POINT('',(-0.364065050236237,0.570420484551954,-0.0711000000000004));
#56354=CARTESIAN_POINT('Origin',(0.,0.,-0.0711000000000004));
#56355=CARTESIAN_POINT('Ctrl Pts',(-0.676652541823757,1.02339851015057E-5,
-0.239182021618994));
#56356=CARTESIAN_POINT('Ctrl Pts',(-0.676615943780199,-0.067948624078856,
-0.235985915395931));
#56357=CARTESIAN_POINT('Ctrl Pts',(-0.64961770844105,-0.248271044387699,
-0.227506685741207));
#56358=CARTESIAN_POINT('Ctrl Pts',(-0.491821179438923,-0.505535863107229,
-0.213744332654824));
#56359=CARTESIAN_POINT('Ctrl Pts',(-0.190657404081973,-0.679046628726581,
-0.197894962359843));
#56360=CARTESIAN_POINT('Ctrl Pts',(0.156805532386105,-0.687652471031271,
-0.182045592064863));
#56361=CARTESIAN_POINT('Ctrl Pts',(0.466191447257558,-0.529265333633324,
-0.166196221769883));
#56362=CARTESIAN_POINT('Ctrl Pts',(0.662358975760562,-0.242345413653074,
-0.150346851474902));
#56363=CARTESIAN_POINT('Ctrl Pts',(0.697685099148249,0.103422631371823,
-0.134497481179922));
#56364=CARTESIAN_POINT('Ctrl Pts',(0.563560339571208,0.424084008064863,
-0.118648110884941));
#56365=CARTESIAN_POINT('Ctrl Pts',(0.292616745553076,0.64173975329643,-0.102798740589961));
#56366=CARTESIAN_POINT('Ctrl Pts',(-0.0494690429576347,0.703588850062655,
-0.0869493702949807));
#56367=CARTESIAN_POINT('Ctrl Pts',(-0.269389956604521,0.630845896423734,
-0.0763831234316606));
#56368=CARTESIAN_POINT('Ctrl Pts',(-0.364065050236245,0.570420484551949,
-0.0711000000000004));
#56369=CARTESIAN_POINT('Origin',(0.,0.,-4.178617978381));
#56370=CARTESIAN_POINT('',(-0.676737173032778,1.25957128338008E-5,-0.478617978381));
#56371=CARTESIAN_POINT('',(-0.676702453340578,-1.73294345428565E-5,-0.439182021618994));
#56372=CARTESIAN_POINT('',(-0.6767,-8.45931892044317E-14,-4.178617978381));
#56373=CARTESIAN_POINT('Ctrl Pts',(-0.676737173032778,1.25957128337788E-5,
-0.478617978381));
#56374=CARTESIAN_POINT('Ctrl Pts',(-0.676652639569119,-0.0987193633761514,
-0.473972941507046));
#56375=CARTESIAN_POINT('Ctrl Pts',(-0.629917600928146,-0.30982344429185,
-0.464044781201433));
#56376=CARTESIAN_POINT('Ctrl Pts',(-0.41842147815042,-0.567783376690792,
-0.448833497464158));
#56377=CARTESIAN_POINT('Ctrl Pts',(-0.0964411493212378,-0.698679898767291,
-0.432984127169178));
#56378=CARTESIAN_POINT('Ctrl Pts',(0.248959603828383,-0.659904244480755,
-0.417134756874197));
#56379=CARTESIAN_POINT('Ctrl Pts',(0.533901314322515,-0.4608729573248,-0.401285386579217));
#56380=CARTESIAN_POINT('Ctrl Pts',(0.689186800078316,-0.149920148114908,
-0.385436016284236));
#56381=CARTESIAN_POINT('Ctrl Pts',(0.677105478124627,0.197440289037993,
-0.369586645989256));
#56382=CARTESIAN_POINT('Ctrl Pts',(0.50059125872345,0.496852984183748,-0.353737275694276));
#56383=CARTESIAN_POINT('Ctrl Pts',(0.202510055068408,0.675606522928187,
-0.337887905399296));
#56384=CARTESIAN_POINT('Ctrl Pts',(-0.144750067291325,0.690291180816235,
-0.322038535104314));
#56385=CARTESIAN_POINT('Ctrl Pts',(-0.456858098816181,0.537340835519866,
-0.306189164809335));
#56386=CARTESIAN_POINT('Ctrl Pts',(-0.640557186228658,0.278503995431137,
-0.291715645901563));
#56387=CARTESIAN_POINT('Ctrl Pts',(-0.676607669375318,0.0830500191364299,
-0.282525250425452));
#56388=CARTESIAN_POINT('Ctrl Pts',(-0.676689663936658,-1.72930529912067E-5,
-0.278617978381001));
#56389=CARTESIAN_POINT('Ctrl Pts',(-0.676702453340578,-1.73294345428357E-5,
-0.439182021618993));
#56390=CARTESIAN_POINT('Ctrl Pts',(-0.676728213481893,-0.0251484697423405,
-0.437999853340846));
#56391=CARTESIAN_POINT('Ctrl Pts',(-0.669218687692859,-0.162575651503364,
-0.431534561631038));
#56392=CARTESIAN_POINT('Ctrl Pts',(-0.57836825932194,-0.40366403145049,
-0.419786146489569));
#56393=CARTESIAN_POINT('Ctrl Pts',(-0.315350287932037,-0.63087929875971,
-0.403936776194589));
#56394=CARTESIAN_POINT('Ctrl Pts',(0.0242494914065197,-0.704887548433319,
-0.388087405899608));
#56395=CARTESIAN_POINT('Ctrl Pts',(0.357960358964906,-0.607716113702729,
-0.372238035604628));
#56396=CARTESIAN_POINT('Ctrl Pts',(0.604741700327879,-0.362962766947641,
-0.356388665309647));
#56397=CARTESIAN_POINT('Ctrl Pts',(0.704663454379142,-0.030065073630256,
-0.340539295014667));
#56398=CARTESIAN_POINT('Ctrl Pts',(0.633459948009497,0.310133825079147,
-0.324689924719686));
#56399=CARTESIAN_POINT('Ctrl Pts',(0.408422715107778,0.575017720253068,
-0.308840554424706));
#56400=CARTESIAN_POINT('Ctrl Pts',(0.0842013460493761,0.700260397514991,
-0.292991184129726));
#56401=CARTESIAN_POINT('Ctrl Pts',(-0.260468074786106,0.655447090429983,
-0.277141813834745));
#56402=CARTESIAN_POINT('Ctrl Pts',(-0.541883609692458,0.451460534380044,
-0.261292443539765));
#56403=CARTESIAN_POINT('Ctrl Pts',(-0.661492385626837,0.201081800936145,
-0.248639179467848));
#56404=CARTESIAN_POINT('Ctrl Pts',(-0.676676439886391,0.0443865144831086,
-0.241269038827591));
#56405=CARTESIAN_POINT('Ctrl Pts',(-0.676652541823757,1.02339851015057E-5,
-0.239182021618994));
#56406=CARTESIAN_POINT('Origin',(0.,0.,-4.178617978381));
#56407=CARTESIAN_POINT('',(-0.676642536276524,-2.06014658737574E-7,-0.678617978381));
#56408=CARTESIAN_POINT('',(-0.676725589147528,1.50742954787217E-5,-0.639182021618993));
#56409=CARTESIAN_POINT('',(-0.6767,-8.45931892044317E-14,-4.178617978381));
#56410=CARTESIAN_POINT('Ctrl Pts',(-0.676642536276524,-2.06014658693521E-7,
-0.678617978381));
#56411=CARTESIAN_POINT('Ctrl Pts',(-0.676643131183487,-0.0559476708465134,
-0.675986879451961));
#56412=CARTESIAN_POINT('Ctrl Pts',(-0.656004364269065,-0.224234593763904,
-0.668072657091263));
#56413=CARTESIAN_POINT('Ctrl Pts',(-0.518031279492488,-0.478641922203943,
-0.654875311298903));
#56414=CARTESIAN_POINT('Ctrl Pts',(-0.226530078974616,-0.667936089415343,
-0.639025941003923));
#56415=CARTESIAN_POINT('Ctrl Pts',(0.119983225911628,-0.695024115929475,
-0.623176570708943));
#56416=CARTESIAN_POINT('Ctrl Pts',(0.437358988551026,-0.553327761238609,
-0.607327200413961));
#56417=CARTESIAN_POINT('Ctrl Pts',(0.648523521169567,-0.277257531391908,
-0.591477830118983));
#56418=CARTESIAN_POINT('Ctrl Pts',(0.702196193133595,0.0661438022220719,
-0.575628459824));
#56419=CARTESIAN_POINT('Ctrl Pts',(0.585342767907381,0.393482325247575,
-0.559779089529022));
#56420=CARTESIAN_POINT('Ctrl Pts',(0.326340725662382,0.625264925449887,
-0.54392971923404));
#56421=CARTESIAN_POINT('Ctrl Pts',(-0.011912116922439,0.705203940498158,
-0.528080348939061));
#56422=CARTESIAN_POINT('Ctrl Pts',(-0.347272140053286,0.613886436539002,
-0.51223097864408));
#56423=CARTESIAN_POINT('Ctrl Pts',(-0.59829823587811,0.373488577025802,
-0.496381608349099));
#56424=CARTESIAN_POINT('Ctrl Pts',(-0.67304244002644,0.139426503702999,
-0.485177274928072));
#56425=CARTESIAN_POINT('Ctrl Pts',(-0.676748785355414,0.013575359070847,
-0.479256064938706));
#56426=CARTESIAN_POINT('Ctrl Pts',(-0.676737173032778,1.25957128337788E-5,
-0.478617978381));
#56427=CARTESIAN_POINT('Ctrl Pts',(-0.676725589147528,1.50742954787165E-5,
-0.639182021618993));
#56428=CARTESIAN_POINT('Ctrl Pts',(-0.676633999892269,-0.0946047616401611,
-0.6347306678541));
#56429=CARTESIAN_POINT('Ctrl Pts',(-0.632835371378299,-0.30160699551933,
-0.624996190657547));
#56430=CARTESIAN_POINT('Ctrl Pts',(-0.42871562406298,-0.560051254246869,
-0.609978590029332));
#56431=CARTESIAN_POINT('Ctrl Pts',(-0.109178218030051,-0.69680313604847,
-0.594129219734354));
#56432=CARTESIAN_POINT('Ctrl Pts',(0.236872768681544,-0.664338607305327,
-0.578279849439372));
#56433=CARTESIAN_POINT('Ctrl Pts',(0.525399961944826,-0.470541574876744,
-0.562430479144392));
#56434=CARTESIAN_POINT('Ctrl Pts',(0.686335456690993,-0.162475027583201,
-0.546581108849412));
#56435=CARTESIAN_POINT('Ctrl Pts',(0.680596583308102,0.185048059941882,
-0.530731738554432));
#56436=CARTESIAN_POINT('Ctrl Pts',(0.509577008823849,0.487632818601885,
-0.514882368259451));
#56437=CARTESIAN_POINT('Ctrl Pts',(0.214808289323237,0.67179750858231,-0.499032997964472));
#56438=CARTESIAN_POINT('Ctrl Pts',(-0.132125935456141,0.692818324582584,
-0.48318362766949));
#56439=CARTESIAN_POINT('Ctrl Pts',(-0.446973799862388,0.545590428747379,
-0.46733425737451));
#56440=CARTESIAN_POINT('Ctrl Pts',(-0.637887935546393,0.286731526864918,
-0.452667055357677));
#56441=CARTESIAN_POINT('Ctrl Pts',(-0.676613091118437,0.0871628810853665,
-0.443282976772505));
#56442=CARTESIAN_POINT('Ctrl Pts',(-0.676702453340578,-1.73294345428357E-5,
-0.439182021618993));
#56443=CARTESIAN_POINT('Origin',(0.,0.,-4.178617978381));
#56444=CARTESIAN_POINT('',(-0.676738329529131,-1.22799319098172E-5,-0.878617978381001));
#56445=CARTESIAN_POINT('',(-0.676643916272068,-3.98541505916561E-6,-0.839182021618994));
#56446=CARTESIAN_POINT('',(-0.6767,-8.45931892044317E-14,-4.178617978381));
#56447=CARTESIAN_POINT('Ctrl Pts',(-0.676738329529131,-1.22799319097634E-5,
-0.878617978381001));
#56448=CARTESIAN_POINT('Ctrl Pts',(-0.676749353176149,-0.013130197661408,
-0.878000817396877));
#56449=CARTESIAN_POINT('Ctrl Pts',(-0.673177374051864,-0.138536282933656,
-0.872100532981092));
#56450=CARTESIAN_POINT('Ctrl Pts',(-0.599033661857993,-0.372307894335739,
-0.860917125133648));
#56451=CARTESIAN_POINT('Ctrl Pts',(-0.348482163889545,-0.613200356877398,
-0.845067754838668));
#56452=CARTESIAN_POINT('Ctrl Pts',(-0.0133028882008698,-0.705179076114163,
-0.829218384543688));
#56453=CARTESIAN_POINT('Ctrl Pts',(0.325106951293811,-0.625907314579525,
-0.813369014248707));
#56454=CARTESIAN_POINT('Ctrl Pts',(0.584565608603702,-0.394635965747537,
-0.797519643953726));
#56455=CARTESIAN_POINT('Ctrl Pts',(0.702064379543393,-0.067528536190703,
-0.781670273658747));
#56456=CARTESIAN_POINT('Ctrl Pts',(0.64906906380117,0.275977982165213,-0.765820903363766));
#56457=CARTESIAN_POINT('Ctrl Pts',(0.438449404123081,0.552464131186653,
-0.749971533068786));
#56458=CARTESIAN_POINT('Ctrl Pts',(0.121353710493789,0.694786134845175,
-0.734122162773805));
#56459=CARTESIAN_POINT('Ctrl Pts',(-0.225212343175068,0.66838155024305,
-0.718272792478825));
#56460=CARTESIAN_POINT('Ctrl Pts',(-0.517086300395306,0.479662646207939,
-0.702423422183845));
#56461=CARTESIAN_POINT('Ctrl Pts',(-0.655780419625378,0.225124967968464,
-0.689205150817903));
#56462=CARTESIAN_POINT('Ctrl Pts',(-0.676641936638166,0.056392218441925,
-0.681270002883622));
#56463=CARTESIAN_POINT('Ctrl Pts',(-0.676642536276524,-2.06014658693521E-7,
-0.678617978381));
#56464=CARTESIAN_POINT('Ctrl Pts',(-0.676643916272068,-3.98541505918296E-6,
-0.839182021618994));
#56465=CARTESIAN_POINT('Ctrl Pts',(-0.676654604183955,-0.0518326861038898,
-0.836744605799016));
#56466=CARTESIAN_POINT('Ctrl Pts',(-0.658031674012512,-0.215993061705228,
-0.829024066547377));
#56467=CARTESIAN_POINT('Ctrl Pts',(-0.526681713994867,-0.469106454701526,
-0.816020403864078));
#56468=CARTESIAN_POINT('Ctrl Pts',(-0.23868430153437,-0.66368991095259,
-0.800171033569099));
#56469=CARTESIAN_POINT('Ctrl Pts',(0.107276829327393,-0.697098397350523,
-0.784321663274117));
#56470=CARTESIAN_POINT('Ctrl Pts',(0.427186125669077,-0.561218769941854,
-0.768472292979137));
#56471=CARTESIAN_POINT('Ctrl Pts',(0.643354639169021,-0.289048961179428,
-0.752622922684157));
#56472=CARTESIAN_POINT('Ctrl Pts',(0.703286538458407,0.0533154623200356,
-0.736773552389177));
#56473=CARTESIAN_POINT('Ctrl Pts',(0.592427553686509,0.38273239650208,-0.720924182094196));
#56474=CARTESIAN_POINT('Ctrl Pts',(0.337699434353656,0.619203993637335,
-0.705074811799215));
#56475=CARTESIAN_POINT('Ctrl Pts',(0.00096208864391743,0.705303883503167,
-0.689225441504236));
#56476=CARTESIAN_POINT('Ctrl Pts',(-0.336008897212553,0.620122983522791,
-0.673376071209255));
#56477=CARTESIAN_POINT('Ctrl Pts',(-0.591381198224044,0.384347202521759,
-0.657526700914275));
#56478=CARTESIAN_POINT('Ctrl Pts',(-0.671751029522471,0.14766660228095,
-0.646128684384187));
#56479=CARTESIAN_POINT('Ctrl Pts',(-0.676742703303884,0.0176955179453271,
-0.64001379128576));
#56480=CARTESIAN_POINT('Ctrl Pts',(-0.676725589147528,1.50742954787165E-5,
-0.639182021618993));
#56481=CARTESIAN_POINT('Origin',(0.,0.,-4.178617978381));
#56482=CARTESIAN_POINT('',(-0.676688317179324,1.72353111514132E-5,-1.078617978381));
#56483=CARTESIAN_POINT('',(-0.676747836763073,-8.96412734507912E-6,-1.03918202161899));
#56484=CARTESIAN_POINT('',(-0.6767,-8.45931892044317E-14,-4.178617978381));
#56485=CARTESIAN_POINT('Ctrl Pts',(-0.676688317179324,1.72353111514319E-5,
-1.078617978381));
#56486=CARTESIAN_POINT('Ctrl Pts',(-0.676607315101875,-0.0826056787905753,
-1.07473163191013));
#56487=CARTESIAN_POINT('Ctrl Pts',(-0.640840351711829,-0.277614899869378,
-1.0655621620076));
#56488=CARTESIAN_POINT('Ctrl Pts',(-0.45791694746335,-0.536438780709928,
-1.05110956867341));
#56489=CARTESIAN_POINT('Ctrl Pts',(-0.146111169363581,-0.69000436405208,
-1.03526019837843));
#56490=CARTESIAN_POINT('Ctrl Pts',(0.201177238393133,-0.676004596860274,
-1.01941082808345));
#56491=CARTESIAN_POINT('Ctrl Pts',(0.49961039794122,-0.497839277772177,
-1.00356145778847));
#56492=CARTESIAN_POINT('Ctrl Pts',(0.676714772016422,-0.198775284073422,
-0.987712087493491));
#56493=CARTESIAN_POINT('Ctrl Pts',(0.689481130432523,0.148560650918064,
-0.971862717198511));
#56494=CARTESIAN_POINT('Ctrl Pts',(0.53480920392387,0.459819107499921,-0.956013346903531));
#56495=CARTESIAN_POINT('Ctrl Pts',(0.250260574610009,0.659411966087648,
-0.94016397660855));
#56496=CARTESIAN_POINT('Ctrl Pts',(-0.0950630339562937,0.698868740035448,
-0.92431460631357));
#56497=CARTESIAN_POINT('Ctrl Pts',(-0.417300889101903,0.568607478123943,
-0.908465236018589));
#56498=CARTESIAN_POINT('Ctrl Pts',(-0.629596992258038,0.31071086642954,
-0.893233026707733));
#56499=CARTESIAN_POINT('Ctrl Pts',(-0.676654986731472,0.0991639691995475,
-0.883283940828537));
#56500=CARTESIAN_POINT('Ctrl Pts',(-0.676738329529131,-1.22799319097634E-5,
-0.878617978381001));
#56501=CARTESIAN_POINT('Ctrl Pts',(-0.676747836763073,-8.96412734503922E-6,
-1.03918202161899));
#56502=CARTESIAN_POINT('Ctrl Pts',(-0.676753746890542,-0.0090097302053093,
-1.03875854374393));
#56503=CARTESIAN_POINT('Ctrl Pts',(-0.674383982793645,-0.130296973834658,
-1.03305194243721));
#56504=CARTESIAN_POINT('Ctrl Pts',(-0.605729665760521,-0.361311590897459,
-1.02206221769882));
#56505=CARTESIAN_POINT('Ctrl Pts',(-0.359616966834596,-0.606737283232118,
-1.00621284740384));
#56506=CARTESIAN_POINT('Ctrl Pts',(-0.0261724389449761,-0.704818769002982,
-0.990363477108863));
#56507=CARTESIAN_POINT('Ctrl Pts',(0.313627981942751,-0.631737273430753,
-0.974514106813883));
#56508=CARTESIAN_POINT('Ctrl Pts',(0.5772648515989,-0.405240403720689,-0.958664736518902));
#56509=CARTESIAN_POINT('Ctrl Pts',(0.700714800347687,-0.0803321994775939,
-0.942815366223922));
#56510=CARTESIAN_POINT('Ctrl Pts',(0.653998403401114,0.264084422198656,
-0.926965995928941));
#56511=CARTESIAN_POINT('Ctrl Pts',(0.44846058817974,0.544368987497165,-0.911116625633962));
#56512=CARTESIAN_POINT('Ctrl Pts',(0.134015555013097,0.692455287158485,
-0.89526725533898));
#56513=CARTESIAN_POINT('Ctrl Pts',(-0.212974726593566,0.672381037456889,
-0.879417885044001));
#56514=CARTESIAN_POINT('Ctrl Pts',(-0.508244777755666,0.489021205658097,
-0.86356851474902));
#56515=CARTESIAN_POINT('Ctrl Pts',(-0.653661894356427,0.233365601831161,
-0.850156560274017));
#56516=CARTESIAN_POINT('Ctrl Pts',(-0.676631438026886,0.0605065466184489,
-0.842027729230676));
#56517=CARTESIAN_POINT('Ctrl Pts',(-0.676643916272068,-3.98541505918296E-6,
-0.839182021618994));
#56518=CARTESIAN_POINT('Origin',(0.,0.,-4.178617978381));
#56519=CARTESIAN_POINT('',(-0.676661399215972,-1.33519825231872E-5,-1.278617978381));
#56520=CARTESIAN_POINT('',(-0.676676376008853,1.62256556966722E-5,-1.23918202161899));
#56521=CARTESIAN_POINT('',(-0.6767,-8.45931892044317E-14,-4.178617978381));
#56522=CARTESIAN_POINT('Ctrl Pts',(-0.676661399215972,-1.3351982523134E-5,
-1.278617978381));
#56523=CARTESIAN_POINT('Ctrl Pts',(-0.676689839809335,-0.0398249105762218,
-1.27674556985505));
#56524=CARTESIAN_POINT('Ctrl Pts',(-0.663481583410436,-0.191948734974615,
-1.26959003789743));
#56525=CARTESIAN_POINT('Ctrl Pts',(-0.550903588163435,-0.440408597523208,
-1.25715138250816));
#56526=CARTESIAN_POINT('Ctrl Pts',(-0.273671211948421,-0.650045047650077,
-1.24130201221318));
#56527=CARTESIAN_POINT('Ctrl Pts',(0.0700213418398019,-0.70182013928831,
-1.2254526419182));
#56528=CARTESIAN_POINT('Ctrl Pts',(0.396709436958603,-0.583160457208559,
-1.20960327162322));
#56529=CARTESIAN_POINT('Ctrl Pts',(0.627057915507849,-0.322882125275867,
-1.19375390132824));
#56530=CARTESIAN_POINT('Ctrl Pts',(0.705127387008331,0.0158070969666729,
-1.17790453103325));
#56531=CARTESIAN_POINT('Ctrl Pts',(0.611958930271261,0.35065761632248,-1.16205516073828));
#56532=CARTESIAN_POINT('Ctrl Pts',(0.37017820670576,0.600352056300146,-1.14620579044329));
#56533=CARTESIAN_POINT('Ctrl Pts',(0.0385008908891459,0.704252921630042,
-1.13035642014832));
#56534=CARTESIAN_POINT('Ctrl Pts',(-0.302526243006624,0.637128219839621,
-1.11450704985333));
#56535=CARTESIAN_POINT('Ctrl Pts',(-0.570085847425583,0.41527896983686,
-1.09865767955835));
#56536=CARTESIAN_POINT('Ctrl Pts',(-0.667542007044258,0.171707850430491,
-1.08669465573424));
#56537=CARTESIAN_POINT('Ctrl Pts',(-0.676717429827001,0.0297124217068367,
-1.08001475534179));
#56538=CARTESIAN_POINT('Ctrl Pts',(-0.676688317179324,1.72353111514319E-5,
-1.078617978381));
#56539=CARTESIAN_POINT('Ctrl Pts',(-0.676676376008853,1.62256556967139E-5,
-1.23918202161899));
#56540=CARTESIAN_POINT('Ctrl Pts',(-0.676605980702497,-0.0784930040488071,
-1.23548935825719));
#56541=CARTESIAN_POINT('Ctrl Pts',(-0.643413256117644,-0.269384004288173,
-1.22651357146372));
#56542=CARTESIAN_POINT('Ctrl Pts',(-0.467632374358977,-0.527990962186469,
-1.21225466123859));
#56543=CARTESIAN_POINT('Ctrl Pts',(-0.158681606577905,-0.687222410456076,
-1.19640529094361));
#56544=CARTESIAN_POINT('Ctrl Pts',(0.188804481289216,-0.679564096715178,
-1.18055592064863));
#56545=CARTESIAN_POINT('Ctrl Pts',(0.490440005394944,-0.506875817935137,
-1.16470655035365));
#56546=CARTESIAN_POINT('Ctrl Pts',(0.67297374449562,-0.211094369699316,
-1.14885718005867));
#56547=CARTESIAN_POINT('Ctrl Pts',(0.692077964492487,0.135950670329878,
-1.13300780976369));
#56548=CARTESIAN_POINT('Ctrl Pts',(0.543113266727756,0.449980525360276,
-1.1171584394687));
#56549=CARTESIAN_POINT('Ctrl Pts',(0.262255251094087,0.654734050567698,
-1.10130906917373));
#56550=CARTESIAN_POINT('Ctrl Pts',(-0.0822906125712717,0.700487507941325,
-1.08545969887874));
#56551=CARTESIAN_POINT('Ctrl Pts',(-0.406852464454183,0.576129816852735,
-1.06961032858376));
#56552=CARTESIAN_POINT('Ctrl Pts',(-0.626579463050419,0.318921822910923,
-1.05418443616385));
#56553=CARTESIAN_POINT('Ctrl Pts',(-0.676680014743584,0.103279862638811,
-1.04404166717559));
#56554=CARTESIAN_POINT('Ctrl Pts',(-0.676747836763073,-8.96412734503922E-6,
-1.03918202161899));
#56555=CARTESIAN_POINT('Origin',(0.,0.,-4.178617978381));
#56556=CARTESIAN_POINT('',(-0.67675648621479,3.15325649049231E-6,-1.478617978381));
#56557=CARTESIAN_POINT('',(-0.676671333621808,-1.54941563473843E-5,-1.43918202161899));
#56558=CARTESIAN_POINT('',(-0.6767,-8.45931892044317E-14,-4.178617978381));
#56559=CARTESIAN_POINT('Ctrl Pts',(-0.67675648621479,3.15325649049647E-6,
-1.478617978381));
#56560=CARTESIAN_POINT('Ctrl Pts',(-0.676727987849731,-0.109274258141125,
-1.4734763843683));
#56561=CARTESIAN_POINT('Ctrl Pts',(-0.622024114183857,-0.330864596680709,
-1.46305166692394));
#56562=CARTESIAN_POINT('Ctrl Pts',(-0.391401124376496,-0.58673644514426,
-1.44734382604792));
#56563=CARTESIAN_POINT('Ctrl Pts',(-0.0636496855493053,-0.702426660764798,
-1.43149445575294));
#56564=CARTESIAN_POINT('Ctrl Pts',(0.279558875618117,-0.647534810868762,
-1.41564508545796));
#56565=CARTESIAN_POINT('Ctrl Pts',(0.554877458941432,-0.435391205449084,
-1.39979571516298));
#56566=CARTESIAN_POINT('Ctrl Pts',(0.695445827983648,-0.117514239834355,
-1.383946344868));
#56567=CARTESIAN_POINT('Ctrl Pts',(0.667127404398765,0.228900682663626,
-1.36809697457302));
#56568=CARTESIAN_POINT('Ctrl Pts',(0.476799226683618,0.51972780727763,-1.35224760427804));
#56569=CARTESIAN_POINT('Ctrl Pts',(0.170681883398015,0.684340697973908,
-1.33639823398306));
#56570=CARTESIAN_POINT('Ctrl Pts',(-0.176885008776566,0.682763641309219,
-1.32054886368808));
#56571=CARTESIAN_POINT('Ctrl Pts',(-0.481495942925332,0.515379620445116,
-1.3046994933931));
#56572=CARTESIAN_POINT('Ctrl Pts',(-0.647004900930806,0.257397591632518,
-1.29072253162407));
#56573=CARTESIAN_POINT('Ctrl Pts',(-0.676609592810283,0.0725060124792107,
-1.28202869328671));
#56574=CARTESIAN_POINT('Ctrl Pts',(-0.676661399215972,-1.3351982523134E-5,
-1.278617978381));
#56575=CARTESIAN_POINT('Ctrl Pts',(-0.676671333621808,-1.54941563473114E-5,
-1.43918202161899));
#56576=CARTESIAN_POINT('Ctrl Pts',(-0.676701550046883,-0.0357074174336674,
-1.4375032962021));
#56577=CARTESIAN_POINT('Ctrl Pts',(-0.665192670506278,-0.183706237481266,
-1.43054144735355));
#56578=CARTESIAN_POINT('Ctrl Pts',(-0.558850665837655,-0.430279475448245,
-1.41829647507333));
#56579=CARTESIAN_POINT('Ctrl Pts',(-0.285491011948519,-0.64494137392155,
-1.40244710477835));
#56580=CARTESIAN_POINT('Ctrl Pts',(0.0571992200988665,-0.7029813247301,
-1.38659773448337));
#56581=CARTESIAN_POINT('Ctrl Pts',(0.385998804687375,-0.590304511654048,
-1.37074836418839));
#56582=CARTESIAN_POINT('Ctrl Pts',(0.62105981545978,-0.334274137977006,
-1.35489899389341));
#56583=CARTESIAN_POINT('Ctrl Pts',(0.705298438575201,0.00293363981907094,
-1.33904962359843));
#56584=CARTESIAN_POINT('Ctrl Pts',(0.618257594127741,0.339428992578101,
-1.32320025330345));
#56585=CARTESIAN_POINT('Ctrl Pts',(0.381074872501545,0.593495101283185,
-1.30735088300847));
#56586=CARTESIAN_POINT('Ctrl Pts',(0.0513493382249849,0.703432824911564,
-1.29150151271349));
#56587=CARTESIAN_POINT('Ctrl Pts',(-0.290846218427701,0.642544139281894,
-1.27565214241851));
#56588=CARTESIAN_POINT('Ctrl Pts',(-0.562410702175123,0.425615666744179,
-1.25980277212353));
#56589=CARTESIAN_POINT('Ctrl Pts',(-0.66594612195667,0.179950018736301,
-1.24764606519036));
#56590=CARTESIAN_POINT('Ctrl Pts',(-0.676706695838444,0.0338307878633588,
-1.24077248168885));
#56591=CARTESIAN_POINT('Ctrl Pts',(-0.676676376008853,1.62256556967139E-5,
-1.23918202161899));
#56592=CARTESIAN_POINT('Origin',(0.,0.,-4.178617978381));
#56593=CARTESIAN_POINT('',(-0.676650274159548,9.11169281612442E-6,-1.678617978381));
#56594=CARTESIAN_POINT('',(-0.6767513059161,7.24714397432741E-6,-1.63918202161899));
#56595=CARTESIAN_POINT('',(-0.6767,-8.45931892044317E-14,-4.178617978381));
#56596=CARTESIAN_POINT('Ctrl Pts',(-0.676650274159548,9.11169281613E-6,
-1.678617978381));
#56597=CARTESIAN_POINT('Ctrl Pts',(-0.676618550586515,-0.0664949256843561,
-1.67549032231322));
#56598=CARTESIAN_POINT('Ctrl Pts',(-0.650429330989842,-0.245359622697372,
-1.66707954281377));
#56599=CARTESIAN_POINT('Ctrl Pts',(-0.495072108323442,-0.502352569202039,
-1.65338563988267));
#56600=CARTESIAN_POINT('Ctrl Pts',(-0.195034448742293,-0.677802375348079,
-1.63753626958769));
#56601=CARTESIAN_POINT('Ctrl Pts',(0.152366702248935,-0.688650044848245,
-1.62168689929271));
#56602=CARTESIAN_POINT('Ctrl Pts',(0.462766087451164,-0.532261255896812,
-1.60583752899773));
#56603=CARTESIAN_POINT('Ctrl Pts',(0.660784210013829,-0.246614525160438,
-1.58998815870274));
#56604=CARTESIAN_POINT('Ctrl Pts',(0.698333002892782,0.0989217533935704,
-1.57413878840777));
#56605=CARTESIAN_POINT('Ctrl Pts',(0.566293861962189,0.420435200866502,
-1.55828941811278));
#56606=CARTESIAN_POINT('Ctrl Pts',(0.296732069830279,0.639847305970687,
-1.54244004781781));
#56607=CARTESIAN_POINT('Ctrl Pts',(-0.0448901553745235,0.703874541501651,
-1.52659067752282));
#56608=CARTESIAN_POINT('Ctrl Pts',(-0.37561095007723,0.596968098314967,
-1.51074130722784));
#56609=CARTESIAN_POINT('Ctrl Pts',(-0.615115828195774,0.345089863842356,
-1.49489193693286));
#56610=CARTESIAN_POINT('Ctrl Pts',(-0.67600460121947,0.118304202037452,
-1.48418416065058));
#56611=CARTESIAN_POINT('Ctrl Pts',(-0.67675727067133,0.00301116371053214,
-1.47875950779996));
#56612=CARTESIAN_POINT('Ctrl Pts',(-0.67675648621479,3.15325649049647E-6,
-1.478617978381));
#56613=CARTESIAN_POINT('Ctrl Pts',(-0.6767513059161,7.24714397433088E-6,
-1.63918202161899));
#56614=CARTESIAN_POINT('Ctrl Pts',(-0.676693498218469,-0.105156040632668,
-1.63423411071536));
#56615=CARTESIAN_POINT('Ctrl Pts',(-0.625174216556339,-0.322661917470327,
-1.62400307638006));
#56616=CARTESIAN_POINT('Ctrl Pts',(-0.402045725983278,-0.579494372636858,
-1.6084889186131));
#56617=CARTESIAN_POINT('Ctrl Pts',(-0.0764606078631723,-0.701147822605475,
-1.59263954831812));
#56618=CARTESIAN_POINT('Ctrl Pts',(0.267692724062702,-0.652529768809897,
-1.57679017802314));
#56619=CARTESIAN_POINT('Ctrl Pts',(0.54683773505632,-0.445446949947669,
-1.56094080772816));
#56620=CARTESIAN_POINT('Ctrl Pts',(0.693184952972512,-0.130188765535679,
-1.54509143743318));
#56621=CARTESIAN_POINT('Ctrl Pts',(0.671194424519117,0.216685343744462,
-1.5292420671382));
#56622=CARTESIAN_POINT('Ctrl Pts',(0.486206479121138,0.510938111085708,
-1.51339269684322));
#56623=CARTESIAN_POINT('Ctrl Pts',(0.183144847018672,0.681111194086335,
-1.49754332654823));
#56624=CARTESIAN_POINT('Ctrl Pts',(-0.16439292478377,0.685878604404777,
-1.48169395625326));
#56625=CARTESIAN_POINT('Ctrl Pts',(-0.472008401160537,0.524082591709629,
-1.46584458595827));
#56626=CARTESIAN_POINT('Ctrl Pts',(-0.644557160212723,0.265632132741012,
-1.45167394108019));
#56627=CARTESIAN_POINT('Ctrl Pts',(-0.676606455815432,0.0766187761712225,
-1.44278641963376));
#56628=CARTESIAN_POINT('Ctrl Pts',(-0.676671333621808,-1.54941563473114E-5,
-1.43918202161899));
#56629=CARTESIAN_POINT('Origin',(0.,0.,-4.178617978381));
#56630=CARTESIAN_POINT('',(-0.676707048125263,-1.71239118336567E-5,-1.878617978381));
#56631=CARTESIAN_POINT('',(-0.676645363994687,5.65701016097542E-6,-1.839182021619));
#56632=CARTESIAN_POINT('',(-0.6767,-8.45931892044317E-14,-4.178617978381));
#56633=CARTESIAN_POINT('Ctrl Pts',(-0.676707048125263,-1.71239118336441E-5,
-1.878617978381));
#56634=CARTESIAN_POINT('Ctrl Pts',(-0.676731370348907,-0.0236926529716641,
-1.87750426025813));
#56635=CARTESIAN_POINT('Ctrl Pts',(-0.669733324470885,-0.15966303113128,
-1.8711074187036));
#56636=CARTESIAN_POINT('Ctrl Pts',(-0.580960354995419,-0.399924445548537,
-1.85942745371742));
#56637=CARTESIAN_POINT('Ctrl Pts',(-0.319413674149484,-0.628831774793575,
-1.84357808342243));
#56638=CARTESIAN_POINT('Ctrl Pts',(0.0197015947556392,-0.705029320941897,
-1.82772871312745));
#56639=CARTESIAN_POINT('Ctrl Pts',(0.354032394455494,-0.610012753882915,
-1.81187934283247));
#56640=CARTESIAN_POINT('Ctrl Pts',(0.602387560713073,-0.366856542700088,
-1.79602997253749));
#56641=CARTESIAN_POINT('Ctrl Pts',(0.704454836593539,-0.0346103947345185,
-1.78018060224251));
#56642=CARTESIAN_POINT('Ctrl Pts',(0.635447510951297,0.306040776775757,
-1.76433123194753));
#56643=CARTESIAN_POINT('Ctrl Pts',(0.412123791868901,0.572370925536324,
-1.74848186165255));
#56644=CARTESIAN_POINT('Ctrl Pts',(0.0887171294811145,0.699702627664309,
-1.73263249135757));
#56645=CARTESIAN_POINT('Ctrl Pts',(-0.256234203744069,0.657113786992292,
-1.71678312106259));
#56646=CARTESIAN_POINT('Ctrl Pts',(-0.53895988100815,0.454946967115278,
-1.70093375076761));
#56647=CARTESIAN_POINT('Ctrl Pts',(-0.660837136749363,0.203994775542709,
-1.68821203654041));
#56648=CARTESIAN_POINT('Ctrl Pts',(-0.676672136897923,0.045841287298366,
-1.68077344574488));
#56649=CARTESIAN_POINT('Ctrl Pts',(-0.676650274159548,9.11169281613E-6,
-1.678617978381));
#56650=CARTESIAN_POINT('Ctrl Pts',(-0.676645363994687,5.65701016099623E-6,
-1.839182021619));
#56651=CARTESIAN_POINT('Ctrl Pts',(-0.676627054762735,-0.0623813489974528,
-1.83624804866027));
#56652=CARTESIAN_POINT('Ctrl Pts',(-0.65266894145479,-0.237120680884818,
-1.82803095226989));
#56653=CARTESIAN_POINT('Ctrl Pts',(-0.504159162883881,-0.493232229461368,
-1.81453073244784));
#56654=CARTESIAN_POINT('Ctrl Pts',(-0.207374009842694,-0.67412944880117,
-1.79868136215287));
#56655=CARTESIAN_POINT('Ctrl Pts',(0.139771257512638,-0.691316489946928,
-1.78283199185788));
#56656=CARTESIAN_POINT('Ctrl Pts',(0.45297352250471,-0.540619534986371,
-1.7669826215629));
#56657=CARTESIAN_POINT('Ctrl Pts',(0.656172617900346,-0.258634856925766,
-1.75113325126792));
#56658=CARTESIAN_POINT('Ctrl Pts',(0.700022293991506,0.0861584680346388,
-1.73528388097294));
#56659=CARTESIAN_POINT('Ctrl Pts',(0.573873797338617,0.410028484897529,
-1.71943451067796));
#56660=CARTESIAN_POINT('Ctrl Pts',(0.308361886447897,0.634324397044211,
-1.70358514038298));
#56661=CARTESIAN_POINT('Ctrl Pts',(-0.0320347212446137,0.704576660367049,
-1.687735770088));
#56662=CARTESIAN_POINT('Ctrl Pts',(-0.364651799452575,0.603724737653847,
-1.67188639979302));
#56663=CARTESIAN_POINT('Ctrl Pts',(-0.608714355716241,0.356260195424872,
-1.65603702949804));
#56664=CARTESIAN_POINT('Ctrl Pts',(-0.6749086000968,0.126542401434684,-1.6451355701067));
#56665=CARTESIAN_POINT('Ctrl Pts',(-0.676755222289058,0.00713188059781006,
-1.63951723414702));
#56666=CARTESIAN_POINT('Ctrl Pts',(-0.6767513059161,7.24714397433088E-6,
-1.63918202161899));
#56667=CARTESIAN_POINT('Origin',(0.,0.,-4.178617978381));
#56668=CARTESIAN_POINT('',(-0.676721208628825,1.57472380184304E-5,-2.078617978381));
#56669=CARTESIAN_POINT('',(-0.676719918585588,-1.59214003083719E-5,-2.039182021619));
#56670=CARTESIAN_POINT('',(-0.6767,-8.45931892044317E-14,-4.178617978381));
#56671=CARTESIAN_POINT('Ctrl Pts',(-0.676721208628825,1.57472380184313E-5,
-2.078617978381));
#56672=CARTESIAN_POINT('Ctrl Pts',(-0.676628683042819,-0.0931508258832454,
-2.07423507477139));
#56673=CARTESIAN_POINT('Ctrl Pts',(-0.633845182230617,-0.298702118546585,
-2.06456904773011));
#56674=CARTESIAN_POINT('Ctrl Pts',(-0.432319723520416,-0.557273858061672,
-2.04961989725718));
#56675=CARTESIAN_POINT('Ctrl Pts',(-0.113671183958779,-0.69608430391808,
-2.0337705269622));
#56676=CARTESIAN_POINT('Ctrl Pts',(0.232582038671535,-0.665852905311,-2.01792115666722));
#56677=CARTESIAN_POINT('Ctrl Pts',(0.522353457898419,-0.473921260596391,
-2.00207178637224));
#56678=CARTESIAN_POINT('Ctrl Pts',(0.685273012361204,-0.166899355160858,
-1.98622241607726));
#56679=CARTESIAN_POINT('Ctrl Pts',(0.681776209899179,0.180653524292269,
-1.97037304578227));
#56680=CARTESIAN_POINT('Ctrl Pts',(0.512712237794087,0.484335273792739,
-1.9545236754873));
#56681=CARTESIAN_POINT('Ctrl Pts',(0.219137740357689,0.670397752811446,
-1.93867430519231));
#56682=CARTESIAN_POINT('Ctrl Pts',(-0.12765365568297,0.693656284058958,
-1.92282493489733));
#56683=CARTESIAN_POINT('Ctrl Pts',(-0.443444770166212,0.548462607691666,
-1.90697556460235));
#56684=CARTESIAN_POINT('Ctrl Pts',(-0.636923641371969,0.289638431046473,
-1.89223991243024));
#56685=CARTESIAN_POINT('Ctrl Pts',(-0.676615993480196,0.0886165029668635,
-1.88278738368979));
#56686=CARTESIAN_POINT('Ctrl Pts',(-0.676707048125263,-1.71239118336441E-5,
-1.878617978381));
#56687=CARTESIAN_POINT('Ctrl Pts',(-0.676719918585588,-1.59214003083753E-5,
-2.039182021619));
#56688=CARTESIAN_POINT('Ctrl Pts',(-0.676739457480622,-0.0195730432971318,
-2.03826198660519));
#56689=CARTESIAN_POINT('Ctrl Pts',(-0.671136992488532,-0.151422004354565,
-2.03205882815972));
#56690=CARTESIAN_POINT('Ctrl Pts',(-0.588163460150873,-0.38925343651991,
-2.02057254628259));
#56691=CARTESIAN_POINT('Ctrl Pts',(-0.330838643304082,-0.622896689504703,
-2.00472317598761));
#56692=CARTESIAN_POINT('Ctrl Pts',(0.00682927878028947,-0.705271475852064,
-1.98887380569263));
#56693=CARTESIAN_POINT('Ctrl Pts',(0.342838732379053,-0.616373342447522,
-1.97302443539765));
#56694=CARTESIAN_POINT('Ctrl Pts',(0.59559089753061,-0.377790916351739,
-1.95717506510267));
#56695=CARTESIAN_POINT('Ctrl Pts',(0.703705720197163,-0.0474631758419071,
-1.94132569480769));
#56696=CARTESIAN_POINT('Ctrl Pts',(0.640927861859323,0.294390844952153,
-1.92547632451271));
#56697=CARTESIAN_POINT('Ctrl Pts',(0.422502724410463,0.56475299163877,-1.90962695421772));
#56698=CARTESIAN_POINT('Ctrl Pts',(0.101474153120063,0.697966682548511,
-1.89377758392275));
#56699=CARTESIAN_POINT('Ctrl Pts',(-0.244197091352646,0.661681399371415,
-1.87792821362777));
#56700=CARTESIAN_POINT('Ctrl Pts',(-0.53056585406773,0.464708906947766,
-1.86207884333278));
#56701=CARTESIAN_POINT('Ctrl Pts',(-0.658928445463778,0.212237031353743,
-1.84916344599653));
#56702=CARTESIAN_POINT('Ctrl Pts',(-0.676660023687023,0.049957196008536,
-1.84153117209193));
#56703=CARTESIAN_POINT('Ctrl Pts',(-0.676645363994687,5.65701016099623E-6,
-1.839182021619));
#56704=CARTESIAN_POINT('Origin',(0.,0.,-4.178617978381));
#56705=CARTESIAN_POINT('',(-0.676644996800385,-5.2859233725154E-6,-2.278617978381));
#56706=CARTESIAN_POINT('',(-0.676708376272384,1.70429511678338E-5,-2.23918202161899));
#56707=CARTESIAN_POINT('',(-0.6767,-8.45931892044317E-14,-4.178617978381));
#56708=CARTESIAN_POINT('Ctrl Pts',(-0.676644996800385,-5.28592337248335E-6,
-2.278617978381));
#56709=CARTESIAN_POINT('Ctrl Pts',(-0.676658801146923,-0.0503782471512948,
-2.2762490127163));
#56710=CARTESIAN_POINT('Ctrl Pts',(-0.658728598412653,-0.213080253371554,
-2.26859692361994));
#56711=CARTESIAN_POINT('Ctrl Pts',(-0.529697069227978,-0.465698948973474,
-2.25566171109192));
#56712=CARTESIAN_POINT('Ctrl Pts',(-0.24296095180248,-0.662136294219658,
-2.23981234079694));
#56713=CARTESIAN_POINT('Ctrl Pts',(0.102777454848793,-0.69777596046189,
-2.22396297050196));
#56714=CARTESIAN_POINT('Ctrl Pts',(0.423556685665886,-0.563962968865366,
-2.20811360020698));
#56715=CARTESIAN_POINT('Ctrl Pts',(0.641476531525165,-0.293193375992965,
-2.192264229912));
#56716=CARTESIAN_POINT('Ctrl Pts',(0.70361585560182,0.048777289484231,-2.17641485961702));
#56717=CARTESIAN_POINT('Ctrl Pts',(0.59488432200333,0.378902546386728,-2.16056548932204));
#56718=CARTESIAN_POINT('Ctrl Pts',(0.341687035524299,0.617012533080427,
-2.14471611902706));
#56719=CARTESIAN_POINT('Ctrl Pts',(0.00551214649170594,0.70528300168426,
-2.12886674873208));
#56720=CARTESIAN_POINT('Ctrl Pts',(-0.332001349667448,0.622277751524753,
-2.1130173784371));
#56721=CARTESIAN_POINT('Ctrl Pts',(-0.588889381071465,0.388154341834502,
-2.09716800814212));
#56722=CARTESIAN_POINT('Ctrl Pts',(-0.671276237328251,0.150578921577801,
-2.08570154145675));
#56723=CARTESIAN_POINT('Ctrl Pts',(-0.676740212780864,0.0191515538507402,
-2.07951819820305));
#56724=CARTESIAN_POINT('Ctrl Pts',(-0.676721208628825,1.57472380184313E-5,
-2.078617978381));
#56725=CARTESIAN_POINT('Ctrl Pts',(-0.676708376272384,1.704295116782E-5,
-2.23918202161899));
#56726=CARTESIAN_POINT('Ctrl Pts',(-0.676616933198787,-0.0890373128188941,
-2.23499280111844));
#56727=CARTESIAN_POINT('Ctrl Pts',(-0.6366424413202,-0.290479846329372,
-2.22552045718623));
#56728=CARTESIAN_POINT('Ctrl Pts',(-0.442419721672428,-0.549289799263099,
-2.21076498982235));
#56729=CARTESIAN_POINT('Ctrl Pts',(-0.126358004157817,-0.693893470559033,
-2.19491561952737));
#56730=CARTESIAN_POINT('Ctrl Pts',(0.220389350089783,-0.669987334258051,
-2.17906624923239));
#56731=CARTESIAN_POINT('Ctrl Pts',(0.513615856317125,-0.483376919017481,
-2.16321687893741));
#56732=CARTESIAN_POINT('Ctrl Pts',(0.682112396348077,-0.179379966683827,
-2.14736750864243));
#56733=CARTESIAN_POINT('Ctrl Pts',(0.684960124933254,0.168178836214988,
-2.13151813834745));
#56734=CARTESIAN_POINT('Ctrl Pts',(0.521467480303687,0.474895947218893,
-2.11566876805247));
#56735=CARTESIAN_POINT('Ctrl Pts',(0.231338127732153,0.666286097976378,
-2.09981939775749));
#56736=CARTESIAN_POINT('Ctrl Pts',(-0.114970948453971,0.695870803174554,
-2.08397002746251));
#56737=CARTESIAN_POINT('Ctrl Pts',(-0.433359697925381,0.556465511881219,
-2.06812065716753));
#56738=CARTESIAN_POINT('Ctrl Pts',(-0.634135429768427,0.297861104444726,
-2.05319132188636));
#56739=CARTESIAN_POINT('Ctrl Pts',(-0.676627259148345,0.0927299532173215,
-2.04354511003685));
#56740=CARTESIAN_POINT('Ctrl Pts',(-0.676719918585588,-1.59214003083753E-5,
-2.039182021619));
#56741=CARTESIAN_POINT('Origin',(0.,0.,-4.178617978381));
#56742=CARTESIAN_POINT('',(-0.676750583136638,-7.642249214652E-6,-2.478617978381));
#56743=CARTESIAN_POINT('',(-0.67664966423598,-8.77515312422417E-6,-2.43918202161899));
#56744=CARTESIAN_POINT('',(-0.6767,-8.45931892044317E-14,-4.178617978381));
#56745=CARTESIAN_POINT('Ctrl Pts',(-0.676750583136638,-7.6422492146077E-6,
-2.478617978381));
#56746=CARTESIAN_POINT('Ctrl Pts',(-0.676754922059666,-0.00755345283786624,
-2.47826295066122));
#56747=CARTESIAN_POINT('Ctrl Pts',(-0.674792200770675,-0.127385273327122,
-2.47262479950977));
#56748=CARTESIAN_POINT('Ctrl Pts',(-0.608047966749425,-0.357396371491931,
-2.46170352492667));
#56749=CARTESIAN_POINT('Ctrl Pts',(-0.363523686348719,-0.604404687016196,
-2.44585415463169));
#56750=CARTESIAN_POINT('Ctrl Pts',(-0.0307188426589624,-0.704635259499128,
-2.43000478433671));
#56751=CARTESIAN_POINT('Ctrl Pts',(0.309545973614037,-0.633747415334411,
-2.41415541404173));
#56752=CARTESIAN_POINT('Ctrl Pts',(0.574638541308189,-0.408956040506685,
-2.39830604374675));
#56753=CARTESIAN_POINT('Ctrl Pts',(0.700181979140083,-0.0848510006492837,
-2.38245667345177));
#56754=CARTESIAN_POINT('Ctrl Pts',(0.655688465200883,0.259859833037388,
-2.36660730315679));
#56755=CARTESIAN_POINT('Ctrl Pts',(0.451963106890093,0.54146453829772,-2.35075793286181));
#56756=CARTESIAN_POINT('Ctrl Pts',(0.138479955179697,0.691576314109395,
-2.33490856256682));
#56757=CARTESIAN_POINT('Ctrl Pts',(-0.20863261025693,0.673740996348811,
-2.31905919227184));
#56758=CARTESIAN_POINT('Ctrl Pts',(-0.505079414298638,0.492289834828481,
-2.30320982197686));
#56759=CARTESIAN_POINT('Ctrl Pts',(-0.652893361036711,0.236277703536981,
-2.28972941734659));
#56760=CARTESIAN_POINT('Ctrl Pts',(-0.676628015531182,0.0619604733928406,
-2.28153213614796));
#56761=CARTESIAN_POINT('Ctrl Pts',(-0.676644996800385,-5.28592337248335E-6,
-2.278617978381));
#56762=CARTESIAN_POINT('Ctrl Pts',(-0.67664966423598,-8.77515312422764E-6,
-2.43918202161899));
#56763=CARTESIAN_POINT('Ctrl Pts',(-0.676670888840999,-0.0462624044265438,
-2.43700673906336));
#56764=CARTESIAN_POINT('Ctrl Pts',(-0.660645579160593,-0.204838031955816,
-2.42954833307605));
#56765=CARTESIAN_POINT('Ctrl Pts',(-0.538109309602317,-0.455952699979421,
-2.4168068036571));
#56766=CARTESIAN_POINT('Ctrl Pts',(-0.255006572123388,-0.657591166206698,
-2.40095743336211));
#56767=CARTESIAN_POINT('Ctrl Pts',(0.0900236949082282,-0.699535723215246,
-2.38510806306714));
#56768=CARTESIAN_POINT('Ctrl Pts',(0.413191995871872,-0.571600269634842,
-2.36925869277215));
#56769=CARTESIAN_POINT('Ctrl Pts',(0.63601794360821,-0.304853520740027,
-2.35340932247718));
#56770=CARTESIAN_POINT('Ctrl Pts',(0.704388970160089,0.0359259295776118,
-2.33755995218219));
#56771=CARTESIAN_POINT('Ctrl Pts',(0.601701390641733,0.367980882926015,
-2.32171058188722));
#56772=CARTESIAN_POINT('Ctrl Pts',(0.352892554951089,0.610672857067759,
-2.30586121159223));
#56773=CARTESIAN_POINT('Ctrl Pts',(0.0183848921922413,0.705064883140754,
-2.29001184129726));
#56774=CARTESIAN_POINT('Ctrl Pts',(-0.320587482770208,0.628234159840316,
-2.27416247100227));
#56775=CARTESIAN_POINT('Ctrl Pts',(-0.581706214008261,0.398838782321105,
-2.2583131007073));
#56776=CARTESIAN_POINT('Ctrl Pts',(-0.669880488577138,0.158819887446242,
-2.24665295091287));
#56777=CARTESIAN_POINT('Ctrl Pts',(-0.67673225418624,0.0232712070114671,
-2.2402759245501));
#56778=CARTESIAN_POINT('Ctrl Pts',(-0.676708376272384,1.704295116782E-5,
-2.23918202161899));
#56779=CARTESIAN_POINT('Origin',(0.,0.,-4.178617978381));
#56780=CARTESIAN_POINT('',(-0.676672441952873,1.56724317931045E-5,-2.678617978381));
#56781=CARTESIAN_POINT('',(-0.676756127719321,-3.58750326429069E-6,-2.639182021619));
#56782=CARTESIAN_POINT('',(-0.6767,-8.45931892044317E-14,-4.178617978381));
#56783=CARTESIAN_POINT('Ctrl Pts',(-0.676672441952873,1.56724317930956E-5,
-2.678617978381));
#56784=CARTESIAN_POINT('Ctrl Pts',(-0.676606295786303,-0.0770395337766664,
-2.67499376517447));
#56785=CARTESIAN_POINT('Ctrl Pts',(-0.644301914118974,-0.266474457412185,
-2.66608642853628));
#56786=CARTESIAN_POINT('Ctrl Pts',(-0.471028835749505,-0.52496317215227,
-2.65189596846643));
#56787=CARTESIAN_POINT('Ctrl Pts',(-0.163111735027927,-0.686184419904654,
-2.63604659817145));
#56788=CARTESIAN_POINT('Ctrl Pts',(0.184416528289274,-0.680767978328477,
-2.62019722787647));
#56789=CARTESIAN_POINT('Ctrl Pts',(0.487159828181642,-0.510029212917986,
-2.60434785758149));
#56790=CARTESIAN_POINT('Ctrl Pts',(0.671597923602639,-0.21543148617677,
-2.58849848728651));
#56791=CARTESIAN_POINT('Ctrl Pts',(0.692940613618548,0.131483087207663,
-2.57264911699153));
#56792=CARTESIAN_POINT('Ctrl Pts',(0.546004894294652,0.446467413850098,
-2.55679974669655));
#56793=CARTESIAN_POINT('Ctrl Pts',(0.266473634605688,0.653028558551418,
-2.54095037640157));
#56794=CARTESIAN_POINT('Ctrl Pts',(-0.0777698940442144,0.701003808694404,
-2.52510100610659));
#56795=CARTESIAN_POINT('Ctrl Pts',(-0.403127252931393,0.578742528390386,
-2.50925163581161));
#56796=CARTESIAN_POINT('Ctrl Pts',(-0.625491336998928,0.321822386292196,
-2.49375729323641));
#56797=CARTESIAN_POINT('Ctrl Pts',(-0.676690355084629,0.104734817936979,
-2.48354607409288));
#56798=CARTESIAN_POINT('Ctrl Pts',(-0.676750583136638,-7.6422492146077E-6,
-2.478617978381));
#56799=CARTESIAN_POINT('Ctrl Pts',(-0.67675612771932,-3.5875032643011E-6,
-2.639182021619));
#56800=CARTESIAN_POINT('Ctrl Pts',(-0.676757135496254,-0.00343274748612147,
-2.63902067700827));
#56801=CARTESIAN_POINT('Ctrl Pts',(-0.675895944019102,-0.119146993585894,
-2.63357620896589));
#56802=CARTESIAN_POINT('Ctrl Pts',(-0.614470285968358,-0.346238012588408,
-2.62284861749184));
#56803=CARTESIAN_POINT('Ctrl Pts',(-0.374495434261829,-0.597668523026142,
-2.60699924719686));
#56804=CARTESIAN_POINT('Ctrl Pts',(-0.0435755654152151,-0.703957146279481,
-2.59114987690188));
#56805=CARTESIAN_POINT('Ctrl Pts',(0.29792648997097,-0.639292030509363,
-2.5753005066069));
#56806=CARTESIAN_POINT('Ctrl Pts',(0.567078051177426,-0.419376892033906,
-2.55945113631192));
#56807=CARTESIAN_POINT('Ctrl Pts',(0.698516523342481,-0.097617418101175,
-2.54360176601694));
#56808=CARTESIAN_POINT('Ctrl Pts',(0.660322494344382,0.247848133263131,
-2.52775239572196));
#56809=CARTESIAN_POINT('Ctrl Pts',(0.461771261834565,0.533124559031865,
-2.51190302542698));
#56810=CARTESIAN_POINT('Ctrl Pts',(0.151080356900915,0.688933392613464,
-2.496053655132));
#56811=CARTESIAN_POINT('Ctrl Pts',(-0.196299928972631,0.67743695764591,
-2.48020428483702));
#56812=CARTESIAN_POINT('Ctrl Pts',(-0.496009405614011,0.501427126551448,
-2.46435491454204));
#56813=CARTESIAN_POINT('Ctrl Pts',(-0.650662304876479,0.244516783651035,
-2.4506808268027));
#56814=CARTESIAN_POINT('Ctrl Pts',(-0.67661934049947,0.066074097321367,
-2.44228986249502));
#56815=CARTESIAN_POINT('Ctrl Pts',(-0.67664966423598,-8.77515312422764E-6,
-2.43918202161899));
#56816=CARTESIAN_POINT('Origin',(0.,0.,-4.178617978381));
#56817=CARTESIAN_POINT('',(-0.67667522099595,-1.60756434531244E-5,-2.878617978381));
#56818=CARTESIAN_POINT('',(-0.676662334990091,1.3602642141286E-5,-2.839182021619));
#56819=CARTESIAN_POINT('',(-0.6767,-8.45931892044317E-14,-4.178617978381));
#56820=CARTESIAN_POINT('Ctrl Pts',(-0.67667522099595,-1.6075643453118E-5,
-2.878617978381));
#56821=CARTESIAN_POINT('Ctrl Pts',(-0.676705554749602,-0.0342520940821256,
-2.87700770311939));
#56822=CARTESIAN_POINT('Ctrl Pts',(-0.66577840727492,-0.180793269959295,
-2.87011430442611));
#56823=CARTESIAN_POINT('Ctrl Pts',(-0.56161486994617,-0.426665248267367,
-2.85793778230118));
#56824=CARTESIAN_POINT('Ctrl Pts',(-0.289645737183324,-0.643086186413016,
-2.84208841200619));
#56825=CARTESIAN_POINT('Ctrl Pts',(0.0526629354583269,-0.703335703240367,
-2.82623904171122));
#56826=CARTESIAN_POINT('Ctrl Pts',(0.382182582841647,-0.592782396496553,
-2.81038967141623));
#56827=CARTESIAN_POINT('Ctrl Pts',(0.618890413665208,-0.33827378275151,
-2.79454030112126));
#56828=CARTESIAN_POINT('Ctrl Pts',(0.705302689111543,-0.0016164639601243,
-2.77869093082627));
#56829=CARTESIAN_POINT('Ctrl Pts',(0.620434464765853,0.335433407928336,
-2.7628415605313));
#56830=CARTESIAN_POINT('Ctrl Pts',(0.384895717176935,0.591024350701866,
-2.74699219023631));
#56831=CARTESIAN_POINT('Ctrl Pts',(0.0558862770419258,0.703086922266445,
-2.73114281994134));
#56832=CARTESIAN_POINT('Ctrl Pts',(-0.286694966534403,0.644407085922823,
-2.71529344964635));
#56833=CARTESIAN_POINT('Ctrl Pts',(-0.559653255436154,0.429235052044242,
-2.69944407935137));
#56834=CARTESIAN_POINT('Ctrl Pts',(-0.665363249906537,0.182862978936254,
-2.68721892226292));
#56835=CARTESIAN_POINT('Ctrl Pts',(-0.676702719021528,0.0352861331343808,
-2.68027688860613));
#56836=CARTESIAN_POINT('Ctrl Pts',(-0.676672441952873,1.56724317930956E-5,
-2.678617978381));
#56837=CARTESIAN_POINT('Ctrl Pts',(-0.67666233499009,1.36026421412444E-5,
-2.839182021619));
#56838=CARTESIAN_POINT('Ctrl Pts',(-0.676609147890392,-0.0729267869494966,
-2.83575149152153));
#56839=CARTESIAN_POINT('Ctrl Pts',(-0.646758396857733,-0.258240144278789,
-2.8270378379924));
#56840=CARTESIAN_POINT('Ctrl Pts',(-0.48053261167355,-0.516277931755177,
-2.81304106103161));
#56841=CARTESIAN_POINT('Ctrl Pts',(-0.175609613684971,-0.683092788192513,
-2.79719169073663));
#56842=CARTESIAN_POINT('Ctrl Pts',(0.171959616715022,-0.684020748163701,
-2.78134232044165));
#56843=CARTESIAN_POINT('Ctrl Pts',(0.477769004781086,-0.518836459560908,
-2.76549295014667));
#56844=CARTESIAN_POINT('Ctrl Pts',(0.667553719770789,-0.227654397979453,
-2.74964357985169));
#56845=CARTESIAN_POINT('Ctrl Pts',(0.695225151307124,0.118812805240822,
-2.7337942095567));
#56846=CARTESIAN_POINT('Ctrl Pts',(0.55406338084068,0.436426699126669,-2.71794483926173));
#56847=CARTESIAN_POINT('Ctrl Pts',(0.278349092353365,0.648055766493336,
-2.70209546896675));
#56848=CARTESIAN_POINT('Ctrl Pts',(-0.0649613819857274,0.702306565930941,
-2.68624609867177));
#56849=CARTESIAN_POINT('Ctrl Pts',(-0.392496192704833,0.586004464497855,
-2.67039672837678));
#56850=CARTESIAN_POINT('Ctrl Pts',(-0.622350605748701,0.330025687005806,
-2.65470870269253));
#56851=CARTESIAN_POINT('Ctrl Pts',(-0.676724136501708,0.108852846529397,
-2.64430380043993));
#56852=CARTESIAN_POINT('Ctrl Pts',(-0.67675612771932,-3.5875032643011E-6,
-2.639182021619));
#56853=CARTESIAN_POINT('Origin',(0.,0.,-4.178617978381));
#56854=CARTESIAN_POINT('',(-0.676748670238398,8.58863998659695E-6,-3.078617978381));
#56855=CARTESIAN_POINT('',(-0.676687048566771,-1.71712397221968E-5,-3.039182021619));
#56856=CARTESIAN_POINT('',(-0.6767,-8.45931892044317E-14,-4.178617978381));
#56857=CARTESIAN_POINT('Ctrl Pts',(-0.676748670238398,8.58863998661613E-6,
-3.078617978381));
#56858=CARTESIAN_POINT('Ctrl Pts',(-0.676682926446315,-0.103701028300201,
-3.07373851763264));
#56859=CARTESIAN_POINT('Ctrl Pts',(-0.626265638634916,-0.319761561202685,
-3.06357593345262));
#56860=CARTESIAN_POINT('Ctrl Pts',(-0.405775812394436,-0.576888625558993,
-3.04813022584094));
#56861=CARTESIAN_POINT('Ctrl Pts',(-0.0809822831169064,-0.700639968917618,
-3.03228085554596));
#56862=CARTESIAN_POINT('Ctrl Pts',(0.263477534324128,-0.654243139154081,
-3.01643148525098));
#56863=CARTESIAN_POINT('Ctrl Pts',(0.543952676164601,-0.448965457821732,
-3.000582114956));
#56864=CARTESIAN_POINT('Ctrl Pts',(0.692330652242036,-0.134657952568069,
-2.98473274466102));
#56865=CARTESIAN_POINT('Ctrl Pts',(0.672578346146962,0.212350805314992,
-2.96888337436604));
#56866=CARTESIAN_POINT('Ctrl Pts',(0.489492542171056,0.507790850038306,
-2.95303400407106));
#56867=CARTESIAN_POINT('Ctrl Pts',(0.1875350416004,0.679915512689367,-2.93718463377608));
#56868=CARTESIAN_POINT('Ctrl Pts',(-0.159964743367749,0.686924870057126,
-2.9213352634811));
#56869=CARTESIAN_POINT('Ctrl Pts',(-0.468617602588818,0.527116722147587,
-2.90548589318612));
#56870=CARTESIAN_POINT('Ctrl Pts',(-0.643671614274052,0.26854177142875,
-2.89124679815276));
#56871=CARTESIAN_POINT('Ctrl Pts',(-0.676606033277398,0.0780722491725114,
-2.88229082655105));
#56872=CARTESIAN_POINT('Ctrl Pts',(-0.67667522099595,-1.6075643453118E-5,
-2.878617978381));
#56873=CARTESIAN_POINT('Ctrl Pts',(-0.676687048566771,-1.71712397222107E-5,
-3.039182021619));
#56874=CARTESIAN_POINT('Ctrl Pts',(-0.676716369911433,-0.0301337864271384,
-3.03776542946644));
#56875=CARTESIAN_POINT('Ctrl Pts',(-0.667382347146982,-0.172551068097945,
-3.03106571388223));
#56876=CARTESIAN_POINT('Ctrl Pts',(-0.569309303103972,-0.416342900862349,
-3.01908287486635));
#56877=CARTESIAN_POINT('Ctrl Pts',(-0.301335854323042,-0.63769208604044,
-3.00323350457137));
#56878=CARTESIAN_POINT('Ctrl Pts',(0.0398160418543145,-0.704179789904724,
-2.98738413427639));
#56879=CARTESIAN_POINT('Ctrl Pts',(0.371298739751515,-0.599659686454028,
-2.97153476398141));
#56880=CARTESIAN_POINT('Ctrl Pts',(0.612612727535191,-0.349514148155837,
-2.95568539368643));
#56881=CARTESIAN_POINT('Ctrl Pts',(0.705155675918236,-0.0144902180625897,
-2.93983602339145));
#56882=CARTESIAN_POINT('Ctrl Pts',(0.62645382619254,0.324052615091952,-2.92398665309647));
#56883=CARTESIAN_POINT('Ctrl Pts',(0.39561967057411,0.583900308232526,-2.90813728280149));
#56884=CARTESIAN_POINT('Ctrl Pts',(0.0687105446633539,0.70194968106786,
-2.89228791250651));
#56885=CARTESIAN_POINT('Ctrl Pts',(-0.274884717019473,0.649532821378821,
-2.87643854221153));
#56886=CARTESIAN_POINT('Ctrl Pts',(-0.551725105308022,0.439378995711058,
-2.86058917191655));
#56887=CARTESIAN_POINT('Ctrl Pts',(-0.663660295032008,0.191105462586324,
-2.84817033171904));
#56888=CARTESIAN_POINT('Ctrl Pts',(-0.676691057684125,0.0394036898040259,
-2.84103461495319));
#56889=CARTESIAN_POINT('Ctrl Pts',(-0.67666233499009,1.36026421412444E-5,
-2.839182021619));
#56890=CARTESIAN_POINT('Origin',(0.,0.,-4.178617978381));
#56891=CARTESIAN_POINT('',(-0.676644198931752,4.36460036937442E-6,-3.278617978381));
#56892=CARTESIAN_POINT('',(-0.676739402418013,1.19727938200573E-5,-3.23918202161899));
#56893=CARTESIAN_POINT('',(-0.6767,-8.45931892044317E-14,-4.178617978381));
#56894=CARTESIAN_POINT('Ctrl Pts',(-0.676644198931752,4.36460036935815E-6,
-3.278617978381));
#56895=CARTESIAN_POINT('Ctrl Pts',(-0.676630431341335,-0.060927441302453,
-3.27575245557756));
#56896=CARTESIAN_POINT('Ctrl Pts',(-0.653440485571609,-0.234208622315155,
-3.26760380934245));
#56897=CARTESIAN_POINT('Ctrl Pts',(-0.507330627672634,-0.489969519918335,
-3.25417203967569));
#56898=CARTESIAN_POINT('Ctrl Pts',(-0.211718659443945,-0.672777604760268,
-3.23832266938071));
#56899=CARTESIAN_POINT('Ctrl Pts',(0.135308507343731,-0.692203802405131,
-3.22247329908573));
#56900=CARTESIAN_POINT('Ctrl Pts',(0.449476436357704,-0.543530522954218,
-3.20662392879074));
#56901=CARTESIAN_POINT('Ctrl Pts',(0.65449045194897,-0.262862596295751,
-3.19077455849577));
#56902=CARTESIAN_POINT('Ctrl Pts',(0.700563556851036,0.0816406702320175,
-3.17492518820078));
#56903=CARTESIAN_POINT('Ctrl Pts',(0.576507045056651,0.406317761393417,
-3.1590758179058));
#56904=CARTESIAN_POINT('Ctrl Pts',(0.312447643247322,0.632321885160478,
-3.14322644761082));
#56905=CARTESIAN_POINT('Ctrl Pts',(-0.0274886683206437,0.704768663702968,
-3.12737707731584));
#56906=CARTESIAN_POINT('Ctrl Pts',(-0.360749444800962,0.606064628814044,
-3.11152770702087));
#56907=CARTESIAN_POINT('Ctrl Pts',(-0.606403373669456,0.360179739333031,
-3.09567833672588));
#56908=CARTESIAN_POINT('Ctrl Pts',(-0.674503132757475,0.129454074981309,
-3.08470842717926));
#56909=CARTESIAN_POINT('Ctrl Pts',(-0.676754109018807,0.00858816421545373,
-3.0790216410643));
#56910=CARTESIAN_POINT('Ctrl Pts',(-0.676748670238398,8.58863998661613E-6,
-3.078617978381));
#56911=CARTESIAN_POINT('Ctrl Pts',(-0.676739402418013,1.19727938200608E-5,
-3.23918202161899));
#56912=CARTESIAN_POINT('Ctrl Pts',(-0.676657269998734,-0.0995849951729056,
-3.23449624397969));
#56913=CARTESIAN_POINT('Ctrl Pts',(-0.629292425415603,-0.311551144554621,
-3.22452734290874));
#56914=CARTESIAN_POINT('Ctrl Pts',(-0.41623826497985,-0.56938580985635,
-3.20927531840611));
#56915=CARTESIAN_POINT('Ctrl Pts',(-0.0937577048939214,-0.699045053249238,
-3.19342594811114));
#56916=CARTESIAN_POINT('Ctrl Pts',(0.251491613629344,-0.658943443683383,
-3.17757657781615));
#56917=CARTESIAN_POINT('Ctrl Pts',(0.535666999015903,-0.458819528643346,
-3.16172720752118));
#56918=CARTESIAN_POINT('Ctrl Pts',(0.689757368805666,-0.147272760134018,
-3.1458778372262));
#56919=CARTESIAN_POINT('Ctrl Pts',(0.676342370066224,0.20003872663164,-3.13002846693121));
#56920=CARTESIAN_POINT('Ctrl Pts',(0.498679792288921,0.498771449124632,
-3.11417909663624));
#56921=CARTESIAN_POINT('Ctrl Pts',(0.199914423641749,0.676379122178673,
-3.09832972634125));
#56922=CARTESIAN_POINT('Ctrl Pts',(-0.147399522694991,0.689730291062018,
-3.08248035604627));
#56923=CARTESIAN_POINT('Ctrl Pts',(-0.458917966893342,0.535582667159503,
-3.0666309857513));
#56924=CARTESIAN_POINT('Ctrl Pts',(-0.641107555059538,0.276772949731498,
-3.05219820760887));
#56925=CARTESIAN_POINT('Ctrl Pts',(-0.67660701713636,0.0821849180722907,
-3.0430485528981));
#56926=CARTESIAN_POINT('Ctrl Pts',(-0.676687048566771,-1.71712397222107E-5,
-3.039182021619));
#56927=CARTESIAN_POINT('Origin',(0.,0.,-4.178617978381));
#56928=CARTESIAN_POINT('',(-0.676724334253827,-1.52803889846311E-5,-3.478617978381));
#56929=CARTESIAN_POINT('',(-0.676642561475797,5.96081397241655E-7,-3.439182021619));
#56930=CARTESIAN_POINT('',(-0.6767,-8.45931892044317E-14,-4.178617978381));
#56931=CARTESIAN_POINT('Ctrl Pts',(-0.676724334253826,-1.5280388984627E-5,
-3.478617978381));
#56932=CARTESIAN_POINT('Ctrl Pts',(-0.676742001449043,-0.0181170211682754,
-3.47776639352247));
#56933=CARTESIAN_POINT('Ctrl Pts',(-0.671614576287041,-0.148509662737602,
-3.47163168523228));
#56934=CARTESIAN_POINT('Ctrl Pts',(-0.590662385922995,-0.385450959342922,
-3.46021385351043));
#56935=CARTESIAN_POINT('Ctrl Pts',(-0.334850209657572,-0.620749412673154,
-3.44436448321545));
#56936=CARTESIAN_POINT('Ctrl Pts',(0.00227926788749094,-0.70530085860637,
-3.42851511292047));
#56937=CARTESIAN_POINT('Ctrl Pts',(0.338855232525197,-0.618572249312001,
-3.41266574262549));
#56938=CARTESIAN_POINT('Ctrl Pts',(0.593141288900064,-0.381625349818476,
-3.39681637233051));
#56939=CARTESIAN_POINT('Ctrl Pts',(0.703384882402956,-0.0520019560290773,
-3.38096700203553));
#56940=CARTESIAN_POINT('Ctrl Pts',(0.642813709332344,0.290249946284879,
-3.36511763174055));
#56941=CARTESIAN_POINT('Ctrl Pts',(0.426137285130135,0.562015578472108,
-3.34926826144557));
#56942=CARTESIAN_POINT('Ctrl Pts',(0.105974785652812,0.697297526906368,
-3.33341889115059));
#56943=CARTESIAN_POINT('Ctrl Pts',(-0.239923351207117,0.663243003558396,
-3.31756952085561));
#56944=CARTESIAN_POINT('Ctrl Pts',(-0.527556870419987,0.468122040387345,
-3.30172015056063));
#56945=CARTESIAN_POINT('Ctrl Pts',(-0.658234470612573,0.215149858671953,
-3.28873630306909));
#56946=CARTESIAN_POINT('Ctrl Pts',(-0.676655814450987,0.0514116582543703,
-3.28103557900922));
#56947=CARTESIAN_POINT('Ctrl Pts',(-0.676644198931752,4.36460036935815E-6,
-3.278617978381));
#56948=CARTESIAN_POINT('Ctrl Pts',(-0.676642561475797,5.96081397224307E-7,
-3.439182021619));
#56949=CARTESIAN_POINT('Ctrl Pts',(-0.67664081343884,-0.056813170325692,
-3.43651018192461));
#56950=CARTESIAN_POINT('Ctrl Pts',(-0.655567470475998,-0.225968086496106,
-3.42855521879857));
#56951=CARTESIAN_POINT('Ctrl Pts',(-0.51618960975049,-0.480627486193364,
-3.41531713224086));
#56952=CARTESIAN_POINT('Ctrl Pts',(-0.223963722768737,-0.6688009753155,
-3.39946776194589));
#56953=CARTESIAN_POINT('Ctrl Pts',(0.122651037193902,-0.694558288968156,
-3.3836183916509));
#56954=CARTESIAN_POINT('Ctrl Pts',(0.43948038548163,-0.551644346002168,
-3.36776902135592));
#56955=CARTESIAN_POINT('Ctrl Pts',(0.649583329296276,-0.274765339880352,
-3.35191965106094));
#56956=CARTESIAN_POINT('Ctrl Pts',(0.701937041446152,0.0688395492796521,
-3.33607028076596));
#56957=CARTESIAN_POINT('Ctrl Pts',(0.583827590563321,0.39572697430961,-3.32022091047098));
#56958=CARTESIAN_POINT('Ctrl Pts',(0.323937478628386,0.626513370678621,
-3.304371540176));
#56959=CARTESIAN_POINT('Ctrl Pts',(-0.0146198127989899,0.705153000967117,
-3.28852216988102));
#56960=CARTESIAN_POINT('Ctrl Pts',(-0.349626729498273,0.612548482750179,
-3.27267279958604));
#56961=CARTESIAN_POINT('Ctrl Pts',(-0.599727914383955,0.371188526772956,
-3.25682342929106));
#56962=CARTESIAN_POINT('Ctrl Pts',(-0.673304323117296,0.137693307660308,
-3.24565983663537));
#56963=CARTESIAN_POINT('Ctrl Pts',(-0.676749872708934,0.0127086550366688,
-3.23977936741135));
#56964=CARTESIAN_POINT('Ctrl Pts',(-0.676739402418013,1.19727938200608E-5,
-3.23918202161899));
#56965=CARTESIAN_POINT('Origin',(0.,0.,-4.178617978381));
#56966=CARTESIAN_POINT('',(-0.676703788167417,1.73951649274827E-5,-3.678617978381));
#56967=CARTESIAN_POINT('',(-0.67673605652177,-1.28860430050337E-5,-3.639182021619));
#56968=CARTESIAN_POINT('',(-0.6767,-8.45931892044317E-14,-4.178617978381));
#56969=CARTESIAN_POINT('Ctrl Pts',(-0.676703788167417,1.73951649275021E-5,
-3.678617978381));
#56970=CARTESIAN_POINT('Ctrl Pts',(-0.676613881463619,-0.0875835708292743,
-3.67449720803573));
#56971=CARTESIAN_POINT('Ctrl Pts',(-0.637609911674448,-0.287573235928348,
-3.66509331425879));
#56972=CARTESIAN_POINT('Ctrl Pts',(-0.445954115113484,-0.546424125806921,
-3.6504062970502));
#56973=CARTESIAN_POINT('Ctrl Pts',(-0.130831839792564,-0.693063915639031,
-3.63455692675522));
#56974=CARTESIAN_POINT('Ctrl Pts',(0.21606252083174,-0.671395152184437,
-3.61870755646024));
#56975=CARTESIAN_POINT('Ctrl Pts',(0.510486794197391,-0.48668032805703,
-3.60285818616526));
#56976=CARTESIAN_POINT('Ctrl Pts',(0.680940981975007,-0.183776692274722,
-3.58700881587028));
#56977=CARTESIAN_POINT('Ctrl Pts',(0.686030833613329,0.163756498125624,
-3.5711594455753));
#56978=CARTESIAN_POINT('Ctrl Pts',(0.524520293312469,0.471521960898263,
-3.55531007528032));
#56979=CARTESIAN_POINT('Ctrl Pts',(0.235631679485712,0.664779818244593,
-3.53946070498533));
#56980=CARTESIAN_POINT('Ctrl Pts',(-0.110479333395072,0.696598028792635,
-3.52361133469035));
#56981=CARTESIAN_POINT('Ctrl Pts',(-0.429760793823647,0.55924963662321,
-3.50776196439537));
#56982=CARTESIAN_POINT('Ctrl Pts',(-0.633128840107847,0.30076613753894,
-3.49276417895892));
#56983=CARTESIAN_POINT('Ctrl Pts',(-0.676632396431899,0.0941838610127268,
-3.48304951695413));
#56984=CARTESIAN_POINT('Ctrl Pts',(-0.676724334253826,-1.5280388984627E-5,
-3.478617978381));
#56985=CARTESIAN_POINT('Ctrl Pts',(-0.67673605652177,-1.28860430050285E-5,
-3.639182021619));
#56986=CARTESIAN_POINT('Ctrl Pts',(-0.676748229532135,-0.0139968950353071,
-3.63852411986953));
#56987=CARTESIAN_POINT('Ctrl Pts',(-0.672913840421779,-0.140269491848012,
-3.6325830946884));
#56988=CARTESIAN_POINT('Ctrl Pts',(-0.597599687597092,-0.374605270350371,
-3.62135894607561));
#56989=CARTESIAN_POINT('Ctrl Pts',(-0.346125077999637,-0.614533907095192,
-3.60550957578063));
#56990=CARTESIAN_POINT('Ctrl Pts',(-0.0105951019105329,-0.705224955685239,
-3.58966020548565));
#56991=CARTESIAN_POINT('Ctrl Pts',(0.32750786099247,-0.624654379983339,
-3.57381083519067));
#56992=CARTESIAN_POINT('Ctrl Pts',(0.586076588355783,-0.392388489065435,
-3.55796146489568));
#56993=CARTESIAN_POINT('Ctrl Pts',(0.702318492816257,-0.0648323094657422,
-3.54211209460071));
#56994=CARTESIAN_POINT('Ctrl Pts',(0.648004599968331,0.278468188664054,
-3.52626272430573));
#56995=CARTESIAN_POINT('Ctrl Pts',(0.436324864834359,0.55414357890779,-3.51041335401075));
#56996=CARTESIAN_POINT('Ctrl Pts',(0.118685033304739,0.695246975223788,
-3.49456398371577));
#56997=CARTESIAN_POINT('Ctrl Pts',(-0.227777078549499,0.667511869700924,
-3.47871461342078));
#56998=CARTESIAN_POINT('Ctrl Pts',(-0.518924256183446,0.477673643863711,
-3.46286524312581));
#56999=CARTESIAN_POINT('Ctrl Pts',(-0.65621553862413,0.223391456722108,
-3.44968771252521));
#57000=CARTESIAN_POINT('Ctrl Pts',(-0.67664426989434,0.0555267058940655,
-3.44179330535627));
#57001=CARTESIAN_POINT('Ctrl Pts',(-0.676642561475797,5.96081397224307E-7,
-3.439182021619));
#57002=CARTESIAN_POINT('Origin',(1.87869726832665E-16,-4.25270154953079E-17,
-0.0711000000000002));
#57003=CARTESIAN_POINT('',(0.533647856309012,-0.584002718706682,-0.0711000000000004));
#57004=CARTESIAN_POINT('Ctrl Pts',(-0.657933019064465,-0.158364055658306,
-0.0711000000000003));
#57005=CARTESIAN_POINT('Ctrl Pts',(-0.65503062620215,-0.177074058470794,
-0.0711000000000003));
#57006=CARTESIAN_POINT('Ctrl Pts',(-0.651342440307925,-0.195634100037483,
-0.0710999999999999));
#57007=CARTESIAN_POINT('Ctrl Pts',(-0.646874620641261,-0.213993464998097,
-0.0710999999999998));
#57008=CARTESIAN_POINT('Ctrl Pts',(-0.640039981846469,-0.242078669274306,
-0.0710999999999997));
#57009=CARTESIAN_POINT('Ctrl Pts',(-0.631382480356379,-0.269694614707558,
-0.0711));
#57010=CARTESIAN_POINT('Ctrl Pts',(-0.62100840580272,-0.296696933525342,
-0.0710999999999998));
#57011=CARTESIAN_POINT('Ctrl Pts',(-0.616895281241109,-0.307402842777815,
-0.0710999999999997));
#57012=CARTESIAN_POINT('Ctrl Pts',(-0.612511970360756,-0.318012260843023,
-0.0710999999999991));
#57013=CARTESIAN_POINT('Ctrl Pts',(-0.607863785080036,-0.328515943120043,
-0.0710999999999991));
#57014=CARTESIAN_POINT('Ctrl Pts',(-0.604119622512866,-0.336976770652498,
-0.0710999999999991));
#57015=CARTESIAN_POINT('Ctrl Pts',(-0.600206902465123,-0.34536129242641,
-0.0710999999999998));
#57016=CARTESIAN_POINT('Ctrl Pts',(-0.596131845457498,-0.353659680525224,
-0.0710999999999997));
#57017=CARTESIAN_POINT('Ctrl Pts',(-0.581559334527423,-0.38333493440406,
-0.0710999999999993));
#57018=CARTESIAN_POINT('Ctrl Pts',(-0.56490503752703,-0.411931064563356,
-0.0710999999999997));
#57019=CARTESIAN_POINT('Ctrl Pts',(-0.546315461068867,-0.439236112401077,
-0.071099999999999));
#57020=CARTESIAN_POINT('Ctrl Pts',(-0.53873175404231,-0.450375337848918,
-0.0710999999999987));
#57021=CARTESIAN_POINT('Ctrl Pts',(-0.530825419406411,-0.461299557966116,
-0.0710999999999999));
#57022=CARTESIAN_POINT('Ctrl Pts',(-0.522604263717814,-0.471993563819338,
-0.0710999999999997));
#57023=CARTESIAN_POINT('Ctrl Pts',(-0.51522815102627,-0.481588345293528,
-0.0710999999999996));
#57024=CARTESIAN_POINT('Ctrl Pts',(-0.507593820692343,-0.491002935074771,
-0.0710999999999987));
#57025=CARTESIAN_POINT('Ctrl Pts',(-0.499731411497607,-0.500197640924792,
-0.0710999999999989));
#57026=CARTESIAN_POINT('Ctrl Pts',(-0.494876261095983,-0.505875503612279,
-0.071099999999999));
#57027=CARTESIAN_POINT('Ctrl Pts',(-0.489932967483916,-0.511471246370217,
-0.0710999999999986));
#57028=CARTESIAN_POINT('Ctrl Pts',(-0.484903330545617,-0.516982602993148,
-0.0710999999999987));
#57029=CARTESIAN_POINT('Ctrl Pts',(-0.461971240369799,-0.542111042405098,
-0.0710999999999992));
#57030=CARTESIAN_POINT('Ctrl Pts',(-0.437248134919206,-0.56548729539326,
-0.0710999999999999));
#57031=CARTESIAN_POINT('Ctrl Pts',(-0.410992239190816,-0.587010422199328,
-0.0711));
#57032=CARTESIAN_POINT('Ctrl Pts',(-0.39326243857021,-0.601544329210201,
-0.0711000000000001));
#57033=CARTESIAN_POINT('Ctrl Pts',(-0.374832581857655,-0.615232798615158,
-0.0711));
#57034=CARTESIAN_POINT('Ctrl Pts',(-0.35577134099474,-0.628036837492105,
-0.0711000000000001));
#57035=CARTESIAN_POINT('Ctrl Pts',(-0.341140666782019,-0.637864724499193,
-0.0711000000000001));
#57036=CARTESIAN_POINT('Ctrl Pts',(-0.326137824756979,-0.647171429838753,
-0.0711000000000004));
#57037=CARTESIAN_POINT('Ctrl Pts',(-0.310791231743006,-0.655936080266888,
-0.0711000000000005));
#57038=CARTESIAN_POINT('Ctrl Pts',(-0.302074038217026,-0.66091458943176,
-0.0711000000000006));
#57039=CARTESIAN_POINT('Ctrl Pts',(-0.293241255994626,-0.665720310855507,
-0.0711000000000007));
#57040=CARTESIAN_POINT('Ctrl Pts',(-0.284325627455792,-0.670335295097501,
-0.0711000000000006));
#57041=CARTESIAN_POINT('Ctrl Pts',(-0.252583677741976,-0.686765835816121,
-0.0711000000000003));
#57042=CARTESIAN_POINT('Ctrl Pts',(-0.219739495999929,-0.700816273313726,
-0.0710999999999988));
#57043=CARTESIAN_POINT('Ctrl Pts',(-0.186058445098527,-0.712362050184812,
-0.0710999999999991));
#57044=CARTESIAN_POINT('Ctrl Pts',(-0.156596236519901,-0.722461618852489,
-0.0710999999999993));
#57045=CARTESIAN_POINT('Ctrl Pts',(-0.126492499041445,-0.730644623003689,
-0.0711000000000014));
#57046=CARTESIAN_POINT('Ctrl Pts',(-0.0959372766721807,-0.736918016760253,
-0.0711000000000021));
#57047=CARTESIAN_POINT('Ctrl Pts',(-0.0782625200973073,-0.74054687948642,
-0.0711000000000024));
#57048=CARTESIAN_POINT('Ctrl Pts',(-0.060436391626456,-0.743536212012475,
-0.0711000000000009));
#57049=CARTESIAN_POINT('Ctrl Pts',(-0.0424941216358214,-0.745882575461859,
-0.0711000000000012));
#57050=CARTESIAN_POINT('Ctrl Pts',(-0.0318388515518829,-0.747275996488369,
-0.0711000000000013));
#57051=CARTESIAN_POINT('Ctrl Pts',(-0.0211364537413023,-0.748442901172957,
-0.0711000000000007));
#57052=CARTESIAN_POINT('Ctrl Pts',(-0.0104285730074772,-0.749379640043616,
-0.0711000000000007));
#57053=CARTESIAN_POINT('Ctrl Pts',(0.025356570627025,-0.752510169404919,
-0.0711000000000008));
#57054=CARTESIAN_POINT('Ctrl Pts',(0.0612586008151781,-0.753084251111668,
-0.0711000000000002));
#57055=CARTESIAN_POINT('Ctrl Pts',(0.0969927642975169,-0.751127525158457,
-0.0711000000000003));
#57056=CARTESIAN_POINT('Ctrl Pts',(0.125940091500207,-0.749542431766203,
-0.0711000000000004));
#57057=CARTESIAN_POINT('Ctrl Pts',(0.154778109260746,-0.746295712572856,
-0.0711000000000011));
#57058=CARTESIAN_POINT('Ctrl Pts',(0.183361235835868,-0.741376633595651,
-0.0711000000000012));
#57059=CARTESIAN_POINT('Ctrl Pts',(0.199996157954703,-0.738513808373675,
-0.0711000000000013));
#57060=CARTESIAN_POINT('Ctrl Pts',(0.216544799385339,-0.735084126475059,
-0.0711000000000006));
#57061=CARTESIAN_POINT('Ctrl Pts',(0.232983116072828,-0.731099822944309,
-0.0711000000000004));
#57062=CARTESIAN_POINT('Ctrl Pts',(0.241901902693802,-0.728938095943941,
-0.0711000000000003));
#57063=CARTESIAN_POINT('Ctrl Pts',(0.250788206317074,-0.726613058778705,
-0.0711000000000002));
#57064=CARTESIAN_POINT('Ctrl Pts',(0.259638114598271,-0.724126353932503,
-0.0711000000000001));
#57065=CARTESIAN_POINT('Ctrl Pts',(0.26675216273337,-0.722127402371474,
-0.0711));
#57066=CARTESIAN_POINT('Ctrl Pts',(0.273841886282841,-0.72002407427316,
-0.0711000000000008));
#57067=CARTESIAN_POINT('Ctrl Pts',(0.280892730142186,-0.717821495687171,
-0.0711000000000007));
#57068=CARTESIAN_POINT('Ctrl Pts',(0.315569759821888,-0.70698890819525,
-0.0711000000000003));
#57069=CARTESIAN_POINT('Ctrl Pts',(0.349386649818376,-0.693738011373514,
-0.0711000000000011));
#57070=CARTESIAN_POINT('Ctrl Pts',(0.382115560216981,-0.678233698777178,
-0.0711000000000009));
#57071=CARTESIAN_POINT('Ctrl Pts',(0.415111724192097,-0.662602783035725,
-0.0711000000000007));
#57072=CARTESIAN_POINT('Ctrl Pts',(0.447003233551593,-0.644681145485417,
-0.0711000000000005));
#57073=CARTESIAN_POINT('Ctrl Pts',(0.477547339957608,-0.624586406195176,
-0.0711000000000002));
#57074=CARTESIAN_POINT('Ctrl Pts',(0.496805372995163,-0.611916690211726,
-0.0711));
#57075=CARTESIAN_POINT('Ctrl Pts',(0.515527533576182,-0.598382096416591,
-0.0711000000000005));
#57076=CARTESIAN_POINT('Ctrl Pts',(0.533647856309012,-0.584002718706682,
-0.0711000000000004));
#57077=CARTESIAN_POINT('',(-0.7911,-9.68818082805471E-17,-0.0711000000000002));
#57078=CARTESIAN_POINT('Origin',(0.,0.,-0.0711000000000002));
#57079=CARTESIAN_POINT('',(0.789513386643969,0.0505148782186592,-0.0710999999999996));
#57080=CARTESIAN_POINT('Origin',(0.,0.,-0.0711000000000002));
#57081=CARTESIAN_POINT('Ctrl Pts',(0.78951338664397,0.0505148782186367,
-0.0711000000000005));
#57082=CARTESIAN_POINT('Ctrl Pts',(0.78661052546768,0.0722981214340736,
-0.0711000000000005));
#57083=CARTESIAN_POINT('Ctrl Pts',(0.782799122054415,0.093925916286846,
-0.0711000000000009));
#57084=CARTESIAN_POINT('Ctrl Pts',(0.778073401536598,0.115341501127996,
-0.0711000000000008));
#57085=CARTESIAN_POINT('Ctrl Pts',(0.771149681304201,0.146717778564259,
-0.0711000000000006));
#57086=CARTESIAN_POINT('Ctrl Pts',(0.762264400925658,0.177639384255821,
-0.0711000000000003));
#57087=CARTESIAN_POINT('Ctrl Pts',(0.751493831504571,0.20793557337634,-0.0711000000000002));
#57088=CARTESIAN_POINT('Ctrl Pts',(0.747066427308488,0.220389276573766,
-0.0711000000000002));
#57089=CARTESIAN_POINT('Ctrl Pts',(0.742320147977868,0.23273712772702,-0.0711000000000011));
#57090=CARTESIAN_POINT('Ctrl Pts',(0.737259077679951,0.244966403627896,
-0.0711000000000011));
#57091=CARTESIAN_POINT('Ctrl Pts',(0.733765772645089,0.253407422733052,
-0.0711000000000011));
#57092=CARTESIAN_POINT('Ctrl Pts',(0.730123916425295,0.261788183558137,
-0.0711000000000004));
#57093=CARTESIAN_POINT('Ctrl Pts',(0.726339264530682,0.270096071681808,
-0.0711000000000004));
#57094=CARTESIAN_POINT('Ctrl Pts',(0.710964767292107,0.303845437957103,
-0.0711000000000003));
#57095=CARTESIAN_POINT('Ctrl Pts',(0.693219611127889,0.336438260657923,
-0.0711000000000011));
#57096=CARTESIAN_POINT('Ctrl Pts',(0.673216664367045,0.36760422296276,-0.0711000000000007));
#57097=CARTESIAN_POINT('Ctrl Pts',(0.660742576029565,0.387039707722144,
-0.0711000000000005));
#57098=CARTESIAN_POINT('Ctrl Pts',(0.647389499046721,0.405919707003685,
-0.0711000000000008));
#57099=CARTESIAN_POINT('Ctrl Pts',(0.633176849541804,0.424170344891628,
-0.0711000000000008));
#57100=CARTESIAN_POINT('Ctrl Pts',(0.628311904428941,0.430417480696169,
-0.0711000000000008));
#57101=CARTESIAN_POINT('Ctrl Pts',(0.623352327566985,0.436582931045207,
-0.0711000000000015));
#57102=CARTESIAN_POINT('Ctrl Pts',(0.618299802221877,0.442663774988552,
-0.0711000000000014));
#57103=CARTESIAN_POINT('Ctrl Pts',(0.614443389962302,0.447305066131087,
-0.0711000000000014));
#57104=CARTESIAN_POINT('Ctrl Pts',(0.610532753409042,0.451897160166506,
-0.0711000000000004));
#57105=CARTESIAN_POINT('Ctrl Pts',(0.606568433677576,0.456438943152013,
-0.0711000000000004));
#57106=CARTESIAN_POINT('Ctrl Pts',(0.58313660419168,0.483283973746704,-0.0711000000000006));
#57107=CARTESIAN_POINT('Ctrl Pts',(0.557832078686923,0.508374602396631,
-0.0711000000000008));
#57108=CARTESIAN_POINT('Ctrl Pts',(0.530883792611114,0.531563679938661,
-0.0711000000000007));
#57109=CARTESIAN_POINT('Ctrl Pts',(0.504174176005348,0.554547381716453,
-0.0711000000000006));
#57110=CARTESIAN_POINT('Ctrl Pts',(0.475848664779934,0.575663628147837,
-0.0711000000000008));
#57111=CARTESIAN_POINT('Ctrl Pts',(0.446106434425362,0.594724507602636,
-0.071100000000001));
#57112=CARTESIAN_POINT('Ctrl Pts',(0.435751912723322,0.601360401670492,
-0.071100000000001));
#57113=CARTESIAN_POINT('Ctrl Pts',(0.425225545807383,0.607746741139793,
-0.0711000000000012));
#57114=CARTESIAN_POINT('Ctrl Pts',(0.414535431121882,0.613874117881312,
-0.0711000000000012));
#57115=CARTESIAN_POINT('Ctrl Pts',(0.408223415711616,0.617492048797379,
-0.0711000000000012));
#57116=CARTESIAN_POINT('Ctrl Pts',(0.401862277040809,0.621015092498111,
-0.0711000000000001));
#57117=CARTESIAN_POINT('Ctrl Pts',(0.395455743413018,0.624441054785095,
-0.0711000000000001));
#57118=CARTESIAN_POINT('Ctrl Pts',(0.365742774357445,0.640330382357987,
-0.0711));
#57119=CARTESIAN_POINT('Ctrl Pts',(0.3350422875416,0.654141967795412,-0.0711000000000001));
#57120=CARTESIAN_POINT('Ctrl Pts',(0.303539059002828,0.665732433051718,
-0.0710999999999999));
#57121=CARTESIAN_POINT('Ctrl Pts',(0.275530358755668,0.676037213931223,
-0.0710999999999998));
#57122=CARTESIAN_POINT('Ctrl Pts',(0.246886289233648,0.684585758484945,
-0.0710999999999995));
#57123=CARTESIAN_POINT('Ctrl Pts',(0.217777992627247,0.691347378539147,
-0.0710999999999995));
#57124=CARTESIAN_POINT('Ctrl Pts',(0.202137684730114,0.694980494587163,
-0.0710999999999995));
#57125=CARTESIAN_POINT('Ctrl Pts',(0.186363322806913,0.698097230410341,
-0.0710999999999994));
#57126=CARTESIAN_POINT('Ctrl Pts',(0.170481817352287,0.700689439048332,
-0.0710999999999994));
#57127=CARTESIAN_POINT('Ctrl Pts',(0.163380351267642,0.701848553452165,
-0.0710999999999993));
#57128=CARTESIAN_POINT('Ctrl Pts',(0.156257469551547,0.702902759038939,
-0.0710999999999998));
#57129=CARTESIAN_POINT('Ctrl Pts',(0.149115623612038,0.703851173059788,
-0.0710999999999999));
#57130=CARTESIAN_POINT('Ctrl Pts',(0.141353010569289,0.704882022942371,
-0.0710999999999999));
#57131=CARTESIAN_POINT('Ctrl Pts',(0.13357626627858,0.705786728185342,-0.0711000000000005));
#57132=CARTESIAN_POINT('Ctrl Pts',(0.12579468693895,0.706564431715505,-0.0711000000000005));
#57133=CARTESIAN_POINT('Ctrl Pts',(0.0920135096877081,0.709940576795407,
-0.0711000000000001));
#57134=CARTESIAN_POINT('Ctrl Pts',(0.058104255206695,0.710932267880054,
-0.0710999999999991));
#57135=CARTESIAN_POINT('Ctrl Pts',(0.0243216192917772,0.709505711937895,
-0.0710999999999992));
#57136=CARTESIAN_POINT('Ctrl Pts',(-0.000340213743341033,0.708464304614045,
-0.0710999999999992));
#57137=CARTESIAN_POINT('Ctrl Pts',(-0.0249347689083127,0.706133099639931,
-0.0711000000000011));
#57138=CARTESIAN_POINT('Ctrl Pts',(-0.0493592836677601,0.702481730021055,
-0.0711000000000013));
#57139=CARTESIAN_POINT('Ctrl Pts',(-0.0651808582794006,0.700116466373908,
-0.0711000000000014));
#57140=CARTESIAN_POINT('Ctrl Pts',(-0.0809309971795266,0.697196915910823,
-0.0710999999999999));
#57141=CARTESIAN_POINT('Ctrl Pts',(-0.0965819268706004,0.693730207786549,
-0.0710999999999999));
#57142=CARTESIAN_POINT('Ctrl Pts',(-0.104866815817021,0.691895090487693,
-0.0710999999999998));
#57143=CARTESIAN_POINT('Ctrl Pts',(-0.113123881048993,0.689906614697153,
-0.0711000000000002));
#57144=CARTESIAN_POINT('Ctrl Pts',(-0.121348819670347,0.687765605816627,
-0.0711000000000001));
#57145=CARTESIAN_POINT('Ctrl Pts',(-0.127458595159029,0.686175188649826,
-0.0711000000000001));
#57146=CARTESIAN_POINT('Ctrl Pts',(-0.133548886198576,0.684500970614239,
-0.0711000000000011));
#57147=CARTESIAN_POINT('Ctrl Pts',(-0.139609180249646,0.682746165691243,
-0.071100000000001));
#57148=CARTESIAN_POINT('Ctrl Pts',(-0.171636625378093,0.673472371728645,
-0.0711000000000007));
#57149=CARTESIAN_POINT('Ctrl Pts',(-0.202898352839185,0.661933786898764,
-0.0711000000000011));
#57150=CARTESIAN_POINT('Ctrl Pts',(-0.233159168168239,0.648235814607184,
-0.071100000000001));
#57151=CARTESIAN_POINT('Ctrl Pts',(-0.262858401786809,0.634792049964209,
-0.071100000000001));
#57152=CARTESIAN_POINT('Ctrl Pts',(-0.291594498854259,0.619267592208833,
-0.0711000000000003));
#57153=CARTESIAN_POINT('Ctrl Pts',(-0.319116683345441,0.601722036612944,
-0.0711000000000002));
#57154=CARTESIAN_POINT('Ctrl Pts',(-0.334495563251145,0.591917909601351,
-0.0711000000000001));
#57155=CARTESIAN_POINT('Ctrl Pts',(-0.349494822078873,0.58148206204072,
-0.0711000000000004));
#57156=CARTESIAN_POINT('Ctrl Pts',(-0.364065050236245,0.570420484551949,
-0.0711000000000004));
#57157=CARTESIAN_POINT('Ctrl Pts',(-0.292601934307099,0.610169646934149,
-3.87494887079529));
#57158=CARTESIAN_POINT('Ctrl Pts',(-0.393874364065824,0.561605269816615,
-3.86966574736363));
#57159=CARTESIAN_POINT('Ctrl Pts',(-0.57167140911708,0.413129829644052,
-3.85909950050031));
#57160=CARTESIAN_POINT('Ctrl Pts',(-0.699554853645959,0.0898747877851167,
-3.84325013020534));
#57161=CARTESIAN_POINT('Ctrl Pts',(-0.657542948589637,-0.255117175027513,
-3.82740075991035));
#57162=CARTESIAN_POINT('Ctrl Pts',(-0.455854483614461,-0.538198316628701,
-3.81155138961538));
#57163=CARTESIAN_POINT('Ctrl Pts',(-0.143460319648273,-0.690557636244561,
-3.79570201932039));
#57164=CARTESIAN_POINT('Ctrl Pts',(0.203771242261294,-0.675228509254,-3.77985264902541));
#57165=CARTESIAN_POINT('Ctrl Pts',(0.501518367203066,-0.495916548685635,
-3.76400327873043));
#57166=CARTESIAN_POINT('Ctrl Pts',(0.677472975891979,-0.19617577998387,
-3.74815390843546));
#57167=CARTESIAN_POINT('Ctrl Pts',(0.688905638980991,0.15120714934306,-3.73230453814047));
#57168=CARTESIAN_POINT('Ctrl Pts',(0.533039672552928,0.46186914013689,-3.71645516784549));
#57169=CARTESIAN_POINT('Ctrl Pts',(0.24772677985824,0.66036808055943,-3.70060579755051));
#57170=CARTESIAN_POINT('Ctrl Pts',(-0.097745794456612,0.698498547043651,
-3.68475642725553));
#57171=CARTESIAN_POINT('Ctrl Pts',(-0.419481102114336,0.567000979985795,
-3.66890705696055));
#57172=CARTESIAN_POINT('Ctrl Pts',(-0.639346774094541,0.297808988211044,
-3.65305768666557));
#57173=CARTESIAN_POINT('Ctrl Pts',(-0.703949125559012,-0.0437049361714047,
-3.63720831637059));
#57174=CARTESIAN_POINT('Ctrl Pts',(-0.597599687597092,-0.374605270350371,
-3.62135894607561));
#57175=CARTESIAN_POINT('Ctrl Pts',(-0.346125077999637,-0.614533907095192,
-3.60550957578063));
#57176=CARTESIAN_POINT('Ctrl Pts',(-0.0105951019105329,-0.705224955685239,
-3.58966020548565));
#57177=CARTESIAN_POINT('Ctrl Pts',(0.32750786099247,-0.624654379983339,
-3.57381083519067));
#57178=CARTESIAN_POINT('Ctrl Pts',(0.586076588355783,-0.392388489065435,
-3.55796146489568));
#57179=CARTESIAN_POINT('Ctrl Pts',(0.702318492816257,-0.0648323094657422,
-3.54211209460071));
#57180=CARTESIAN_POINT('Ctrl Pts',(0.648004599968331,0.278468188664054,
-3.52626272430573));
#57181=CARTESIAN_POINT('Ctrl Pts',(0.436324864834359,0.55414357890779,-3.51041335401075));
#57182=CARTESIAN_POINT('Ctrl Pts',(0.118685033304739,0.695246975223788,
-3.49456398371577));
#57183=CARTESIAN_POINT('Ctrl Pts',(-0.227777078549499,0.667511869700924,
-3.47871461342078));
#57184=CARTESIAN_POINT('Ctrl Pts',(-0.518924256183446,0.477673643863711,
-3.46286524312581));
#57185=CARTESIAN_POINT('Ctrl Pts',(-0.684052339708951,0.171833903051996,
-3.44701587283082));
#57186=CARTESIAN_POINT('Ctrl Pts',(-0.683060502755426,-0.175735150937388,
-3.43116650253584));
#57187=CARTESIAN_POINT('Ctrl Pts',(-0.51618960975049,-0.480627486193364,
-3.41531713224086));
#57188=CARTESIAN_POINT('Ctrl Pts',(-0.223963722768737,-0.6688009753155,
-3.39946776194589));
#57189=CARTESIAN_POINT('Ctrl Pts',(0.122651037193902,-0.694558288968156,
-3.3836183916509));
#57190=CARTESIAN_POINT('Ctrl Pts',(0.43948038548163,-0.551644346002168,
-3.36776902135592));
#57191=CARTESIAN_POINT('Ctrl Pts',(0.649583329296276,-0.274765339880352,
-3.35191965106094));
#57192=CARTESIAN_POINT('Ctrl Pts',(0.701937041446152,0.0688395492796521,
-3.33607028076596));
#57193=CARTESIAN_POINT('Ctrl Pts',(0.583827590563321,0.39572697430961,-3.32022091047098));
#57194=CARTESIAN_POINT('Ctrl Pts',(0.323937478628386,0.626513370678621,
-3.304371540176));
#57195=CARTESIAN_POINT('Ctrl Pts',(-0.0146198127989899,0.705153000967117,
-3.28852216988102));
#57196=CARTESIAN_POINT('Ctrl Pts',(-0.349626729498273,0.612548482750179,
-3.27267279958604));
#57197=CARTESIAN_POINT('Ctrl Pts',(-0.599727914383955,0.371188526772956,
-3.25682342929106));
#57198=CARTESIAN_POINT('Ctrl Pts',(-0.704187095487817,0.0396866255511638,
-3.24097405899607));
#57199=CARTESIAN_POINT('Ctrl Pts',(-0.637636695139234,-0.301453045615932,
-3.22512468870111));
#57200=CARTESIAN_POINT('Ctrl Pts',(-0.41623826497985,-0.56938580985635,
-3.20927531840611));
#57201=CARTESIAN_POINT('Ctrl Pts',(-0.0937577048939214,-0.699045053249238,
-3.19342594811114));
#57202=CARTESIAN_POINT('Ctrl Pts',(0.251491613629344,-0.658943443683383,
-3.17757657781615));
#57203=CARTESIAN_POINT('Ctrl Pts',(0.535666999015903,-0.458819528643346,
-3.16172720752118));
#57204=CARTESIAN_POINT('Ctrl Pts',(0.689757368805666,-0.147272760134018,
-3.1458778372262));
#57205=CARTESIAN_POINT('Ctrl Pts',(0.676342370066224,0.20003872663164,-3.13002846693121));
#57206=CARTESIAN_POINT('Ctrl Pts',(0.498679792288921,0.498771449124632,
-3.11417909663624));
#57207=CARTESIAN_POINT('Ctrl Pts',(0.199914423641749,0.676379122178673,
-3.09832972634125));
#57208=CARTESIAN_POINT('Ctrl Pts',(-0.147399522694991,0.689730291062018,
-3.08248035604627));
#57209=CARTESIAN_POINT('Ctrl Pts',(-0.458917966893342,0.535582667159503,
-3.0666309857513));
#57210=CARTESIAN_POINT('Ctrl Pts',(-0.658989652208569,0.251370507381504,
-3.05078161545631));
#57211=CARTESIAN_POINT('Ctrl Pts',(-0.699027810457228,-0.093886175268675,
-3.03493224516134));
#57212=CARTESIAN_POINT('Ctrl Pts',(-0.569309303103972,-0.416342900862349,
-3.01908287486635));
#57213=CARTESIAN_POINT('Ctrl Pts',(-0.301335854323042,-0.63769208604044,
-3.00323350457137));
#57214=CARTESIAN_POINT('Ctrl Pts',(0.0398160418543145,-0.704179789904724,
-2.98738413427639));
#57215=CARTESIAN_POINT('Ctrl Pts',(0.371298739751515,-0.599659686454028,
-2.97153476398141));
#57216=CARTESIAN_POINT('Ctrl Pts',(0.612612727535191,-0.349514148155837,
-2.95568539368643));
#57217=CARTESIAN_POINT('Ctrl Pts',(0.705155675918236,-0.0144902180625897,
-2.93983602339145));
#57218=CARTESIAN_POINT('Ctrl Pts',(0.62645382619254,0.324052615091952,-2.92398665309647));
#57219=CARTESIAN_POINT('Ctrl Pts',(0.39561967057411,0.583900308232526,-2.90813728280149));
#57220=CARTESIAN_POINT('Ctrl Pts',(0.0687105446633539,0.70194968106786,
-2.89228791250651));
#57221=CARTESIAN_POINT('Ctrl Pts',(-0.274884717019473,0.649532821378821,
-2.87643854221153));
#57222=CARTESIAN_POINT('Ctrl Pts',(-0.551725105308022,0.439378995711058,
-2.86058917191655));
#57223=CARTESIAN_POINT('Ctrl Pts',(-0.694580818302046,0.122523387751345,
-2.84473980162157));
#57224=CARTESIAN_POINT('Ctrl Pts',(-0.668759803500533,-0.22408663262483,
-2.82889043132659));
#57225=CARTESIAN_POINT('Ctrl Pts',(-0.48053261167355,-0.516277931755177,
-2.81304106103161));
#57226=CARTESIAN_POINT('Ctrl Pts',(-0.175609613684971,-0.683092788192513,
-2.79719169073663));
#57227=CARTESIAN_POINT('Ctrl Pts',(0.171959616715022,-0.684020748163701,
-2.78134232044165));
#57228=CARTESIAN_POINT('Ctrl Pts',(0.477769004781086,-0.518836459560908,
-2.76549295014667));
#57229=CARTESIAN_POINT('Ctrl Pts',(0.667553719770789,-0.227654397979453,
-2.74964357985169));
#57230=CARTESIAN_POINT('Ctrl Pts',(0.695225151307124,0.118812805240822,
-2.7337942095567));
#57231=CARTESIAN_POINT('Ctrl Pts',(0.55406338084068,0.436426699126669,-2.71794483926173));
#57232=CARTESIAN_POINT('Ctrl Pts',(0.278349092353365,0.648055766493336,
-2.70209546896675));
#57233=CARTESIAN_POINT('Ctrl Pts',(-0.0649613819857274,0.702306565930941,
-2.68624609867177));
#57234=CARTESIAN_POINT('Ctrl Pts',(-0.392496192704833,0.586004464497855,
-2.67039672837678));
#57235=CARTESIAN_POINT('Ctrl Pts',(-0.624714559731321,0.327393055147643,
-2.6545473580818));
#57236=CARTESIAN_POINT('Ctrl Pts',(-0.705222996156349,-0.0107247093885438,
-2.63869798778683));
#57237=CARTESIAN_POINT('Ctrl Pts',(-0.614470285968358,-0.346238012588408,
-2.62284861749184));
#57238=CARTESIAN_POINT('Ctrl Pts',(-0.374495434261829,-0.597668523026142,
-2.60699924719686));
#57239=CARTESIAN_POINT('Ctrl Pts',(-0.0435755654152151,-0.703957146279481,
-2.59114987690188));
#57240=CARTESIAN_POINT('Ctrl Pts',(0.29792648997097,-0.639292030509363,
-2.5753005066069));
#57241=CARTESIAN_POINT('Ctrl Pts',(0.567078051177426,-0.419376892033906,
-2.55945113631192));
#57242=CARTESIAN_POINT('Ctrl Pts',(0.698516523342481,-0.097617418101175,
-2.54360176601694));
#57243=CARTESIAN_POINT('Ctrl Pts',(0.660322494344382,0.247848133263131,
-2.52775239572196));
#57244=CARTESIAN_POINT('Ctrl Pts',(0.461771261834565,0.533124559031865,
-2.51190302542698));
#57245=CARTESIAN_POINT('Ctrl Pts',(0.151080356900915,0.688933392613464,
-2.496053655132));
#57246=CARTESIAN_POINT('Ctrl Pts',(-0.196299928972631,0.67743695764591,
-2.48020428483702));
#57247=CARTESIAN_POINT('Ctrl Pts',(-0.496009405614011,0.501427126551448,
-2.46435491454204));
#57248=CARTESIAN_POINT('Ctrl Pts',(-0.675264586239405,0.203647323257959,
-2.44850554424706));
#57249=CARTESIAN_POINT('Ctrl Pts',(-0.690533924178398,-0.143587580444789,
-2.43265617395207));
#57250=CARTESIAN_POINT('Ctrl Pts',(-0.538109309602317,-0.455952699979421,
-2.4168068036571));
#57251=CARTESIAN_POINT('Ctrl Pts',(-0.255006572123388,-0.657591166206698,
-2.40095743336211));
#57252=CARTESIAN_POINT('Ctrl Pts',(0.0900236949082282,-0.699535723215246,
-2.38510806306714));
#57253=CARTESIAN_POINT('Ctrl Pts',(0.413191995871872,-0.571600269634842,
-2.36925869277215));
#57254=CARTESIAN_POINT('Ctrl Pts',(0.63601794360821,-0.304853520740027,
-2.35340932247718));
#57255=CARTESIAN_POINT('Ctrl Pts',(0.704388970160089,0.0359259295776118,
-2.33755995218219));
#57256=CARTESIAN_POINT('Ctrl Pts',(0.601701390641733,0.367980882926015,
-2.32171058188722));
#57257=CARTESIAN_POINT('Ctrl Pts',(0.352892554951089,0.610672857067759,
-2.30586121159223));
#57258=CARTESIAN_POINT('Ctrl Pts',(0.0183848921922413,0.705064883140754,
-2.29001184129726));
#57259=CARTESIAN_POINT('Ctrl Pts',(-0.320587482770208,0.628234159840316,
-2.27416247100227));
#57260=CARTESIAN_POINT('Ctrl Pts',(-0.581706214008261,0.398838782321105,
-2.2583131007073));
#57261=CARTESIAN_POINT('Ctrl Pts',(-0.701559453698322,0.0725866835288543,
-2.24246373041231));
#57262=CARTESIAN_POINT('Ctrl Pts',(-0.651041226331259,-0.271292858948218,
-2.22661436011734));
#57263=CARTESIAN_POINT('Ctrl Pts',(-0.442419721672428,-0.549289799263099,
-2.21076498982235));
#57264=CARTESIAN_POINT('Ctrl Pts',(-0.126358004157817,-0.693893470559033,
-2.19491561952737));
#57265=CARTESIAN_POINT('Ctrl Pts',(0.220389350089783,-0.669987334258051,
-2.17906624923239));
#57266=CARTESIAN_POINT('Ctrl Pts',(0.513615856317125,-0.483376919017481,
-2.16321687893741));
#57267=CARTESIAN_POINT('Ctrl Pts',(0.682112396348077,-0.179379966683827,
-2.14736750864243));
#57268=CARTESIAN_POINT('Ctrl Pts',(0.684960124933254,0.168178836214988,
-2.13151813834745));
#57269=CARTESIAN_POINT('Ctrl Pts',(0.521467480303687,0.474895947218893,
-2.11566876805247));
#57270=CARTESIAN_POINT('Ctrl Pts',(0.231338127732153,0.666286097976378,
-2.09981939775749));
#57271=CARTESIAN_POINT('Ctrl Pts',(-0.114970948453971,0.695870803174554,
-2.08397002746251));
#57272=CARTESIAN_POINT('Ctrl Pts',(-0.433359697925381,0.556465511881219,
-2.06812065716753));
#57273=CARTESIAN_POINT('Ctrl Pts',(-0.646508432299333,0.28192435273503,
-2.05227128687255));
#57274=CARTESIAN_POINT('Ctrl Pts',(-0.702654663898939,-0.0610812327992534,
-2.03642191657757));
#57275=CARTESIAN_POINT('Ctrl Pts',(-0.588163460150873,-0.38925343651991,
-2.02057254628259));
#57276=CARTESIAN_POINT('Ctrl Pts',(-0.330838643304082,-0.622896689504703,
-2.00472317598761));
#57277=CARTESIAN_POINT('Ctrl Pts',(0.00682927878028947,-0.705271475852064,
-1.98887380569263));
#57278=CARTESIAN_POINT('Ctrl Pts',(0.342838732379053,-0.616373342447522,
-1.97302443539765));
#57279=CARTESIAN_POINT('Ctrl Pts',(0.59559089753061,-0.377790916351739,
-1.95717506510267));
#57280=CARTESIAN_POINT('Ctrl Pts',(0.703705720197163,-0.0474631758419071,
-1.94132569480769));
#57281=CARTESIAN_POINT('Ctrl Pts',(0.640927861859323,0.294390844952153,
-1.92547632451271));
#57282=CARTESIAN_POINT('Ctrl Pts',(0.422502724410463,0.56475299163877,-1.90962695421772));
#57283=CARTESIAN_POINT('Ctrl Pts',(0.101474153120063,0.697966682548511,
-1.89377758392275));
#57284=CARTESIAN_POINT('Ctrl Pts',(-0.244197091352646,0.661681399371415,
-1.87792821362777));
#57285=CARTESIAN_POINT('Ctrl Pts',(-0.53056585406773,0.464708906947766,
-1.86207884333278));
#57286=CARTESIAN_POINT('Ctrl Pts',(-0.688088397903683,0.154883344390378,
-1.8462294730378));
#57287=CARTESIAN_POINT('Ctrl Pts',(-0.678510877450221,-0.192555142442203,
-1.83038010274283));
#57288=CARTESIAN_POINT('Ctrl Pts',(-0.504159162883881,-0.493232229461368,
-1.81453073244784));
#57289=CARTESIAN_POINT('Ctrl Pts',(-0.207374009842694,-0.67412944880117,
-1.79868136215287));
#57290=CARTESIAN_POINT('Ctrl Pts',(0.139771257512638,-0.691316489946928,
-1.78283199185788));
#57291=CARTESIAN_POINT('Ctrl Pts',(0.45297352250471,-0.540619534986371,
-1.7669826215629));
#57292=CARTESIAN_POINT('Ctrl Pts',(0.656172617900346,-0.258634856925766,
-1.75113325126792));
#57293=CARTESIAN_POINT('Ctrl Pts',(0.700022293991506,0.0861584680346388,
-1.73528388097294));
#57294=CARTESIAN_POINT('Ctrl Pts',(0.573873797338617,0.410028484897529,
-1.71943451067796));
#57295=CARTESIAN_POINT('Ctrl Pts',(0.308361886447897,0.634324397044211,
-1.70358514038298));
#57296=CARTESIAN_POINT('Ctrl Pts',(-0.0320347212446137,0.704576660367049,
-1.687735770088));
#57297=CARTESIAN_POINT('Ctrl Pts',(-0.364651799452575,0.603724737653847,
-1.67188639979302));
#57298=CARTESIAN_POINT('Ctrl Pts',(-0.608714355716241,0.356260195424872,
-1.65603702949804));
#57299=CARTESIAN_POINT('Ctrl Pts',(-0.704952579693588,0.0222790054212492,
-1.64018765920306));
#57300=CARTESIAN_POINT('Ctrl Pts',(-0.629995326830073,-0.317112569715355,
-1.62433828890808));
#57301=CARTESIAN_POINT('Ctrl Pts',(-0.402045725983278,-0.579494372636858,
-1.6084889186131));
#57302=CARTESIAN_POINT('Ctrl Pts',(-0.0764606078631723,-0.701147822605475,
-1.59263954831812));
#57303=CARTESIAN_POINT('Ctrl Pts',(0.267692724062702,-0.652529768809897,
-1.57679017802314));
#57304=CARTESIAN_POINT('Ctrl Pts',(0.54683773505632,-0.445446949947669,
-1.56094080772816));
#57305=CARTESIAN_POINT('Ctrl Pts',(0.693184952972512,-0.130188765535679,
-1.54509143743318));
#57306=CARTESIAN_POINT('Ctrl Pts',(0.671194424519117,0.216685343744462,
-1.5292420671382));
#57307=CARTESIAN_POINT('Ctrl Pts',(0.486206479121138,0.510938111085708,
-1.51339269684322));
#57308=CARTESIAN_POINT('Ctrl Pts',(0.183144847018672,0.681111194086335,
-1.49754332654823));
#57309=CARTESIAN_POINT('Ctrl Pts',(-0.16439292478377,0.685878604404777,
-1.48169395625326));
#57310=CARTESIAN_POINT('Ctrl Pts',(-0.472008401160537,0.524082591709629,
-1.46584458595827));
#57311=CARTESIAN_POINT('Ctrl Pts',(-0.664998148605724,0.235014799640717,
-1.4499952156633));
#57312=CARTESIAN_POINT('Ctrl Pts',(-0.696495224872468,-0.111125584043703,
-1.43414584536831));
#57313=CARTESIAN_POINT('Ctrl Pts',(-0.558850665837655,-0.430279475448245,
-1.41829647507333));
#57314=CARTESIAN_POINT('Ctrl Pts',(-0.285491011948519,-0.64494137392155,
-1.40244710477835));
#57315=CARTESIAN_POINT('Ctrl Pts',(0.0571992200988665,-0.7029813247301,
-1.38659773448337));
#57316=CARTESIAN_POINT('Ctrl Pts',(0.385998804687375,-0.590304511654048,
-1.37074836418839));
#57317=CARTESIAN_POINT('Ctrl Pts',(0.62105981545978,-0.334274137977006,
-1.35489899389341));
#57318=CARTESIAN_POINT('Ctrl Pts',(0.705298438575201,0.00293363981907094,
-1.33904962359843));
#57319=CARTESIAN_POINT('Ctrl Pts',(0.618257594127741,0.339428992578101,
-1.32320025330345));
#57320=CARTESIAN_POINT('Ctrl Pts',(0.381074872501545,0.593495101283185,
-1.30735088300847));
#57321=CARTESIAN_POINT('Ctrl Pts',(0.0513493382249849,0.703432824911564,
-1.29150151271349));
#57322=CARTESIAN_POINT('Ctrl Pts',(-0.290846218427701,0.642544139281894,
-1.27565214241851));
#57323=CARTESIAN_POINT('Ctrl Pts',(-0.562410702175123,0.425615666744179,
-1.25980277212353));
#57324=CARTESIAN_POINT('Ctrl Pts',(-0.6973955476423,0.105327792286287,-1.24395340182855));
#57325=CARTESIAN_POINT('Ctrl Pts',(-0.66302011730594,-0.240538599286731,
-1.22810403153357));
#57326=CARTESIAN_POINT('Ctrl Pts',(-0.467632374358977,-0.527990962186469,
-1.21225466123859));
#57327=CARTESIAN_POINT('Ctrl Pts',(-0.158681606577905,-0.687222410456076,
-1.19640529094361));
#57328=CARTESIAN_POINT('Ctrl Pts',(0.188804481289216,-0.679564096715178,
-1.18055592064863));
#57329=CARTESIAN_POINT('Ctrl Pts',(0.490440005394944,-0.506875817935137,
-1.16470655035365));
#57330=CARTESIAN_POINT('Ctrl Pts',(0.67297374449562,-0.211094369699316,
-1.14885718005867));
#57331=CARTESIAN_POINT('Ctrl Pts',(0.692077964492487,0.135950670329878,
-1.13300780976369));
#57332=CARTESIAN_POINT('Ctrl Pts',(0.543113266727756,0.449980525360276,
-1.1171584394687));
#57333=CARTESIAN_POINT('Ctrl Pts',(0.262255251094087,0.654734050567698,
-1.10130906917373));
#57334=CARTESIAN_POINT('Ctrl Pts',(-0.0822906125712717,0.700487507941325,
-1.08545969887874));
#57335=CARTESIAN_POINT('Ctrl Pts',(-0.406852464454183,0.576129816852735,
-1.06961032858376));
#57336=CARTESIAN_POINT('Ctrl Pts',(-0.63261149801648,0.311860844410696,
-1.05376095828879));
#57337=CARTESIAN_POINT('Ctrl Pts',(-0.704742854799411,-0.0281425355713375,
-1.0379115879938));
#57338=CARTESIAN_POINT('Ctrl Pts',(-0.605729665760521,-0.361311590897459,
-1.02206221769882));
#57339=CARTESIAN_POINT('Ctrl Pts',(-0.359616966834596,-0.606737283232118,
-1.00621284740384));
#57340=CARTESIAN_POINT('Ctrl Pts',(-0.0261724389449761,-0.704818769002982,
-0.990363477108863));
#57341=CARTESIAN_POINT('Ctrl Pts',(0.313627981942751,-0.631737273430753,
-0.974514106813883));
#57342=CARTESIAN_POINT('Ctrl Pts',(0.5772648515989,-0.405240403720689,-0.958664736518902));
#57343=CARTESIAN_POINT('Ctrl Pts',(0.700714800347687,-0.0803321994775939,
-0.942815366223922));
#57344=CARTESIAN_POINT('Ctrl Pts',(0.653998403401114,0.264084422198656,
-0.926965995928941));
#57345=CARTESIAN_POINT('Ctrl Pts',(0.44846058817974,0.544368987497165,-0.911116625633962));
#57346=CARTESIAN_POINT('Ctrl Pts',(0.134015555013097,0.692455287158485,
-0.89526725533898));
#57347=CARTESIAN_POINT('Ctrl Pts',(-0.212974726593566,0.672381037456889,
-0.879417885044001));
#57348=CARTESIAN_POINT('Ctrl Pts',(-0.508244777755666,0.489021205658097,
-0.86356851474902));
#57349=CARTESIAN_POINT('Ctrl Pts',(-0.680089211952753,0.186904139827591,
-0.847719144454039));
#57350=CARTESIAN_POINT('Ctrl Pts',(-0.686776158556577,-0.160601997924922,
-0.831869774159059));
#57351=CARTESIAN_POINT('Ctrl Pts',(-0.526681713994867,-0.469106454701526,
-0.816020403864078));
#57352=CARTESIAN_POINT('Ctrl Pts',(-0.23868430153437,-0.66368991095259,
-0.800171033569099));
#57353=CARTESIAN_POINT('Ctrl Pts',(0.107276829327393,-0.697098397350523,
-0.784321663274117));
#57354=CARTESIAN_POINT('Ctrl Pts',(0.427186125669077,-0.561218769941854,
-0.768472292979137));
#57355=CARTESIAN_POINT('Ctrl Pts',(0.643354639169021,-0.289048961179428,
-0.752622922684157));
#57356=CARTESIAN_POINT('Ctrl Pts',(0.703286538458407,0.0533154623200356,
-0.736773552389177));
#57357=CARTESIAN_POINT('Ctrl Pts',(0.592427553686509,0.38273239650208,-0.720924182094196));
#57358=CARTESIAN_POINT('Ctrl Pts',(0.337699434353656,0.619203993637335,
-0.705074811799215));
#57359=CARTESIAN_POINT('Ctrl Pts',(0.00096208864391743,0.705303883503167,
-0.689225441504236));
#57360=CARTESIAN_POINT('Ctrl Pts',(-0.336008897212553,0.620122983522791,
-0.673376071209255));
#57361=CARTESIAN_POINT('Ctrl Pts',(-0.591381198224044,0.384347202521759,
-0.657526700914275));
#57362=CARTESIAN_POINT('Ctrl Pts',(-0.703138468748386,0.0552339340023888,
-0.641677330619294));
#57363=CARTESIAN_POINT('Ctrl Pts',(-0.644140813466435,-0.287292718539838,
-0.625827960324315));
#57364=CARTESIAN_POINT('Ctrl Pts',(-0.42871562406298,-0.560051254246869,
-0.609978590029332));
#57365=CARTESIAN_POINT('Ctrl Pts',(-0.109178218030051,-0.69680313604847,
-0.594129219734354));
#57366=CARTESIAN_POINT('Ctrl Pts',(0.236872768681544,-0.664338607305327,
-0.578279849439372));
#57367=CARTESIAN_POINT('Ctrl Pts',(0.525399961944826,-0.470541574876744,
-0.562430479144392));
#57368=CARTESIAN_POINT('Ctrl Pts',(0.686335456690993,-0.162475027583201,
-0.546581108849412));
#57369=CARTESIAN_POINT('Ctrl Pts',(0.680596583308102,0.185048059941882,
-0.530731738554432));
#57370=CARTESIAN_POINT('Ctrl Pts',(0.509577008823849,0.487632818601885,
-0.514882368259451));
#57371=CARTESIAN_POINT('Ctrl Pts',(0.214808289323237,0.67179750858231,-0.499032997964472));
#57372=CARTESIAN_POINT('Ctrl Pts',(-0.132125935456141,0.692818324582584,
-0.48318362766949));
#57373=CARTESIAN_POINT('Ctrl Pts',(-0.446973799862388,0.545590428747379,
-0.46733425737451));
#57374=CARTESIAN_POINT('Ctrl Pts',(-0.653275508090676,0.265867644171376,
-0.451484887079529));
#57375=CARTESIAN_POINT('Ctrl Pts',(-0.700931350885312,-0.0784202465154788,
-0.43563551678455));
#57376=CARTESIAN_POINT('Ctrl Pts',(-0.57836825932194,-0.40366403145049,
-0.419786146489569));
#57377=CARTESIAN_POINT('Ctrl Pts',(-0.315350287932037,-0.63087929875971,
-0.403936776194589));
#57378=CARTESIAN_POINT('Ctrl Pts',(0.0242494914065197,-0.704887548433319,
-0.388087405899608));
#57379=CARTESIAN_POINT('Ctrl Pts',(0.357960358964906,-0.607716113702729,
-0.372238035604628));
#57380=CARTESIAN_POINT('Ctrl Pts',(0.604741700327879,-0.362962766947641,
-0.356388665309647));
#57381=CARTESIAN_POINT('Ctrl Pts',(0.704663454379142,-0.030065073630256,
-0.340539295014667));
#57382=CARTESIAN_POINT('Ctrl Pts',(0.633459948009497,0.310133825079147,
-0.324689924719686));
#57383=CARTESIAN_POINT('Ctrl Pts',(0.408422715107778,0.575017720253068,
-0.308840554424706));
#57384=CARTESIAN_POINT('Ctrl Pts',(0.0842013460493761,0.700260397514991,
-0.292991184129726));
#57385=CARTESIAN_POINT('Ctrl Pts',(-0.260468074786106,0.655447090429983,
-0.277141813834745));
#57386=CARTESIAN_POINT('Ctrl Pts',(-0.541883609692458,0.451460534380044,
-0.261292443539765));
#57387=CARTESIAN_POINT('Ctrl Pts',(-0.691704538864457,0.137838275507889,
-0.245443073244785));
#57388=CARTESIAN_POINT('Ctrl Pts',(-0.6735470517312,-0.209257650350784,
-0.229593702949804));
#57389=CARTESIAN_POINT('Ctrl Pts',(-0.491821179438923,-0.505535863107229,
-0.213744332654824));
#57390=CARTESIAN_POINT('Ctrl Pts',(-0.190657404081973,-0.679046628726581,
-0.197894962359843));
#57391=CARTESIAN_POINT('Ctrl Pts',(0.156805532386105,-0.687652471031271,
-0.182045592064863));
#57392=CARTESIAN_POINT('Ctrl Pts',(0.466191447257558,-0.529265333633324,
-0.166196221769883));
#57393=CARTESIAN_POINT('Ctrl Pts',(0.662358975760562,-0.242345413653074,
-0.150346851474902));
#57394=CARTESIAN_POINT('Ctrl Pts',(0.697685099148249,0.103422631371823,
-0.134497481179922));
#57395=CARTESIAN_POINT('Ctrl Pts',(0.563560339571208,0.424084008064863,
-0.118648110884941));
#57396=CARTESIAN_POINT('Ctrl Pts',(0.292616745553076,0.64173975329643,-0.102798740589961));
#57397=CARTESIAN_POINT('Ctrl Pts',(-0.0494690429576347,0.703588850062655,
-0.0869493702949807));
#57398=CARTESIAN_POINT('Ctrl Pts',(-0.269389956604521,0.630845896423734,
-0.0763831234316606));
#57399=CARTESIAN_POINT('Ctrl Pts',(-0.364065050236245,0.570420484551949,
-0.0711000000000004));
#57400=CARTESIAN_POINT('Ctrl Pts',(-0.309090610374644,0.644553868208604,
-3.8529325805302));
#57401=CARTESIAN_POINT('Ctrl Pts',(-0.416069934357496,0.593252795981349,
-3.84764945709854));
#57402=CARTESIAN_POINT('Ctrl Pts',(-0.60388618139578,0.436410482080527,
-3.83708321023521));
#57403=CARTESIAN_POINT('Ctrl Pts',(-0.738976101494388,0.0949394031846672,
-3.82123383994024));
#57404=CARTESIAN_POINT('Ctrl Pts',(-0.694596745603902,-0.269493513544402,
-3.80538446964525));
#57405=CARTESIAN_POINT('Ctrl Pts',(-0.481542751643377,-0.56852681641803,
-3.78953509935028));
#57406=CARTESIAN_POINT('Ctrl Pts',(-0.151544581786972,-0.729471873763095,
-3.77368572905529));
#57407=CARTESIAN_POINT('Ctrl Pts',(0.215254139712002,-0.713278921282305,
-3.75783635876032));
#57408=CARTESIAN_POINT('Ctrl Pts',(0.529779882009245,-0.523862390353358,
-3.74198698846533));
#57409=CARTESIAN_POINT('Ctrl Pts',(0.715649867888453,-0.207230658674656,
-3.72613761817036));
#57410=CARTESIAN_POINT('Ctrl Pts',(0.727726783308574,0.159727960083829,
-3.71028824787537));
#57411=CARTESIAN_POINT('Ctrl Pts',(0.563077472927324,0.487896345511823,
-3.69443887758039));
#57412=CARTESIAN_POINT('Ctrl Pts',(0.261686655537168,0.697581079138808,
-3.67858950728541));
#57413=CARTESIAN_POINT('Ctrl Pts',(-0.103253956067285,0.737860270003995,
-3.66274013699043));
#57414=CARTESIAN_POINT('Ctrl Pts',(-0.443119660846356,0.59895256469117,
-3.64689076669546));
#57415=CARTESIAN_POINT('Ctrl Pts',(-0.675375182033268,0.31459109167952,
-3.63104139640047));
#57416=CARTESIAN_POINT('Ctrl Pts',(-0.743617998995764,-0.0461677925321744,
-3.6151920261055));
#57417=CARTESIAN_POINT('Ctrl Pts',(-0.631275567731624,-0.395714990525769,
-3.5993426558105));
#57418=CARTESIAN_POINT('Ctrl Pts',(-0.365629885114147,-0.649164062738602,
-3.58349328551553));
#57419=CARTESIAN_POINT('Ctrl Pts',(-0.0111921560746506,-0.74496572457859,
-3.56764391522055));
#57420=CARTESIAN_POINT('Ctrl Pts',(0.345963552484283,-0.659854843541832,
-3.55179454492557));
#57421=CARTESIAN_POINT('Ctrl Pts',(0.619103119909842,-0.414500327471964,
-3.53594517463059));
#57422=CARTESIAN_POINT('Ctrl Pts',(0.741895476993479,-0.0684857335349459,
-3.52009580433561));
#57423=CARTESIAN_POINT('Ctrl Pts',(0.684520892878228,0.294160401256122,
-3.50424643404063));
#57424=CARTESIAN_POINT('Ctrl Pts',(0.460912601663608,0.585370624583888,
-3.48839706374565));
#57425=CARTESIAN_POINT('Ctrl Pts',(0.125373160889622,0.734425465921584,
-3.47254769345066));
#57426=CARTESIAN_POINT('Ctrl Pts',(-0.24061275057849,0.705127434399112,
-3.45669832315569));
#57427=CARTESIAN_POINT('Ctrl Pts',(-0.548166625971821,0.504591463113016,
-3.44084895286071));
#57428=CARTESIAN_POINT('Ctrl Pts',(-0.722599991382613,0.181517070634459,
-3.42499958256572));
#57429=CARTESIAN_POINT('Ctrl Pts',(-0.721552262528453,-0.185638161265563,
-3.40915021227075));
#57430=CARTESIAN_POINT('Ctrl Pts',(-0.545277877006026,-0.507711760081603,
-3.39330084197576));
#57431=CARTESIAN_POINT('Ctrl Pts',(-0.236584504939444,-0.706489183569325,
-3.37745147168079));
#57432=CARTESIAN_POINT('Ctrl Pts',(0.129562656648595,-0.733697970884298,
-3.3616021013858));
#57433=CARTESIAN_POINT('Ctrl Pts',(0.464245941906974,-0.582730555145881,
-3.34575273109082));
#57434=CARTESIAN_POINT('Ctrl Pts',(0.686188586609458,-0.290248889893811,
-3.32990336079585));
#57435=CARTESIAN_POINT('Ctrl Pts',(0.741492530112445,0.0727187889415322,
-3.31405399050086));
#57436=CARTESIAN_POINT('Ctrl Pts',(0.616727386810033,0.418026942715604,
-3.29820462020588));
#57437=CARTESIAN_POINT('Ctrl Pts',(0.342191972276529,0.661818591902024,
-3.2823552499109));
#57438=CARTESIAN_POINT('Ctrl Pts',(-0.015443667084096,0.74488971507511,
-3.26650587961592));
#57439=CARTESIAN_POINT('Ctrl Pts',(-0.369328861341332,0.647066755951808,
-3.25065650932095));
#57440=CARTESIAN_POINT('Ctrl Pts',(-0.633523724149739,0.392105706942817,
-3.23480713902596));
#57441=CARTESIAN_POINT('Ctrl Pts',(-0.743869378983116,0.041923042458244,
-3.21895776873098));
#57442=CARTESIAN_POINT('Ctrl Pts',(-0.673568736873105,-0.318440498656892,
-3.203108398436));
#57443=CARTESIAN_POINT('Ctrl Pts',(-0.439694083665483,-0.601471784265275,
-3.18725902814102));
#57444=CARTESIAN_POINT('Ctrl Pts',(-0.0990411300650332,-0.73843757287473,
-3.17140965784604));
#57445=CARTESIAN_POINT('Ctrl Pts',(0.265663644858933,-0.696076161262508,
-3.15556028755106));
#57446=CARTESIAN_POINT('Ctrl Pts',(0.565852854238509,-0.484674882604632,
-3.13971091725608));
#57447=CARTESIAN_POINT('Ctrl Pts',(0.728626509730431,-0.155571860552392,
-3.1238615469611));
#57448=CARTESIAN_POINT('Ctrl Pts',(0.714455550271918,0.211311289720478,
-3.10801217666611));
#57449=CARTESIAN_POINT('Ctrl Pts',(0.526781347994482,0.526878169867379,
-3.09216280637114));
#57450=CARTESIAN_POINT('Ctrl Pts',(0.211179982020463,0.714494373435872,
-3.07631343607615));
#57451=CARTESIAN_POINT('Ctrl Pts',(-0.155705766425003,0.728597906104378,
-3.06046406578118));
#57452=CARTESIAN_POINT('Ctrl Pts',(-0.48477886803742,0.565763770121453,
-3.04461469548619));
#57453=CARTESIAN_POINT('Ctrl Pts',(-0.696124973726058,0.265535714043468,
-3.02876532519122));
#57454=CARTESIAN_POINT('Ctrl Pts',(-0.738419358418565,-0.0991768399899824,
-3.01291595489623));
#57455=CARTESIAN_POINT('Ctrl Pts',(-0.60139096621175,-0.439804615979164,
-2.99706658460126));
#57456=CARTESIAN_POINT('Ctrl Pts',(-0.318316703411543,-0.673627249157046,
-2.98121721430627));
#57457=CARTESIAN_POINT('Ctrl Pts',(0.0420597516164567,-0.743861661716508,
-2.9653678440113));
#57458=CARTESIAN_POINT('Ctrl Pts',(0.392222130632537,-0.633451651446071,
-2.94951847371631));
#57459=CARTESIAN_POINT('Ctrl Pts',(0.647134621052763,-0.36920993582592,
-2.93366910342134));
#57460=CARTESIAN_POINT('Ctrl Pts',(0.744892540764818,-0.0153067694375815,
-2.91781973312635));
#57461=CARTESIAN_POINT('Ctrl Pts',(0.661755691970793,0.342313596899012,
-2.90197036283138));
#57462=CARTESIAN_POINT('Ctrl Pts',(0.417913592210328,0.616804202258335,
-2.88612099253639));
#57463=CARTESIAN_POINT('Ctrl Pts',(0.0725825146695105,0.7415058820009,-2.87027162224141));
#57464=CARTESIAN_POINT('Ctrl Pts',(-0.290374994161988,0.686135232474697,
-2.85442225194643));
#57465=CARTESIAN_POINT('Ctrl Pts',(-0.582815865392368,0.464138838629808,
-2.83857288165145));
#57466=CARTESIAN_POINT('Ctrl Pts',(-0.733721769789043,0.129427813916935,
-2.82272351135647));
#57467=CARTESIAN_POINT('Ctrl Pts',(-0.706445691644203,-0.23671434099992,
-2.80687414106149));
#57468=CARTESIAN_POINT('Ctrl Pts',(-0.507611539201978,-0.545371176123821,
-2.79102477076651));
#57469=CARTESIAN_POINT('Ctrl Pts',(-0.185505549749978,-0.721586367311385,
-2.77517540047153));
#57470=CARTESIAN_POINT('Ctrl Pts',(0.181649868501726,-0.722566619593644,
-2.75932603017655));
#57471=CARTESIAN_POINT('Ctrl Pts',(0.504692197799631,-0.548073881842458,
-2.74347665988157));
#57472=CARTESIAN_POINT('Ctrl Pts',(0.705171642800086,-0.240483156724765,
-2.72762728958659));
#57473=CARTESIAN_POINT('Ctrl Pts',(0.734402412185669,0.125508133017552,
-2.71177791929161));
#57474=CARTESIAN_POINT('Ctrl Pts',(0.585285907203018,0.46102017451216,-2.69592854899663));
#57475=CARTESIAN_POINT('Ctrl Pts',(0.294034593641594,0.684574942734325,
-2.68007917870165));
#57476=CARTESIAN_POINT('Ctrl Pts',(-0.068622079537157,0.741882878005469,
-2.66422980840666));
#57477=CARTESIAN_POINT('Ctrl Pts',(-0.414614100416485,0.619026931735213,
-2.64838043811169));
#57478=CARTESIAN_POINT('Ctrl Pts',(-0.659918414533182,0.345842277111536,
-2.6325310678167));
#57479=CARTESIAN_POINT('Ctrl Pts',(-0.744963654626517,-0.0113290671807901,
-2.61668169752173));
#57480=CARTESIAN_POINT('Ctrl Pts',(-0.649096856440149,-0.365749183781997,
-2.60083232722674));
#57481=CARTESIAN_POINT('Ctrl Pts',(-0.395598964964535,-0.631348282168147,
-2.58498295693176));
#57482=CARTESIAN_POINT('Ctrl Pts',(-0.0460311314875812,-0.743626471699101,
-2.56913358663678));
#57483=CARTESIAN_POINT('Ctrl Pts',(0.314715214887314,-0.675317353542847,
-2.5532842163418));
#57484=CARTESIAN_POINT('Ctrl Pts',(0.599033978991175,-0.443009578329501,
-2.53743484604682));
#57485=CARTESIAN_POINT('Ctrl Pts',(0.737879259301487,-0.10311834545982,
-2.52158547575185));
#57486=CARTESIAN_POINT('Ctrl Pts',(0.697532924053757,0.261814847437454,
-2.50573610545686));
#57487=CARTESIAN_POINT('Ctrl Pts',(0.487792951580825,0.563167142920953,
-2.48988673516189));
#57488=CARTESIAN_POINT('Ctrl Pts',(0.159594022646185,0.727756100911073,
-2.4740373648669));
#57489=CARTESIAN_POINT('Ctrl Pts',(-0.207361803695285,0.715611819945646,
-2.45818799457192));
#57490=CARTESIAN_POINT('Ctrl Pts',(-0.523960479946426,0.529683499773207,
-2.44233862427694));
#57491=CARTESIAN_POINT('Ctrl Pts',(-0.713317031274519,0.215123237636915,
-2.42648925398196));
#57492=CARTESIAN_POINT('Ctrl Pts',(-0.729446825476861,-0.151679013971647,
-2.41063988368698));
#57493=CARTESIAN_POINT('Ctrl Pts',(-0.568432793676261,-0.481646502687485,
-2.394790513392));
#57494=CARTESIAN_POINT('Ctrl Pts',(-0.269376677956068,-0.694647680375479,
-2.37894114309702));
#57495=CARTESIAN_POINT('Ctrl Pts',(0.0950967015076525,-0.738955893027485,
-2.36309177280204));
#57496=CARTESIAN_POINT('Ctrl Pts',(0.436476151493632,-0.603811033068285,
-2.34724240250705));
#57497=CARTESIAN_POINT('Ctrl Pts',(0.671858765611449,-0.322032597028224,
-2.33139303221208));
#57498=CARTESIAN_POINT('Ctrl Pts',(0.744082629677508,0.037950424106782,
-2.3155436619171));
#57499=CARTESIAN_POINT('Ctrl Pts',(0.635608409551846,0.388717306258229,
-2.29969429162212));
#57500=CARTESIAN_POINT('Ctrl Pts',(0.372778722276054,0.645085435191274,
-2.28384492132714));
#57501=CARTESIAN_POINT('Ctrl Pts',(0.0194209158693028,0.744796631641469,
-2.26799555103216));
#57502=CARTESIAN_POINT('Ctrl Pts',(-0.338653197773854,0.663636350809105,
-2.25214618073718));
#57503=CARTESIAN_POINT('Ctrl Pts',(-0.614486466647313,0.421314107032963,
-2.23629681044219));
#57504=CARTESIAN_POINT('Ctrl Pts',(-0.741093664576154,0.0766770813396573,
-2.22044744014722));
#57505=CARTESIAN_POINT('Ctrl Pts',(-0.687728638917978,-0.286580728050069,
-2.20459806985223));
#57506=CARTESIAN_POINT('Ctrl Pts',(-0.467350915288179,-0.580243325215363,
-2.18874869955726));
#57507=CARTESIAN_POINT('Ctrl Pts',(-0.133478518258434,-0.732995688692106,
-2.17289932926227));
#57508=CARTESIAN_POINT('Ctrl Pts',(0.232808709554962,-0.707742396096938,
-2.1570499589673));
#57509=CARTESIAN_POINT('Ctrl Pts',(0.542559087666651,-0.510616128679865,
-2.14120058867231));
#57510=CARTESIAN_POINT('Ctrl Pts',(0.720550728519998,-0.189488369318495,
-2.12535121837734));
#57511=CARTESIAN_POINT('Ctrl Pts',(0.723558932032592,0.177656033822487,
-2.10950184808235));
#57512=CARTESIAN_POINT('Ctrl Pts',(0.550853165613154,0.501657237973947,
-2.09365247778737));
#57513=CARTESIAN_POINT('Ctrl Pts',(0.244374471662288,0.703832588104202,
-2.07780310749239));
#57514=CARTESIAN_POINT('Ctrl Pts',(-0.121449780286455,0.735084447765053,
-2.06195373719741));
#57515=CARTESIAN_POINT('Ctrl Pts',(-0.457780341954077,0.587823402900981,
-2.04610436690243));
#57516=CARTESIAN_POINT('Ctrl Pts',(-0.682940413312603,0.297811326752515,
-2.03025499660745));
#57517=CARTESIAN_POINT('Ctrl Pts',(-0.74225059195669,-0.0645232765568143,
-2.01440562631247));
#57518=CARTESIAN_POINT('Ctrl Pts',(-0.621307590903676,-0.41118860874683,
-1.99855625601749));
#57519=CARTESIAN_POINT('Ctrl Pts',(-0.349482030720463,-0.657998103858348,
-1.98270688572251));
#57520=CARTESIAN_POINT('Ctrl Pts',(0.00721412164145659,-0.745014866245382,
-1.96685751542753));
#57521=CARTESIAN_POINT('Ctrl Pts',(0.362158347661135,-0.651107153775044,
-1.95100814513255));
#57522=CARTESIAN_POINT('Ctrl Pts',(0.629153578520462,-0.399080153744305,
-1.93515877483757));
#57523=CARTESIAN_POINT('Ctrl Pts',(0.743360877278368,-0.0501378161632328,
-1.91930940454259));
#57524=CARTESIAN_POINT('Ctrl Pts',(0.67704536710375,0.310980329540358,-1.90346003424761));
#57525=CARTESIAN_POINT('Ctrl Pts',(0.446311557311583,0.596577897920959,
-1.88761066395263));
#57526=CARTESIAN_POINT('Ctrl Pts',(0.107192414839656,0.737298433931963,
-1.87176129365765));
#57527=CARTESIAN_POINT('Ctrl Pts',(-0.257958062364287,0.69896840596621,
-1.85591192336267));
#57528=CARTESIAN_POINT('Ctrl Pts',(-0.560464250060707,0.490896138588981,
-1.84006255306769));
#57529=CARTESIAN_POINT('Ctrl Pts',(-0.726863489140655,0.163611315720987,
-1.8242131827727));
#57530=CARTESIAN_POINT('Ctrl Pts',(-0.716746257175511,-0.203405991314366,
-1.80836381247773));
#57531=CARTESIAN_POINT('Ctrl Pts',(-0.532569491554352,-0.521026804630263,
-1.79251444218274));
#57532=CARTESIAN_POINT('Ctrl Pts',(-0.219059930105742,-0.712117926680512,
-1.77666507188777));
#57533=CARTESIAN_POINT('Ctrl Pts',(0.147647633976574,-0.730273490316333,
-1.76081570159278));
#57534=CARTESIAN_POINT('Ctrl Pts',(0.478499442890174,-0.571084475039791,
-1.7449663312978));
#57535=CARTESIAN_POINT('Ctrl Pts',(0.693149194171365,-0.27320942351476,
-1.72911696100282));
#57536=CARTESIAN_POINT('Ctrl Pts',(0.739469882993344,0.0910136617409349,
-1.71326759070784));
#57537=CARTESIAN_POINT('Ctrl Pts',(0.606212678386616,0.433134370653044,
-1.69741822041286));
#57538=CARTESIAN_POINT('Ctrl Pts',(0.325738665823124,0.670069784474314,
-1.68156885011788));
#57539=CARTESIAN_POINT('Ctrl Pts',(-0.0338399387759541,0.744280896584965,
-1.6657194798229));
#57540=CARTESIAN_POINT('Ctrl Pts',(-0.385200622592994,0.637745776020236,
-1.64987010952792));
#57541=CARTESIAN_POINT('Ctrl Pts',(-0.64301656855991,0.376336135702008,
-1.63402073923294));
#57542=CARTESIAN_POINT('Ctrl Pts',(-0.744677999681247,0.0235344697925616,
-1.61817136893796));
#57543=CARTESIAN_POINT('Ctrl Pts',(-0.665496762911727,-0.334982466752658,
-1.60232199864298));
#57544=CARTESIAN_POINT('Ctrl Pts',(-0.424701768076029,-0.612149983803623,
-1.586472628348));
#57545=CARTESIAN_POINT('Ctrl Pts',(-0.0807693086855734,-0.740658837287543,
-1.57062325805302));
#57546=CARTESIAN_POINT('Ctrl Pts',(0.282777718709647,-0.689301063599245,
-1.55477388775804));
#57547=CARTESIAN_POINT('Ctrl Pts',(0.577653082522177,-0.470548733640108,
-1.53892451746306));
#57548=CARTESIAN_POINT('Ctrl Pts',(0.732247244790675,-0.137525150333124,
-1.52307514716808));
#57549=CARTESIAN_POINT('Ctrl Pts',(0.709017508192331,0.228895975400221,
-1.5072257768731));
#57550=CARTESIAN_POINT('Ctrl Pts',(0.513605139882413,0.539730446393427,
-1.49137640657812));
#57551=CARTESIAN_POINT('Ctrl Pts',(0.193465407827965,0.719493106604671,
-1.47552703628314));
#57552=CARTESIAN_POINT('Ctrl Pts',(-0.173656779074324,0.72452916957098,
-1.45967766598816));
#57553=CARTESIAN_POINT('Ctrl Pts',(-0.498606973197754,0.553615643525593,
-1.44382829569318));
#57554=CARTESIAN_POINT('Ctrl Pts',(-0.702472060334454,0.24825833103272,
-1.4279789253982));
#57555=CARTESIAN_POINT('Ctrl Pts',(-0.735744056814447,-0.117387722270682,
-1.41212955510321));
#57556=CARTESIAN_POINT('Ctrl Pts',(-0.59034296482383,-0.454526543076082,
-1.39628018480824));
#57557=CARTESIAN_POINT('Ctrl Pts',(-0.301578974003058,-0.681285048211793,
-1.38043081451325));
#57558=CARTESIAN_POINT('Ctrl Pts',(0.0604225050500024,-0.742595660747599,
-1.36458144421827));
#57559=CARTESIAN_POINT('Ctrl Pts',(0.407750572214209,-0.62356929473529,
-1.3487320739233));
#57560=CARTESIAN_POINT('Ctrl Pts',(0.656057718463867,-0.353111122058863,
-1.33288270362831));
#57561=CARTESIAN_POINT('Ctrl Pts',(0.7450433483693,0.00309895600807202,
-1.31703333333333));
#57562=CARTESIAN_POINT('Ctrl Pts',(0.653097586624771,0.358556462530776,
-1.30118396303835));
#57563=CARTESIAN_POINT('Ctrl Pts',(0.402549167075302,0.626939680164418,
-1.28533459274337));
#57564=CARTESIAN_POINT('Ctrl Pts',(0.0542429711952568,0.743072603823875,
-1.26948522244839));
#57565=CARTESIAN_POINT('Ctrl Pts',(-0.307235956562828,0.678752724836228,
-1.25363585215341));
#57566=CARTESIAN_POINT('Ctrl Pts',(-0.594103615986673,0.44959991987237,
-1.23778648185843));
#57567=CARTESIAN_POINT('Ctrl Pts',(-0.736695114486434,0.111263213909636,
-1.22193711156345));
#57568=CARTESIAN_POINT('Ctrl Pts',(-0.70038256320506,-0.254093407305248,
-1.20608774126847));
#57569=CARTESIAN_POINT('Ctrl Pts',(-0.49398434895465,-0.557744258119735,
-1.19023837097349));
#57570=CARTESIAN_POINT('Ctrl Pts',(-0.167623617214091,-0.72594870165167,
-1.17438900067851));
#57571=CARTESIAN_POINT('Ctrl Pts',(0.199443973264722,-0.717858827351214,
-1.15853963038353));
#57572=CARTESIAN_POINT('Ctrl Pts',(0.518077233421729,-0.535439235289842,
-1.14269026008855));
#57573=CARTESIAN_POINT('Ctrl Pts',(0.710897096237059,-0.222989939323281,
-1.12684088979357));
#57574=CARTESIAN_POINT('Ctrl Pts',(0.731077875402266,0.143611749432251,
-1.11099151949859));
#57575=CARTESIAN_POINT('Ctrl Pts',(0.573718733312487,0.475337784658443,
-1.09514214920361));
#57576=CARTESIAN_POINT('Ctrl Pts',(0.277033833787142,0.691629560830709,
-1.07929277890863));
#57577=CARTESIAN_POINT('Ctrl Pts',(-0.086927845258402,0.739961312634932,
-1.06344340861365));
#57578=CARTESIAN_POINT('Ctrl Pts',(-0.429779375411057,0.60859582889547,
-1.04759403831867));
#57579=CARTESIAN_POINT('Ctrl Pts',(-0.668260360325273,0.329434796728608,
-1.03174466802369));
#57580=CARTESIAN_POINT('Ctrl Pts',(-0.744456456389999,-0.0297284210298624,
-1.01589529772871));
#57581=CARTESIAN_POINT('Ctrl Pts',(-0.639863685642797,-0.381672186926551,
-1.00004592743373));
#57582=CARTESIAN_POINT('Ctrl Pts',(-0.379882067571449,-0.640928084277264,
-0.984196557138746));
#57583=CARTESIAN_POINT('Ctrl Pts',(-0.0276473057078523,-0.744536648503469,
-0.968347186843765));
#57584=CARTESIAN_POINT('Ctrl Pts',(0.331301515824945,-0.667336871519755,
-0.952497816548785));
#57585=CARTESIAN_POINT('Ctrl Pts',(0.60979482501051,-0.428076471986122,
-0.936648446253804));
#57586=CARTESIAN_POINT('Ctrl Pts',(0.740201413401119,-0.0848590718583864,
-0.920799075958824));
#57587=CARTESIAN_POINT('Ctrl Pts',(0.690852458545734,0.278966082165907,
-0.904949705663843));
#57588=CARTESIAN_POINT('Ctrl Pts',(0.473732196124063,0.575045216337946,
-0.889100335368864));
#57589=CARTESIAN_POINT('Ctrl Pts',(0.141567586683216,0.731476460918855,
-0.873250965073882));
#57590=CARTESIAN_POINT('Ctrl Pts',(-0.224976257908425,0.710270989028275,
-0.857401594778903));
#57591=CARTESIAN_POINT('Ctrl Pts',(-0.53688533860254,0.516578481618539,
-0.841552224483921));
#57592=CARTESIAN_POINT('Ctrl Pts',(-0.718413533832164,0.197436543943786,
-0.825702854188942));
#57593=CARTESIAN_POINT('Ctrl Pts',(-0.72547730260804,-0.169652226269635,
-0.809853483893961));
#57594=CARTESIAN_POINT('Ctrl Pts',(-0.556361231299935,-0.495541496530917,
-0.79400411359898));
#57595=CARTESIAN_POINT('Ctrl Pts',(-0.252134616344252,-0.701090100998879,
-0.778154743304001));
#57596=CARTESIAN_POINT('Ctrl Pts',(0.113322082898667,-0.736381219209989,
-0.762305373009019));
#57597=CARTESIAN_POINT('Ctrl Pts',(0.451258877147593,-0.592844516102809,
-0.74645600271404));
#57598=CARTESIAN_POINT('Ctrl Pts',(0.679608897935057,-0.305337420446921,
-0.730606632419059));
#57599=CARTESIAN_POINT('Ctrl Pts',(0.742918073850576,0.0563198901262535,
-0.714757262124078));
#57600=CARTESIAN_POINT('Ctrl Pts',(0.625811974228227,0.404300095708931,
-0.698907891829099));
#57601=CARTESIAN_POINT('Ctrl Pts',(0.356729440407579,0.654097317548526,
-0.683058521534117));
#57602=CARTESIAN_POINT('Ctrl Pts',(0.00101630417067649,0.745049100129323,
-0.667209151239138));
#57603=CARTESIAN_POINT('Ctrl Pts',(-0.354943638280041,0.655068094263647,
-0.651359780944157));
#57604=CARTESIAN_POINT('Ctrl Pts',(-0.624706654643346,0.406005899122171,
-0.635510410649177));
#57605=CARTESIAN_POINT('Ctrl Pts',(-0.742761660130492,0.0583464713403934,
-0.619661040354196));
#57606=CARTESIAN_POINT('Ctrl Pts',(-0.680439374650891,-0.303482210190962,
-0.603811670059217));
#57607=CARTESIAN_POINT('Ctrl Pts',(-0.452874565687931,-0.591611208675634,
-0.587962299764235));
#57608=CARTESIAN_POINT('Ctrl Pts',(-0.115330618474684,-0.736069319371431,
-0.572112929469256));
#57609=CARTESIAN_POINT('Ctrl Pts',(0.250221000166279,-0.701775352626115,
-0.556263559174274));
#57610=CARTESIAN_POINT('Ctrl Pts',(0.555007250081607,-0.497057488460266,
-0.540414188879294));
#57611=CARTESIAN_POINT('Ctrl Pts',(0.7250117663533,-0.171630804715129,-0.524564818584314));
#57612=CARTESIAN_POINT('Ctrl Pts',(0.718949496529346,0.195475870422815,
-0.508715448289334));
#57613=CARTESIAN_POINT('Ctrl Pts',(0.538292643427788,0.515111856308425,
-0.492866077994354));
#57614=CARTESIAN_POINT('Ctrl Pts',(0.226913145388744,0.709654577190661,
-0.477016707699373));
#57615=CARTESIAN_POINT('Ctrl Pts',(-0.139571483466669,0.731859956192972,
-0.461167337404393));
#57616=CARTESIAN_POINT('Ctrl Pts',(-0.472161624454404,0.576335488128052,
-0.445317967109412));
#57617=CARTESIAN_POINT('Ctrl Pts',(-0.690088826708267,0.280849792091782,
-0.429468596814432));
#57618=CARTESIAN_POINT('Ctrl Pts',(-0.740430166973819,-0.0828393767067807,
-0.413619226519452));
#57619=CARTESIAN_POINT('Ctrl Pts',(-0.61096041185947,-0.426411268137316,
-0.397769856224471));
#57620=CARTESIAN_POINT('Ctrl Pts',(-0.333120877035743,-0.666430548342542,
-0.381920485929491));
#57621=CARTESIAN_POINT('Ctrl Pts',(0.0256159964145952,-0.744609303785652,
-0.36607111563451));
#57622=CARTESIAN_POINT('Ctrl Pts',(0.378132106694367,-0.641962073708442,
-0.35022174533953));
#57623=CARTESIAN_POINT('Ctrl Pts',(0.638820046477084,-0.383416409890756,
-0.334372375044549));
#57624=CARTESIAN_POINT('Ctrl Pts',(0.744372581604882,-0.0317592977686295,
-0.318523004749569));
#57625=CARTESIAN_POINT('Ctrl Pts',(0.66915662209072,0.327610456569737,-0.302673634454589));
#57626=CARTESIAN_POINT('Ctrl Pts',(0.431438112678508,0.607421063535145,
-0.286824264159608));
#57627=CARTESIAN_POINT('Ctrl Pts',(0.0889462522057513,0.739721404103688,
-0.270974893864627));
#57628=CARTESIAN_POINT('Ctrl Pts',(-0.275145946691687,0.692382781846757,
-0.255125523569648));
#57629=CARTESIAN_POINT('Ctrl Pts',(-0.572419782762165,0.476901195004193,
-0.239276153274667));
#57630=CARTESIAN_POINT('Ctrl Pts',(-0.730683406529149,0.145605724755764,
-0.223426782979687));
#57631=CARTESIAN_POINT('Ctrl Pts',(-0.711502710426857,-0.221049717342616,
-0.207577412684706));
#57632=CARTESIAN_POINT('Ctrl Pts',(-0.519536239252636,-0.534023771456305,
-0.191728042389726));
#57633=CARTESIAN_POINT('Ctrl Pts',(-0.201401311784543,-0.717312199056277,
-0.175878672094745));
#57634=CARTESIAN_POINT('Ctrl Pts',(0.165641822669815,-0.726402996959048,
-0.160029301799765));
#57635=CARTESIAN_POINT('Ctrl Pts',(0.492462222867754,-0.559090442823836,
-0.144179931504785));
#57636=CARTESIAN_POINT('Ctrl Pts',(0.699684165074883,-0.256002039101042,
-0.128330561209804));
#57637=CARTESIAN_POINT('Ctrl Pts',(0.737000982771008,0.109250693550497,
-0.112481190914824));
#57638=CARTESIAN_POINT('Ctrl Pts',(0.595318037638767,0.447981949310424,
-0.0966318206198438));
#57639=CARTESIAN_POINT('Ctrl Pts',(0.309106256262539,0.67790301016905,-0.0807824503248628));
#57640=CARTESIAN_POINT('Ctrl Pts',(-0.0522567177097866,0.743237421289278,
-0.0649330800298829));
#57641=CARTESIAN_POINT('Ctrl Pts',(-0.284570593536469,0.666395263721345,
-0.0543668331665628));
#57642=CARTESIAN_POINT('Ctrl Pts',(-0.384580808941244,0.60256476484984,
-0.0490837097349025));
#57643=CARTESIAN_POINT('Ctrl Pts',(-0.325579286442189,0.678938089483059,
-3.8309162902651));
#57644=CARTESIAN_POINT('Ctrl Pts',(-0.438265504649167,0.624900322146083,
-3.82563316683344));
#57645=CARTESIAN_POINT('Ctrl Pts',(-0.63610095367448,0.459691134517002,
-3.81506691997012));
#57646=CARTESIAN_POINT('Ctrl Pts',(-0.778397349342817,0.100004018584218,
-3.79921754967514));
#57647=CARTESIAN_POINT('Ctrl Pts',(-0.731650542618167,-0.283869852061292,
-3.78336817938015));
#57648=CARTESIAN_POINT('Ctrl Pts',(-0.507231019672293,-0.598855316207359,
-3.76751880908518));
#57649=CARTESIAN_POINT('Ctrl Pts',(-0.159628843925671,-0.76838611128163,
-3.75166943879019));
#57650=CARTESIAN_POINT('Ctrl Pts',(0.22673703716271,-0.751329333310609,
-3.73582006849522));
#57651=CARTESIAN_POINT('Ctrl Pts',(0.558041396815425,-0.551808232021081,
-3.71997069820023));
#57652=CARTESIAN_POINT('Ctrl Pts',(0.753826759884924,-0.218285537365442,
-3.70412132790526));
#57653=CARTESIAN_POINT('Ctrl Pts',(0.766547927636159,0.168248770824598,
-3.68827195761027));
#57654=CARTESIAN_POINT('Ctrl Pts',(0.59311527330172,0.513923550886757,-3.67242258731529));
#57655=CARTESIAN_POINT('Ctrl Pts',(0.275646531216097,0.734794077718187,
-3.65657321702032));
#57656=CARTESIAN_POINT('Ctrl Pts',(-0.108762117677957,0.777221992964339,
-3.64072384672533));
#57657=CARTESIAN_POINT('Ctrl Pts',(-0.466758219578375,0.630904149396545,
-3.62487447643035));
#57658=CARTESIAN_POINT('Ctrl Pts',(-0.711403589971996,0.331373195147995,
-3.60902510613537));
#57659=CARTESIAN_POINT('Ctrl Pts',(-0.783286872432518,-0.0486306488929434,
-3.59317573584039));
#57660=CARTESIAN_POINT('Ctrl Pts',(-0.664951447866154,-0.416824710701167,
-3.57732636554541));
#57661=CARTESIAN_POINT('Ctrl Pts',(-0.385134692228658,-0.68379421838201,
-3.56147699525044));
#57662=CARTESIAN_POINT('Ctrl Pts',(-0.0117892102387679,-0.78470649347194,
-3.54562762495545));
#57663=CARTESIAN_POINT('Ctrl Pts',(0.364419243976096,-0.695055307100327,
-3.52977825466047));
#57664=CARTESIAN_POINT('Ctrl Pts',(0.652129651463901,-0.436612165878492,
-3.51392888436549));
#57665=CARTESIAN_POINT('Ctrl Pts',(0.781472461170702,-0.0721391576041502,
-3.49807951407051));
#57666=CARTESIAN_POINT('Ctrl Pts',(0.721037185788124,0.30985261384819,-3.48223014377553));
#57667=CARTESIAN_POINT('Ctrl Pts',(0.485500338492858,0.616597670259985,
-3.46638077348055));
#57668=CARTESIAN_POINT('Ctrl Pts',(0.132061288474505,0.773603956619382,
-3.45053140318557));
#57669=CARTESIAN_POINT('Ctrl Pts',(-0.25344842260748,0.742742999097299,
-3.43468203289059));
#57670=CARTESIAN_POINT('Ctrl Pts',(-0.577408995760196,0.531509282362323,
-3.41883266259561));
#57671=CARTESIAN_POINT('Ctrl Pts',(-0.761147643056275,0.191200238216922,
-3.40298329230063));
#57672=CARTESIAN_POINT('Ctrl Pts',(-0.760044022301481,-0.195541171593737,
-3.38713392200565));
#57673=CARTESIAN_POINT('Ctrl Pts',(-0.574366144261561,-0.534796033969841,
-3.37128455171067));
#57674=CARTESIAN_POINT('Ctrl Pts',(-0.249205287110151,-0.74417739182315,
-3.35543518141569));
#57675=CARTESIAN_POINT('Ctrl Pts',(0.136474276103288,-0.772837652800438,
-3.33958581112071));
#57676=CARTESIAN_POINT('Ctrl Pts',(0.489011498332319,-0.613816764289597,
-3.32373644082573));
#57677=CARTESIAN_POINT('Ctrl Pts',(0.722793843922638,-0.305732439907269,
-3.30788707053074));
#57678=CARTESIAN_POINT('Ctrl Pts',(0.781048018778739,0.0765980286034119,
-3.29203770023577));
#57679=CARTESIAN_POINT('Ctrl Pts',(0.649627183056744,0.4403269111216,-3.27618832994078));
#57680=CARTESIAN_POINT('Ctrl Pts',(0.360446465924673,0.697123813125427,
-3.2603389596458));
#57681=CARTESIAN_POINT('Ctrl Pts',(-0.0162675213692028,0.784626429183104,
-3.24448958935083));
#57682=CARTESIAN_POINT('Ctrl Pts',(-0.38903099318439,0.681585029153437,
-3.22864021905584));
#57683=CARTESIAN_POINT('Ctrl Pts',(-0.667319533915525,0.413022887112677,
-3.21279084876086));
#57684=CARTESIAN_POINT('Ctrl Pts',(-0.783551662478414,0.0441594593653245,
-3.19694147846588));
#57685=CARTESIAN_POINT('Ctrl Pts',(-0.709500778606978,-0.335427951697853,
-3.1810921081709));
#57686=CARTESIAN_POINT('Ctrl Pts',(-0.463149902351115,-0.633557758674201,
-3.16524273787593));
#57687=CARTESIAN_POINT('Ctrl Pts',(-0.104324555236145,-0.777830092500222,
-3.14939336758094));
#57688=CARTESIAN_POINT('Ctrl Pts',(0.27983567608852,-0.733208878841634,
-3.13354399728597));
#57689=CARTESIAN_POINT('Ctrl Pts',(0.596038709461116,-0.510530236565918,
-3.11769462699098));
#57690=CARTESIAN_POINT('Ctrl Pts',(0.767495650655195,-0.163870960970766,
-3.101845256696));
#57691=CARTESIAN_POINT('Ctrl Pts',(0.752568730477612,0.222583852809316,
-3.08599588640102));
#57692=CARTESIAN_POINT('Ctrl Pts',(0.554882903700043,0.554984890610126,
-3.07014651610604));
#57693=CARTESIAN_POINT('Ctrl Pts',(0.222445540399176,0.75260962469307,-3.05429714581105));
#57694=CARTESIAN_POINT('Ctrl Pts',(-0.164012010155015,0.767465521146739,
-3.03844777551608));
#57695=CARTESIAN_POINT('Ctrl Pts',(-0.510639769181497,0.595944873083403,
-3.02259840522109));
#57696=CARTESIAN_POINT('Ctrl Pts',(-0.733260295243549,0.279700920705432,
-3.00674903492612));
#57697=CARTESIAN_POINT('Ctrl Pts',(-0.777810906379899,-0.104467504711289,
-2.99089966463113));
#57698=CARTESIAN_POINT('Ctrl Pts',(-0.633472629319529,-0.463266331095978,
-2.97505029433616));
#57699=CARTESIAN_POINT('Ctrl Pts',(-0.335297552500043,-0.709562412273652,
-2.95920092404117));
#57700=CARTESIAN_POINT('Ctrl Pts',(0.0443034613785977,-0.78354353352829,
-2.9433515537462));
#57701=CARTESIAN_POINT('Ctrl Pts',(0.413145521513561,-0.667243616438114,
-2.92750218345121));
#57702=CARTESIAN_POINT('Ctrl Pts',(0.681656514570333,-0.388905723496004,
-2.91165281315624));
#57703=CARTESIAN_POINT('Ctrl Pts',(0.7846294056114,-0.0161233208125725,
-2.89580344286125));
#57704=CARTESIAN_POINT('Ctrl Pts',(0.697057557749046,0.36057457870607,-2.87995407256628));
#57705=CARTESIAN_POINT('Ctrl Pts',(0.440207513846546,0.649708096284145,
-2.86410470227129));
#57706=CARTESIAN_POINT('Ctrl Pts',(0.0764544846756664,0.781062082933939,
-2.84825533197632));
#57707=CARTESIAN_POINT('Ctrl Pts',(-0.305865271304502,0.722737643570575,
-2.83240596168133));
#57708=CARTESIAN_POINT('Ctrl Pts',(-0.613906625476715,0.488898681548557,
-2.81655659138636));
#57709=CARTESIAN_POINT('Ctrl Pts',(-0.772862721276039,0.136332240082525,
-2.80070722109137));
#57710=CARTESIAN_POINT('Ctrl Pts',(-0.744131579787873,-0.249342049375011,
-2.78485785079639));
#57711=CARTESIAN_POINT('Ctrl Pts',(-0.534690466730406,-0.574464420492465,
-2.76900848050141));
#57712=CARTESIAN_POINT('Ctrl Pts',(-0.195401485814985,-0.760079946430257,
-2.75315911020643));
#57713=CARTESIAN_POINT('Ctrl Pts',(0.191340120288431,-0.761112491023588,
-2.73730973991145));
#57714=CARTESIAN_POINT('Ctrl Pts',(0.531615390818176,-0.577311304124008,
-2.72146036961647));
#57715=CARTESIAN_POINT('Ctrl Pts',(0.742789565829382,-0.253311915470078,
-2.70561099932149));
#57716=CARTESIAN_POINT('Ctrl Pts',(0.773579673064216,0.132203460794283,
-2.68976162902651));
#57717=CARTESIAN_POINT('Ctrl Pts',(0.616508433565354,0.485613649897649,
-2.67391225873153));
#57718=CARTESIAN_POINT('Ctrl Pts',(0.309720094929824,0.721094118975316,
-2.65806288843655));
#57719=CARTESIAN_POINT('Ctrl Pts',(-0.0722827770885867,0.781459190079997,
-2.64221351814157));
#57720=CARTESIAN_POINT('Ctrl Pts',(-0.436732008128137,0.652049398972571,
-2.62636414784659));
#57721=CARTESIAN_POINT('Ctrl Pts',(-0.695122269335044,0.364291499075428,
-2.61051477755161));
#57722=CARTESIAN_POINT('Ctrl Pts',(-0.784704313096684,-0.0119334249730362,
-2.59466540725663));
#57723=CARTESIAN_POINT('Ctrl Pts',(-0.683723426911941,-0.385260354975586,
-2.57881603696165));
#57724=CARTESIAN_POINT('Ctrl Pts',(-0.41670249566724,-0.665028041310152,
-2.56296666666666));
#57725=CARTESIAN_POINT('Ctrl Pts',(-0.0484866975599475,-0.783295797118723,
-2.54711729637169));
#57726=CARTESIAN_POINT('Ctrl Pts',(0.331503939803658,-0.711342676576329,
-2.53126792607671));
#57727=CARTESIAN_POINT('Ctrl Pts',(0.630989906804924,-0.466642264625097,
-2.51541855578172));
#57728=CARTESIAN_POINT('Ctrl Pts',(0.777241995260494,-0.108619272818464,
-2.49956918548675));
#57729=CARTESIAN_POINT('Ctrl Pts',(0.734743353763132,0.275781561611777,
-2.48371981519176));
#57730=CARTESIAN_POINT('Ctrl Pts',(0.513814641327085,0.593209726810042,
-2.46787044489679));
#57731=CARTESIAN_POINT('Ctrl Pts',(0.168107688391456,0.766578809208684,
-2.4520210746018));
#57732=CARTESIAN_POINT('Ctrl Pts',(-0.218423678417938,0.753786682245382,
-2.43617170430682));
#57733=CARTESIAN_POINT('Ctrl Pts',(-0.551911554278842,0.557939872994966,
-2.42032233401184));
#57734=CARTESIAN_POINT('Ctrl Pts',(-0.751369476309632,0.226599152015872,
-2.40447296371687));
#57735=CARTESIAN_POINT('Ctrl Pts',(-0.768359726775325,-0.159770447498504,
-2.38862359342188));
#57736=CARTESIAN_POINT('Ctrl Pts',(-0.598756277750203,-0.507340305395548,
-2.3727742231269));
#57737=CARTESIAN_POINT('Ctrl Pts',(-0.28374678378875,-0.73170419454426,
-2.35692485283192));
#57738=CARTESIAN_POINT('Ctrl Pts',(0.100169708107077,-0.778376062839723,
-2.34107548253694));
#57739=CARTESIAN_POINT('Ctrl Pts',(0.459760307115391,-0.636021796501728,
-2.32522611224196));
#57740=CARTESIAN_POINT('Ctrl Pts',(0.707699587614688,-0.339211673316421,
-2.30937674194698));
#57741=CARTESIAN_POINT('Ctrl Pts',(0.783776289194928,0.039974918635952,
-2.293527371652));
#57742=CARTESIAN_POINT('Ctrl Pts',(0.669515428461959,0.409453729590444,
-2.27767800135702));
#57743=CARTESIAN_POINT('Ctrl Pts',(0.39266488960102,0.679498013314787,-2.26182863106204));
#57744=CARTESIAN_POINT('Ctrl Pts',(0.0204569395463645,0.784528380142186,
-2.24597926076706));
#57745=CARTESIAN_POINT('Ctrl Pts',(-0.356718912777502,0.699038541777891,
-2.23012989047208));
#57746=CARTESIAN_POINT('Ctrl Pts',(-0.647266719286364,0.443789431744821,
-2.2142805201771));
#57747=CARTESIAN_POINT('Ctrl Pts',(-0.780627875453987,0.0807674791504598,
-2.19843114988212));
#57748=CARTESIAN_POINT('Ctrl Pts',(-0.724416051504697,-0.301868597151919,
-2.18258177958714));
#57749=CARTESIAN_POINT('Ctrl Pts',(-0.492282108903929,-0.611196851167628,
-2.16673240929215));
#57750=CARTESIAN_POINT('Ctrl Pts',(-0.140599032359052,-0.772097906825179,
-2.15088303899718));
#57751=CARTESIAN_POINT('Ctrl Pts',(0.245228069020143,-0.745497457935825,
-2.13503366870219));
#57752=CARTESIAN_POINT('Ctrl Pts',(0.571502319016177,-0.537855338342251,
-2.11918429840722));
#57753=CARTESIAN_POINT('Ctrl Pts',(0.758989060691919,-0.199596771953163,
-2.10333492811223));
#57754=CARTESIAN_POINT('Ctrl Pts',(0.762157739131931,0.187133231429987,
-2.08748555781726));
#57755=CARTESIAN_POINT('Ctrl Pts',(0.580238850922621,0.528418528729,-2.07163618752227));
#57756=CARTESIAN_POINT('Ctrl Pts',(0.257410815592424,0.741379078232026,
-2.0557868172273));
#57757=CARTESIAN_POINT('Ctrl Pts',(-0.127928612118938,0.774298092355551,
-2.03993744693231));
#57758=CARTESIAN_POINT('Ctrl Pts',(-0.482200985982773,0.619181293920742,
-2.02408807663734));
#57759=CARTESIAN_POINT('Ctrl Pts',(-0.719372394325873,0.31369830077,-2.00823870634235));
#57760=CARTESIAN_POINT('Ctrl Pts',(-0.781846520014441,-0.0679653203143754,
-1.99238933604737));
#57761=CARTESIAN_POINT('Ctrl Pts',(-0.654451721656478,-0.433123780973749,
-1.97653996575239));
#57762=CARTESIAN_POINT('Ctrl Pts',(-0.368125418136845,-0.693099518211992,
-1.96069059545741));
#57763=CARTESIAN_POINT('Ctrl Pts',(0.00759896450262343,-0.784758256638701,
-1.94484122516243));
#57764=CARTESIAN_POINT('Ctrl Pts',(0.381477962943217,-0.685840965102565,
-1.92899185486745));
#57765=CARTESIAN_POINT('Ctrl Pts',(0.662716259510312,-0.42036939113687,
-1.91314248457247));
#57766=CARTESIAN_POINT('Ctrl Pts',(0.783016034359574,-0.0528124564845589,
-1.89729311427749));
#57767=CARTESIAN_POINT('Ctrl Pts',(0.713162872348176,0.327569814128564,
-1.88144374398251));
#57768=CARTESIAN_POINT('Ctrl Pts',(0.470120390212704,0.628402804203147,
-1.86559437368753));
#57769=CARTESIAN_POINT('Ctrl Pts',(0.112910676559248,0.776630185315416,
-1.84974500339255));
#57770=CARTESIAN_POINT('Ctrl Pts',(-0.271719033375929,0.736255412561006,
-1.83389563309757));
#57771=CARTESIAN_POINT('Ctrl Pts',(-0.590362646053683,0.517083370230197,
-1.81804626280259));
#57772=CARTESIAN_POINT('Ctrl Pts',(-0.765638580377628,0.172339287051596,
-1.8021968925076));
#57773=CARTESIAN_POINT('Ctrl Pts',(-0.754981636900799,-0.214256840186529,
-1.78634752221263));
#57774=CARTESIAN_POINT('Ctrl Pts',(-0.560979820224823,-0.548821379799159,
-1.77049815191765));
#57775=CARTESIAN_POINT('Ctrl Pts',(-0.23074585036879,-0.750106404559852,
-1.75464878162267));
#57776=CARTESIAN_POINT('Ctrl Pts',(0.155524010440509,-0.76923049068574,
-1.73879941132768));
#57777=CARTESIAN_POINT('Ctrl Pts',(0.504025363275639,-0.601549415093211,
-1.72295004103271));
#57778=CARTESIAN_POINT('Ctrl Pts',(0.730125770442385,-0.287783990103754,
-1.70710067073772));
#57779=CARTESIAN_POINT('Ctrl Pts',(0.77891747199518,0.0958688554472317,
-1.69125130044275));
#57780=CARTESIAN_POINT('Ctrl Pts',(0.638551559434616,0.456240256408558,
-1.67540193014776));
#57781=CARTESIAN_POINT('Ctrl Pts',(0.34311544519835,0.705815171904418,-1.65955255985279));
#57782=CARTESIAN_POINT('Ctrl Pts',(-0.0356451563072939,0.783985132802881,
-1.6437031895578));
#57783=CARTESIAN_POINT('Ctrl Pts',(-0.405749445733414,0.671766814386624,
-1.62785381926282));
#57784=CARTESIAN_POINT('Ctrl Pts',(-0.677318781403579,0.396412075979144,
-1.61200444896784));
#57785=CARTESIAN_POINT('Ctrl Pts',(-0.784403419668906,0.0247899341638738,
-1.59615507867286));
#57786=CARTESIAN_POINT('Ctrl Pts',(-0.700998198993379,-0.352852363789961,
-1.58030570837788));
#57787=CARTESIAN_POINT('Ctrl Pts',(-0.447357810168782,-0.644805594970389,
-1.5644563380829));
#57788=CARTESIAN_POINT('Ctrl Pts',(-0.0850780095079747,-0.780169851969611,
-1.54860696778792));
#57789=CARTESIAN_POINT('Ctrl Pts',(0.297862713356593,-0.726072358388593,
-1.53275759749294));
#57790=CARTESIAN_POINT('Ctrl Pts',(0.608468429988034,-0.495650517332548,
-1.51690822719796));
#57791=CARTESIAN_POINT('Ctrl Pts',(0.771309536608839,-0.144861535130568,
-1.50105885690298));
#57792=CARTESIAN_POINT('Ctrl Pts',(0.746840591865543,0.24110660705598,-1.485209486608));
#57793=CARTESIAN_POINT('Ctrl Pts',(0.541003800643689,0.568522781701145,
-1.46936011631302));
#57794=CARTESIAN_POINT('Ctrl Pts',(0.203785968637258,0.757875019123007,
-1.45351074601804));
#57795=CARTESIAN_POINT('Ctrl Pts',(-0.182920633364878,0.763179734737182,
-1.43766137572306));
#57796=CARTESIAN_POINT('Ctrl Pts',(-0.525205545234974,0.583148695341557,
-1.42181200542808));
#57797=CARTESIAN_POINT('Ctrl Pts',(-0.739945972063181,0.261501862424725,
-1.4059626351331));
#57798=CARTESIAN_POINT('Ctrl Pts',(-0.774992888756427,-0.123649860497661,
-1.39011326483812));
#57799=CARTESIAN_POINT('Ctrl Pts',(-0.621835263810005,-0.478773610703918,
-1.37426389454314));
#57800=CARTESIAN_POINT('Ctrl Pts',(-0.317666936057598,-0.717628722502035,
-1.35841452424816));
#57801=CARTESIAN_POINT('Ctrl Pts',(0.0636457900011377,-0.782209996765098,
-1.34256515395318));
#57802=CARTESIAN_POINT('Ctrl Pts',(0.429502339741044,-0.656834077816532,
-1.3267157836582));
#57803=CARTESIAN_POINT('Ctrl Pts',(0.691055621467951,-0.371948106140721,
-1.31086641336322));
#57804=CARTESIAN_POINT('Ctrl Pts',(0.784788258163402,0.00326427219707354,
-1.29501704306824));
#57805=CARTESIAN_POINT('Ctrl Pts',(0.687937579121799,0.377683932483451,
-1.27916767277326));
#57806=CARTESIAN_POINT('Ctrl Pts',(0.424023461649061,0.660384259045651,
-1.26331830247827));
#57807=CARTESIAN_POINT('Ctrl Pts',(0.0571366041655278,0.782712382736185,
-1.2474689321833));
#57808=CARTESIAN_POINT('Ctrl Pts',(-0.323625694697954,0.714961310390562,
-1.23161956188831));
#57809=CARTESIAN_POINT('Ctrl Pts',(-0.625796529798224,0.473584173000561,
-1.21577019159333));
#57810=CARTESIAN_POINT('Ctrl Pts',(-0.775994681330568,0.117198635532986,
-1.19992082129835));
#57811=CARTESIAN_POINT('Ctrl Pts',(-0.73774500910418,-0.267648215323767,
-1.18407145100337));
#57812=CARTESIAN_POINT('Ctrl Pts',(-0.520336323550321,-0.587497554053001,
-1.16822208070839));
#57813=CARTESIAN_POINT('Ctrl Pts',(-0.176565627850278,-0.764674992847263,
-1.15237271041341));
#57814=CARTESIAN_POINT('Ctrl Pts',(0.210083465240229,-0.756153557987252,
-1.13652334011843));
#57815=CARTESIAN_POINT('Ctrl Pts',(0.545714461448512,-0.564002652644547,
-1.12067396982345));
#57816=CARTESIAN_POINT('Ctrl Pts',(0.748820447978499,-0.234885508947245,
-1.10482459952847));
#57817=CARTESIAN_POINT('Ctrl Pts',(0.770077786312045,0.151272828534624,
-1.08897522923349));
#57818=CARTESIAN_POINT('Ctrl Pts',(0.604324199897217,0.50069504395661,-1.07312585893851));
#57819=CARTESIAN_POINT('Ctrl Pts',(0.291812416480199,0.72852507109372,-1.05727648864353));
#57820=CARTESIAN_POINT('Ctrl Pts',(-0.091565077945533,0.779435117328539,
-1.04142711834855));
#57821=CARTESIAN_POINT('Ctrl Pts',(-0.452706286367931,0.641061840938205,
-1.02557774805357));
#57822=CARTESIAN_POINT('Ctrl Pts',(-0.703909222634067,0.34700874904652,
-1.00972837775859));
#57823=CARTESIAN_POINT('Ctrl Pts',(-0.784170057980586,-0.0313143064883875,
-0.993879007463609));
#57824=CARTESIAN_POINT('Ctrl Pts',(-0.673997705525074,-0.402032782955643,
-0.978029637168627));
#57825=CARTESIAN_POINT('Ctrl Pts',(-0.400147168308302,-0.675118885322409,
-0.962180266873648));
#57826=CARTESIAN_POINT('Ctrl Pts',(-0.0291221724707292,-0.784254528003958,
-0.946330896578668));
#57827=CARTESIAN_POINT('Ctrl Pts',(0.348975049707139,-0.702936469608757,
-0.930481526283687));
#57828=CARTESIAN_POINT('Ctrl Pts',(0.642324798422119,-0.450912540251555,
-0.914632155988707));
#57829=CARTESIAN_POINT('Ctrl Pts',(0.779688026454552,-0.0893859442391789,
-0.898782785693727));
#57830=CARTESIAN_POINT('Ctrl Pts',(0.727706513690353,0.293847742133158,
-0.882933415398745));
#57831=CARTESIAN_POINT('Ctrl Pts',(0.499003804068385,0.605721445178727,
-0.867084045103767));
#57832=CARTESIAN_POINT('Ctrl Pts',(0.149119618353334,0.770497634679226,
-0.851234674808784));
#57833=CARTESIAN_POINT('Ctrl Pts',(-0.236977789223283,0.748160940599662,
-0.835385304513805));
#57834=CARTESIAN_POINT('Ctrl Pts',(-0.565525899449417,0.54413575757898,
-0.819535934218824));
#57835=CARTESIAN_POINT('Ctrl Pts',(-0.756737855711574,0.20796894805998,
-0.803686563923844));
#57836=CARTESIAN_POINT('Ctrl Pts',(-0.764178446659503,-0.178702454614348,
-0.787837193628863));
#57837=CARTESIAN_POINT('Ctrl Pts',(-0.586040748605003,-0.521976538360308,
-0.771987823333882));
#57838=CARTESIAN_POINT('Ctrl Pts',(-0.265584931154134,-0.73849029104517,
-0.756138453038903));
#57839=CARTESIAN_POINT('Ctrl Pts',(0.119367336469941,-0.775664041069455,
-0.740289082743921));
#57840=CARTESIAN_POINT('Ctrl Pts',(0.475331628626109,-0.624470262263764,
-0.724439712448942));
#57841=CARTESIAN_POINT('Ctrl Pts',(0.715863156701094,-0.321625879714412,
-0.708590342153962));
#57842=CARTESIAN_POINT('Ctrl Pts',(0.782549609242745,0.0593243179324704,
-0.692740971858981));
#57843=CARTESIAN_POINT('Ctrl Pts',(0.659196394769945,0.425867794915784,
-0.676891601564001));
#57844=CARTESIAN_POINT('Ctrl Pts',(0.375759446461501,0.688990641459715,
-0.66104223126902));
#57845=CARTESIAN_POINT('Ctrl Pts',(0.0010705196974362,0.78479431675548,
-0.64519286097404));
#57846=CARTESIAN_POINT('Ctrl Pts',(-0.373878379347529,0.690013205004504,
-0.629343490679059));
#57847=CARTESIAN_POINT('Ctrl Pts',(-0.658032111062648,0.427664595722584,
-0.613494120384079));
#57848=CARTESIAN_POINT('Ctrl Pts',(-0.782384851512599,0.0614590086783985,
-0.597644750089098));
#57849=CARTESIAN_POINT('Ctrl Pts',(-0.716737935835347,-0.319671701842087,
-0.581795379794119));
#57850=CARTESIAN_POINT('Ctrl Pts',(-0.477033507312882,-0.623171163104398,
-0.565946009499137));
#57851=CARTESIAN_POINT('Ctrl Pts',(-0.121483018919316,-0.775335502694393,
-0.550096639204157));
#57852=CARTESIAN_POINT('Ctrl Pts',(0.263569231651014,-0.739212097946903,
-0.534247268909177));
#57853=CARTESIAN_POINT('Ctrl Pts',(0.58461453821839,-0.523573402043788,
-0.518397898614196));
#57854=CARTESIAN_POINT('Ctrl Pts',(0.763688076015605,-0.180786581847057,
-0.502548528319217));
#57855=CARTESIAN_POINT('Ctrl Pts',(0.757302409750591,0.205903680903747,
-0.486699158024236));
#57856=CARTESIAN_POINT('Ctrl Pts',(0.567008278031727,0.542590894014966,
-0.470849787729256));
#57857=CARTESIAN_POINT('Ctrl Pts',(0.239018001454253,0.747511645799011,
-0.455000417434275));
#57858=CARTESIAN_POINT('Ctrl Pts',(-0.147017031477197,0.770901587803361,
-0.439151047139295));
#57859=CARTESIAN_POINT('Ctrl Pts',(-0.497349449046418,0.607080547508727,
-0.423301676844315));
#57860=CARTESIAN_POINT('Ctrl Pts',(-0.726902145325857,0.295831940012187,
-0.407452306549334));
#57861=CARTESIAN_POINT('Ctrl Pts',(-0.779928983062327,-0.0872585068980811,
-0.391602936254354));
#57862=CARTESIAN_POINT('Ctrl Pts',(-0.643552564396997,-0.449158504824145,
-0.375753565959373));
#57863=CARTESIAN_POINT('Ctrl Pts',(-0.350891466139449,-0.701981797925372,
-0.359904195664393));
#57864=CARTESIAN_POINT('Ctrl Pts',(0.0269825014226717,-0.784331059137986,
-0.344054825369413));
#57865=CARTESIAN_POINT('Ctrl Pts',(0.398303854423826,-0.676208033714155,
-0.328205455074432));
#57866=CARTESIAN_POINT('Ctrl Pts',(0.672898392626291,-0.403870052833872,
-0.312356084779451));
#57867=CARTESIAN_POINT('Ctrl Pts',(0.784081708830621,-0.0334535219070024,
-0.296506714484472));
#57868=CARTESIAN_POINT('Ctrl Pts',(0.704853296171943,0.345087088060326,
-0.28065734418949));
#57869=CARTESIAN_POINT('Ctrl Pts',(0.454453510249238,0.639824406817222,
-0.26480797389451));
#57870=CARTESIAN_POINT('Ctrl Pts',(0.0936911583621272,0.779182410692385,
-0.24895860359953));
#57871=CARTESIAN_POINT('Ctrl Pts',(-0.289823818597269,0.729318473263532,
-0.23310923330455));
#57872=CARTESIAN_POINT('Ctrl Pts',(-0.602955955831871,0.502341855628342,
-0.217259863009569));
#57873=CARTESIAN_POINT('Ctrl Pts',(-0.769662274193841,0.15337317400364,
-0.201410492714589));
#57874=CARTESIAN_POINT('Ctrl Pts',(-0.749458369122514,-0.232841784334449,
-0.185561122419608));
#57875=CARTESIAN_POINT('Ctrl Pts',(-0.547251299066349,-0.562511679805382,
-0.169711752124628));
#57876=CARTESIAN_POINT('Ctrl Pts',(-0.212145219487114,-0.755577769385975,
-0.153862381829647));
#57877=CARTESIAN_POINT('Ctrl Pts',(0.174478112953526,-0.765153522886825,
-0.138013011534667));
#57878=CARTESIAN_POINT('Ctrl Pts',(0.518732998477949,-0.588915552014349,
-0.122163641239687));
#57879=CARTESIAN_POINT('Ctrl Pts',(0.737009354389205,-0.269658664549011,
-0.106314270944705));
#57880=CARTESIAN_POINT('Ctrl Pts',(0.776316866393766,0.115078755729171,
-0.090464900649726));
#57881=CARTESIAN_POINT('Ctrl Pts',(0.627075735706326,0.471879890555984,
-0.0746155303547465));
#57882=CARTESIAN_POINT('Ctrl Pts',(0.325595766972002,0.714066267041671,
-0.0587661600597641));
#57883=CARTESIAN_POINT('Ctrl Pts',(-0.0550443924619386,0.782885992515902,
-0.0429167897647847));
#57884=CARTESIAN_POINT('Ctrl Pts',(-0.299751230468417,0.701944631018955,
-0.0323505429014654));
#57885=CARTESIAN_POINT('Ctrl Pts',(-0.405096567646243,0.634709045147731,
-0.0270674194698051));
#57886=CARTESIAN_POINT('Ctrl Pts',(-0.342067962509734,0.713322310757514,
-3.8089));
#57887=CARTESIAN_POINT('Ctrl Pts',(-0.460461074940839,0.656547848310817,
-3.80361687656834));
#57888=CARTESIAN_POINT('Ctrl Pts',(-0.668315725953181,0.482971786953477,
-3.79305062970501));
#57889=CARTESIAN_POINT('Ctrl Pts',(-0.817818597191245,0.105068633983768,
-3.77720125941004));
#57890=CARTESIAN_POINT('Ctrl Pts',(-0.768704339632432,-0.298246190578182,
-3.76135188911506));
#57891=CARTESIAN_POINT('Ctrl Pts',(-0.532919287701208,-0.629183815996688,
-3.74550251882008));
#57892=CARTESIAN_POINT('Ctrl Pts',(-0.16771310606437,-0.807300348800163,
-3.7296531485251));
#57893=CARTESIAN_POINT('Ctrl Pts',(0.238219934613418,-0.789379745338913,
-3.71380377823012));
#57894=CARTESIAN_POINT('Ctrl Pts',(0.586302911621603,-0.579754073688803,
-3.69795440793514));
#57895=CARTESIAN_POINT('Ctrl Pts',(0.792003651881398,-0.229340416056228,
-3.68210503764016));
#57896=CARTESIAN_POINT('Ctrl Pts',(0.805369071963743,0.176769581565368,
-3.66625566734517));
#57897=CARTESIAN_POINT('Ctrl Pts',(0.623153073676116,0.53995075626169,-3.6504062970502));
#57898=CARTESIAN_POINT('Ctrl Pts',(0.289606406895025,0.772007076297564,
-3.63455692675521));
#57899=CARTESIAN_POINT('Ctrl Pts',(-0.11427027928863,0.816583715924684,
-3.61870755646024));
#57900=CARTESIAN_POINT('Ctrl Pts',(-0.490396778310394,0.662855734101919,
-3.60285818616526));
#57901=CARTESIAN_POINT('Ctrl Pts',(-0.747431997910723,0.348155298616472,
-3.58700881587027));
#57902=CARTESIAN_POINT('Ctrl Pts',(-0.82295574586927,-0.0510935052537138,
-3.5711594455753));
#57903=CARTESIAN_POINT('Ctrl Pts',(-0.698627328000686,-0.437934430876563,
-3.55531007528031));
#57904=CARTESIAN_POINT('Ctrl Pts',(-0.404639499343168,-0.71842437402542,
-3.53946070498534));
#57905=CARTESIAN_POINT('Ctrl Pts',(-0.0123862644028858,-0.824447262365292,
-3.52361133469035));
#57906=CARTESIAN_POINT('Ctrl Pts',(0.382874935467909,-0.730255770658821,
-3.50776196439537));
#57907=CARTESIAN_POINT('Ctrl Pts',(0.68515618301796,-0.458724004285021,
-3.49191259410039));
#57908=CARTESIAN_POINT('Ctrl Pts',(0.821049445347924,-0.0757925816733543,
-3.47606322380541));
#57909=CARTESIAN_POINT('Ctrl Pts',(0.75755347869802,0.325544826440259,-3.46021385351043));
#57910=CARTESIAN_POINT('Ctrl Pts',(0.510088075322107,0.647824715936081,
-3.44436448321545));
#57911=CARTESIAN_POINT('Ctrl Pts',(0.138749416059389,0.812782447317181,
-3.42851511292047));
#57912=CARTESIAN_POINT('Ctrl Pts',(-0.26628409463647,0.780358563795485,
-3.41266574262549));
#57913=CARTESIAN_POINT('Ctrl Pts',(-0.606651365548571,0.558427101611629,
-3.39681637233051));
#57914=CARTESIAN_POINT('Ctrl Pts',(-0.799695294729937,0.200883405799385,
-3.38096700203553));
#57915=CARTESIAN_POINT('Ctrl Pts',(-0.798535782074509,-0.205444181921911,
-3.36511763174055));
#57916=CARTESIAN_POINT('Ctrl Pts',(-0.603454411517097,-0.561880307858081,
-3.34926826144557));
#57917=CARTESIAN_POINT('Ctrl Pts',(-0.261826069280859,-0.781865600076974,
-3.33341889115059));
#57918=CARTESIAN_POINT('Ctrl Pts',(0.143385895557981,-0.81197733471658,
-3.31756952085561));
#57919=CARTESIAN_POINT('Ctrl Pts',(0.513777054757662,-0.64490297343331,
-3.30172015056063));
#57920=CARTESIAN_POINT('Ctrl Pts',(0.759399101235821,-0.321215989920727,
-3.28587078026565));
#57921=CARTESIAN_POINT('Ctrl Pts',(0.82060350744503,0.0804772682652918,
-3.27002140997067));
#57922=CARTESIAN_POINT('Ctrl Pts',(0.682526979303457,0.462626879527595,
-3.25417203967569));
#57923=CARTESIAN_POINT('Ctrl Pts',(0.378700959572816,0.73242903434883,-3.23832266938071));
#57924=CARTESIAN_POINT('Ctrl Pts',(-0.017091375654309,0.824363143291098,
-3.22247329908572));
#57925=CARTESIAN_POINT('Ctrl Pts',(-0.408733125027448,0.716103302355065,
-3.20662392879075));
#57926=CARTESIAN_POINT('Ctrl Pts',(-0.70111534368131,0.433940067282538,
-3.19077455849577));
#57927=CARTESIAN_POINT('Ctrl Pts',(-0.823233945973712,0.0463958762724045,
-3.17492518820078));
#57928=CARTESIAN_POINT('Ctrl Pts',(-0.745432820340849,-0.352415404738813,
-3.15907581790581));
#57929=CARTESIAN_POINT('Ctrl Pts',(-0.486605721036748,-0.665643733083127,
-3.14322644761082));
#57930=CARTESIAN_POINT('Ctrl Pts',(-0.109607980407257,-0.817222612125714,
-3.12737707731585));
#57931=CARTESIAN_POINT('Ctrl Pts',(0.294007707318109,-0.77034159642076,
-3.11152770702086));
#57932=CARTESIAN_POINT('Ctrl Pts',(0.626224564683723,-0.536385590527203,
-3.09567833672589));
#57933=CARTESIAN_POINT('Ctrl Pts',(0.80636479157996,-0.172170061389141,
-3.0798289664309));
#57934=CARTESIAN_POINT('Ctrl Pts',(0.790681910683307,0.233856415898155,
-3.06397959613592));
#57935=CARTESIAN_POINT('Ctrl Pts',(0.582984459405604,0.583091611352872,
-3.04813022584094));
#57936=CARTESIAN_POINT('Ctrl Pts',(0.233711098777889,0.790724875950268,
-3.03228085554596));
#57937=CARTESIAN_POINT('Ctrl Pts',(-0.172318253885027,0.8063331361891,-3.01643148525098));
#57938=CARTESIAN_POINT('Ctrl Pts',(-0.536500670325573,0.626125976045352,
-3.000582114956));
#57939=CARTESIAN_POINT('Ctrl Pts',(-0.77039561676104,0.293866127367396,
-2.98473274466102));
#57940=CARTESIAN_POINT('Ctrl Pts',(-0.817202454341236,-0.109758169432597,
-2.96888337436604));
#57941=CARTESIAN_POINT('Ctrl Pts',(-0.665554292427307,-0.486728046212792,
-2.95303400407106));
#57942=CARTESIAN_POINT('Ctrl Pts',(-0.352278401588544,-0.745497575390258,
-2.93718463377608));
#57943=CARTESIAN_POINT('Ctrl Pts',(0.0465471711407394,-0.823225405340074,
-2.9213352634811));
#57944=CARTESIAN_POINT('Ctrl Pts',(0.434068912394584,-0.701035581430156,
-2.90548589318612));
#57945=CARTESIAN_POINT('Ctrl Pts',(0.716178408087904,-0.408601511166088,
-2.88963652289114));
#57946=CARTESIAN_POINT('Ctrl Pts',(0.824366270457982,-0.0169398721875644,
-2.87378715259615));
#57947=CARTESIAN_POINT('Ctrl Pts',(0.732359423527299,0.37883556051313,-2.85793778230118));
#57948=CARTESIAN_POINT('Ctrl Pts',(0.462501435482764,0.682611990309953,
-2.84208841200619));
#57949=CARTESIAN_POINT('Ctrl Pts',(0.0803264546818227,0.820618283866978,
-2.82623904171122));
#57950=CARTESIAN_POINT('Ctrl Pts',(-0.321355548447016,0.759340054666452,
-2.81038967141623));
#57951=CARTESIAN_POINT('Ctrl Pts',(-0.64499738556106,0.513658524467306,
-2.79454030112126));
#57952=CARTESIAN_POINT('Ctrl Pts',(-0.812003672763037,0.143236666248114,
-2.77869093082627));
#57953=CARTESIAN_POINT('Ctrl Pts',(-0.781817467931542,-0.261969757750101,
-2.7628415605313));
#57954=CARTESIAN_POINT('Ctrl Pts',(-0.561769394258834,-0.603557664861111,
-2.74699219023631));
#57955=CARTESIAN_POINT('Ctrl Pts',(-0.205297421879992,-0.798573525549128,
-2.73114281994133));
#57956=CARTESIAN_POINT('Ctrl Pts',(0.201030372075136,-0.799658362453533,
-2.71529344964635));
#57957=CARTESIAN_POINT('Ctrl Pts',(0.558538583836721,-0.606548726405558,
-2.69944407935137));
#57958=CARTESIAN_POINT('Ctrl Pts',(0.78040748885868,-0.26614067421539,-2.68359470905639));
#57959=CARTESIAN_POINT('Ctrl Pts',(0.812756933942761,0.138898788571012,
-2.66774533876141));
#57960=CARTESIAN_POINT('Ctrl Pts',(0.647730959927692,0.51020712528314,-2.65189596846643));
#57961=CARTESIAN_POINT('Ctrl Pts',(0.325405596218053,0.757613295216305,
-2.63604659817145));
#57962=CARTESIAN_POINT('Ctrl Pts',(-0.075943474640016,0.821035502154527,
-2.62019722787647));
#57963=CARTESIAN_POINT('Ctrl Pts',(-0.458849915839789,0.685071866209927,
-2.60434785758149));
#57964=CARTESIAN_POINT('Ctrl Pts',(-0.730326124136905,0.382740721039322,
-2.58849848728651));
#57965=CARTESIAN_POINT('Ctrl Pts',(-0.82444497156685,-0.0125377827652834,
-2.57264911699154));
#57966=CARTESIAN_POINT('Ctrl Pts',(-0.718349997383733,-0.404771526169174,
-2.55679974669655));
#57967=CARTESIAN_POINT('Ctrl Pts',(-0.437806026369945,-0.698707800452159,
-2.54095037640157));
#57968=CARTESIAN_POINT('Ctrl Pts',(-0.0509422636323139,-0.822965122538343,
-2.52510100610659));
#57969=CARTESIAN_POINT('Ctrl Pts',(0.348292664720002,-0.747367999609815,
-2.50925163581161));
#57970=CARTESIAN_POINT('Ctrl Pts',(0.662945834618673,-0.49027495092069,
-2.49340226551663));
#57971=CARTESIAN_POINT('Ctrl Pts',(0.816604731219499,-0.114120200177109,
-2.47755289522165));
#57972=CARTESIAN_POINT('Ctrl Pts',(0.771953783472506,0.2897482757861,-2.46170352492666));
#57973=CARTESIAN_POINT('Ctrl Pts',(0.539836331073344,0.62325231069913,-2.44585415463169));
#57974=CARTESIAN_POINT('Ctrl Pts',(0.176621354136727,0.805401517506294,
-2.43000478433671));
#57975=CARTESIAN_POINT('Ctrl Pts',(-0.229485553140592,0.791961544545119,
-2.41415541404173));
#57976=CARTESIAN_POINT('Ctrl Pts',(-0.579862628611256,0.586196246216725,
-2.39830604374674));
#57977=CARTESIAN_POINT('Ctrl Pts',(-0.789421921344748,0.238075066394829,
-2.38245667345177));
#57978=CARTESIAN_POINT('Ctrl Pts',(-0.807272628073788,-0.167861881025363,
-2.36660730315678));
#57979=CARTESIAN_POINT('Ctrl Pts',(-0.629079761824146,-0.53303410810361,
-2.35075793286181));
#57980=CARTESIAN_POINT('Ctrl Pts',(-0.29811688962143,-0.768760708713042,
-2.33490856256682));
#57981=CARTESIAN_POINT('Ctrl Pts',(0.105242714706501,-0.817796232651961,
-2.31905919227185));
#57982=CARTESIAN_POINT('Ctrl Pts',(0.483044462737151,-0.668232559935171,
-2.30320982197686));
#57983=CARTESIAN_POINT('Ctrl Pts',(0.743540409617926,-0.356390749604617,
-2.28736045168189));
#57984=CARTESIAN_POINT('Ctrl Pts',(0.823469948712349,0.0419994131651224,
-2.2715110813869));
#57985=CARTESIAN_POINT('Ctrl Pts',(0.703422447372071,0.430190152922657,
-2.25566171109193));
#57986=CARTESIAN_POINT('Ctrl Pts',(0.412551056925986,0.713910591438302,
-2.23981234079694));
#57987=CARTESIAN_POINT('Ctrl Pts',(0.0214929632234256,0.824260128642901,
-2.22396297050196));
#57988=CARTESIAN_POINT('Ctrl Pts',(-0.374784627781147,0.73444073274668,
-2.20811360020698));
#57989=CARTESIAN_POINT('Ctrl Pts',(-0.680046971925417,0.466264756456678,
-2.192264229912));
#57990=CARTESIAN_POINT('Ctrl Pts',(-0.820162086331818,0.084857876961263,
-2.17641485961702));
#57991=CARTESIAN_POINT('Ctrl Pts',(-0.761103464091417,-0.31715646625377,
-2.16056548932204));
#57992=CARTESIAN_POINT('Ctrl Pts',(-0.517213302519679,-0.642150377119893,
-2.14471611902706));
#57993=CARTESIAN_POINT('Ctrl Pts',(-0.147719546459669,-0.811200124958251,
-2.12886674873208));
#57994=CARTESIAN_POINT('Ctrl Pts',(0.257647428485322,-0.783252519774712,
-2.1130173784371));
#57995=CARTESIAN_POINT('Ctrl Pts',(0.600445550365703,-0.565094548004635,
-2.09716800814212));
#57996=CARTESIAN_POINT('Ctrl Pts',(0.79742739286384,-0.209705174587831,
-2.08131863784714));
#57997=CARTESIAN_POINT('Ctrl Pts',(0.80075654623127,0.196610429037486,-2.06546926755216));
#57998=CARTESIAN_POINT('Ctrl Pts',(0.609624536232087,0.555179819484054,
-2.04961989725718));
#57999=CARTESIAN_POINT('Ctrl Pts',(0.270447159522559,0.778925568359848,
-2.0337705269622));
#58000=CARTESIAN_POINT('Ctrl Pts',(-0.134407443951421,0.813511736946051,
-2.01792115666722));
#58001=CARTESIAN_POINT('Ctrl Pts',(-0.506621630011469,0.650539184940502,
-2.00207178637223));
#58002=CARTESIAN_POINT('Ctrl Pts',(-0.755804375339143,0.329585274787486,
-1.98622241607726));
#58003=CARTESIAN_POINT('Ctrl Pts',(-0.821442448072192,-0.0714073640719366,
-1.97037304578228));
#58004=CARTESIAN_POINT('Ctrl Pts',(-0.687595852409281,-0.455058953200669,
-1.9545236754873));
#58005=CARTESIAN_POINT('Ctrl Pts',(-0.386768805553227,-0.728200932565636,
-1.93867430519231));
#58006=CARTESIAN_POINT('Ctrl Pts',(0.00798380736379087,-0.82450164703202,
-1.92282493489733));
#58007=CARTESIAN_POINT('Ctrl Pts',(0.400797578225299,-0.720574776430087,
-1.90697556460235));
#58008=CARTESIAN_POINT('Ctrl Pts',(0.696278940500164,-0.441658628529436,
-1.89112619430737));
#58009=CARTESIAN_POINT('Ctrl Pts',(0.822671191440778,-0.055487096805885,
-1.8752768240124));
#58010=CARTESIAN_POINT('Ctrl Pts',(0.749280377592604,0.34415929871677,-1.85942745371741));
#58011=CARTESIAN_POINT('Ctrl Pts',(0.493929223113824,0.660227710485335,
-1.84357808342243));
#58012=CARTESIAN_POINT('Ctrl Pts',(0.118628938278841,0.81596193669887,-1.82772871312745));
#58013=CARTESIAN_POINT('Ctrl Pts',(-0.28548000438757,0.773542419155801,
-1.81187934283247));
#58014=CARTESIAN_POINT('Ctrl Pts',(-0.62026104204666,0.543270601871413,
-1.79602997253749));
#58015=CARTESIAN_POINT('Ctrl Pts',(-0.804413671614601,0.181067258382205,
-1.78018060224251));
#58016=CARTESIAN_POINT('Ctrl Pts',(-0.793217016626087,-0.225107689058692,
-1.76433123194753));
#58017=CARTESIAN_POINT('Ctrl Pts',(-0.589390148895294,-0.576615954968053,
-1.74848186165255));
#58018=CARTESIAN_POINT('Ctrl Pts',(-0.242431770631838,-0.788094882439194,
-1.73263249135757));
#58019=CARTESIAN_POINT('Ctrl Pts',(0.163400386904445,-0.808187491055145,
-1.71678312106259));
#58020=CARTESIAN_POINT('Ctrl Pts',(0.529551283661103,-0.632014355146631,
-1.70093375076761));
#58021=CARTESIAN_POINT('Ctrl Pts',(0.767102346713403,-0.302358556692748,
-1.68508438047263));
#58022=CARTESIAN_POINT('Ctrl Pts',(0.818365060997018,0.100724049153528,
-1.66923501017765));
#58023=CARTESIAN_POINT('Ctrl Pts',(0.670890440482616,0.479346142164072,
-1.65338563988267));
#58024=CARTESIAN_POINT('Ctrl Pts',(0.360492224573578,0.741560559334522,
-1.63753626958769));
#58025=CARTESIAN_POINT('Ctrl Pts',(-0.037450373838634,0.823689369020797,
-1.62168689929271));
#58026=CARTESIAN_POINT('Ctrl Pts',(-0.426298268873834,0.705787852753012,
-1.60583752899773));
#58027=CARTESIAN_POINT('Ctrl Pts',(-0.711620994247248,0.416488016256281,
-1.58998815870274));
#58028=CARTESIAN_POINT('Ctrl Pts',(-0.824128839656565,0.0260453985351858,
-1.57413878840777));
#58029=CARTESIAN_POINT('Ctrl Pts',(-0.736499635075034,-0.370722260827263,
-1.55828941811278));
#58030=CARTESIAN_POINT('Ctrl Pts',(-0.470013852261533,-0.677461206137155,
-1.54244004781781));
#58031=CARTESIAN_POINT('Ctrl Pts',(-0.0893867103303759,-0.819680866651678,
-1.52659067752282));
#58032=CARTESIAN_POINT('Ctrl Pts',(0.312947708003538,-0.762843653177941,
-1.51074130722784));
#58033=CARTESIAN_POINT('Ctrl Pts',(0.639283777453891,-0.520752301024987,
-1.49489193693286));
#58034=CARTESIAN_POINT('Ctrl Pts',(0.810371828427002,-0.152197919928012,
-1.47904256663788));
#58035=CARTESIAN_POINT('Ctrl Pts',(0.784663675538757,0.25331723871174,-1.4631931963429));
#58036=CARTESIAN_POINT('Ctrl Pts',(0.568402461404965,0.597315117008862,
-1.44734382604792));
#58037=CARTESIAN_POINT('Ctrl Pts',(0.214106529446551,0.796256931641343,
-1.43149445575294));
#58038=CARTESIAN_POINT('Ctrl Pts',(-0.192184487655432,0.801830299903386,
-1.41564508545796));
#58039=CARTESIAN_POINT('Ctrl Pts',(-0.551804117272192,0.612681747157521,
-1.39979571516298));
#58040=CARTESIAN_POINT('Ctrl Pts',(-0.77741988379191,0.274745393816729,
-1.383946344868));
#58041=CARTESIAN_POINT('Ctrl Pts',(-0.814241720698406,-0.12991199872464,
-1.36809697457302));
#58042=CARTESIAN_POINT('Ctrl Pts',(-0.65332756279618,-0.503020678331755,
-1.35224760427804));
#58043=CARTESIAN_POINT('Ctrl Pts',(-0.333754898112137,-0.753972396792277,
-1.33639823398306));
#58044=CARTESIAN_POINT('Ctrl Pts',(0.0668690749522735,-0.821824332782597,
-1.32054886368808));
#58045=CARTESIAN_POINT('Ctrl Pts',(0.451254107267879,-0.690098860897773,
-1.3046994933931));
#58046=CARTESIAN_POINT('Ctrl Pts',(0.726053524472037,-0.390785090222578,
-1.28885012309812));
#58047=CARTESIAN_POINT('Ctrl Pts',(0.824533167957502,0.00342958838607511,
-1.27300075280314));
#58048=CARTESIAN_POINT('Ctrl Pts',(0.722777571618828,0.396811402436126,
-1.25715138250816));
#58049=CARTESIAN_POINT('Ctrl Pts',(0.445497756222818,0.693828837926884,
-1.24130201221318));
#58050=CARTESIAN_POINT('Ctrl Pts',(0.0600302371357995,0.822352161648496,
-1.2254526419182));
#58051=CARTESIAN_POINT('Ctrl Pts',(-0.34001543283308,0.751169895944896,
-1.20960327162322));
#58052=CARTESIAN_POINT('Ctrl Pts',(-0.657489443609774,0.497568426128753,
-1.19375390132824));
#58053=CARTESIAN_POINT('Ctrl Pts',(-0.815294248174704,0.123134057156335,
-1.17790453103326));
#58054=CARTESIAN_POINT('Ctrl Pts',(-0.775107455003299,-0.281203023342284,
-1.16205516073828));
#58055=CARTESIAN_POINT('Ctrl Pts',(-0.546688298145994,-0.617250849986269,
-1.14620579044329));
#58056=CARTESIAN_POINT('Ctrl Pts',(-0.185507638486464,-0.803401284042857,
-1.13035642014831));
#58057=CARTESIAN_POINT('Ctrl Pts',(0.220722957215736,-0.794448288623288,
-1.11450704985333));
#58058=CARTESIAN_POINT('Ctrl Pts',(0.573351689475297,-0.592566069999252,
-1.09865767955836));
#58059=CARTESIAN_POINT('Ctrl Pts',(0.786743799719937,-0.24678107857121,
-1.08280830926337));
#58060=CARTESIAN_POINT('Ctrl Pts',(0.809077697221824,0.158933907636998,
-1.06695893896839));
#58061=CARTESIAN_POINT('Ctrl Pts',(0.634929666481948,0.526052303254776,
-1.05110956867341));
#58062=CARTESIAN_POINT('Ctrl Pts',(0.306590999173255,0.765420581356732,
-1.03526019837843));
#58063=CARTESIAN_POINT('Ctrl Pts',(-0.0962023106326629,0.818908922022144,
-1.01941082808345));
#58064=CARTESIAN_POINT('Ctrl Pts',(-0.475633197324806,0.673527852980943,
-1.00356145778847));
#58065=CARTESIAN_POINT('Ctrl Pts',(-0.739558084942859,0.364582701364431,
-0.987712087493491));
#58066=CARTESIAN_POINT('Ctrl Pts',(-0.823883659571175,-0.0329001919469118,
-0.971862717198511));
#58067=CARTESIAN_POINT('Ctrl Pts',(-0.70813172540735,-0.422393378984735,
-0.956013346903529));
#58068=CARTESIAN_POINT('Ctrl Pts',(-0.420412269045156,-0.709309686367555,
-0.940163976608551));
#58069=CARTESIAN_POINT('Ctrl Pts',(-0.0305970392336053,-0.823972407504445,
-0.92431460631357));
#58070=CARTESIAN_POINT('Ctrl Pts',(0.366648583589333,-0.738536067697759,
-0.908465236018589));
#58071=CARTESIAN_POINT('Ctrl Pts',(0.674854771833728,-0.473748608516987,
-0.892615865723609));
#58072=CARTESIAN_POINT('Ctrl Pts',(0.819174639507985,-0.0939128166199715,
-0.876766495428628));
#58073=CARTESIAN_POINT('Ctrl Pts',(0.764560568834973,0.30872940210041,-0.860917125133647));
#58074=CARTESIAN_POINT('Ctrl Pts',(0.524275412012708,0.636397674019507,
-0.845067754838669));
#58075=CARTESIAN_POINT('Ctrl Pts',(0.156671650023453,0.809518808439597,
-0.829218384543686));
#58076=CARTESIAN_POINT('Ctrl Pts',(-0.248979320538142,0.786050892171048,
-0.813369014248708));
#58077=CARTESIAN_POINT('Ctrl Pts',(-0.594166460296292,0.571693033539423,
-0.797519643953725));
#58078=CARTESIAN_POINT('Ctrl Pts',(-0.795062177590985,0.218501352176174,
-0.781670273658746));
#58079=CARTESIAN_POINT('Ctrl Pts',(-0.802879590710967,-0.18775268295906,
-0.765820903363765));
#58080=CARTESIAN_POINT('Ctrl Pts',(-0.615720265910071,-0.5484115801897,
-0.749971533068785));
#58081=CARTESIAN_POINT('Ctrl Pts',(-0.279035245964017,-0.775890481091459,
-0.734122162773804));
#58082=CARTESIAN_POINT('Ctrl Pts',(0.125412590041216,-0.814946862928921,
-0.718272792478824));
#58083=CARTESIAN_POINT('Ctrl Pts',(0.499404380104624,-0.656096008424718,
-0.702423422183844));
#58084=CARTESIAN_POINT('Ctrl Pts',(0.752117415467132,-0.337914338981905,
-0.686574051888864));
#58085=CARTESIAN_POINT('Ctrl Pts',(0.822181144634913,0.0623287457386882,
-0.670724681593882));
#58086=CARTESIAN_POINT('Ctrl Pts',(0.692580815311664,0.447435494122635,
-0.654875311298904));
#58087=CARTESIAN_POINT('Ctrl Pts',(0.394789452515422,0.723883965370905,
-0.639025941003921));
#58088=CARTESIAN_POINT('Ctrl Pts',(0.00112473522419552,0.824539533381638,
-0.623176570708943));
#58089=CARTESIAN_POINT('Ctrl Pts',(-0.392813120415017,0.72495831574536,
-0.607327200413961));
#58090=CARTESIAN_POINT('Ctrl Pts',(-0.691357567481951,0.449323292322997,
-0.591477830118982));
#58091=CARTESIAN_POINT('Ctrl Pts',(-0.822008042894706,0.0645715460164029,
-0.575628459824001));
#58092=CARTESIAN_POINT('Ctrl Pts',(-0.753036497019803,-0.335861193493211,
-0.559779089529021));
#58093=CARTESIAN_POINT('Ctrl Pts',(-0.501192448937833,-0.654731117533164,
-0.543929719234039));
#58094=CARTESIAN_POINT('Ctrl Pts',(-0.127635419363948,-0.814601686017354,
-0.52808034893906));
#58095=CARTESIAN_POINT('Ctrl Pts',(0.276917463135748,-0.776648843267691,
-0.512230978644079));
#58096=CARTESIAN_POINT('Ctrl Pts',(0.614221826355172,-0.550089315627309,
-0.496381608349099));
#58097=CARTESIAN_POINT('Ctrl Pts',(0.802364385677912,-0.189942358978986,
-0.480532238054119));
#58098=CARTESIAN_POINT('Ctrl Pts',(0.795655322971835,0.21633149138468,-0.464682867759138));
#58099=CARTESIAN_POINT('Ctrl Pts',(0.595723912635665,0.570069931721507,
-0.448833497464158));
#58100=CARTESIAN_POINT('Ctrl Pts',(0.251122857519761,0.785368714407362,
-0.432984127169178));
#58101=CARTESIAN_POINT('Ctrl Pts',(-0.154462579487725,0.809943219413749,
-0.417134756874197));
#58102=CARTESIAN_POINT('Ctrl Pts',(-0.522537273638433,0.637825606889401,
-0.401285386579217));
#58103=CARTESIAN_POINT('Ctrl Pts',(-0.763715463943447,0.310814087932593,
-0.385436016284235));
#58104=CARTESIAN_POINT('Ctrl Pts',(-0.819427799150836,-0.091677637089383,
-0.369586645989256));
#58105=CARTESIAN_POINT('Ctrl Pts',(-0.676144716934526,-0.471905741510971,
-0.353737275694275));
#58106=CARTESIAN_POINT('Ctrl Pts',(-0.368662055243155,-0.737533047508205,
-0.337887905399296));
#58107=CARTESIAN_POINT('Ctrl Pts',(0.0283490064307482,-0.82405281449032,
-0.322038535104314));
#58108=CARTESIAN_POINT('Ctrl Pts',(0.418475602153286,-0.710453993719867,
-0.306189164809335));
#58109=CARTESIAN_POINT('Ctrl Pts',(0.706976738775498,-0.424323695776988,
-0.290339794514353));
#58110=CARTESIAN_POINT('Ctrl Pts',(0.82379083605636,-0.0351477460453753,
-0.274490424219374));
#58111=CARTESIAN_POINT('Ctrl Pts',(0.740549970253167,0.362563719550915,
-0.258641053924393));
#58112=CARTESIAN_POINT('Ctrl Pts',(0.477468907819966,0.6722277500993,-0.242791683629412));
#58113=CARTESIAN_POINT('Ctrl Pts',(0.0984360645185036,0.818643417281081,
-0.226942313334432));
#58114=CARTESIAN_POINT('Ctrl Pts',(-0.304501690502851,0.766254164680306,
-0.211092943039452));
#58115=CARTESIAN_POINT('Ctrl Pts',(-0.633492128901577,0.527782516252492,
-0.195243572744471));
#58116=CARTESIAN_POINT('Ctrl Pts',(-0.808641141858534,0.161140623251515,
-0.179394202449491));
#58117=CARTESIAN_POINT('Ctrl Pts',(-0.787414027818169,-0.244633851326282,
-0.16354483215451));
#58118=CARTESIAN_POINT('Ctrl Pts',(-0.574966358880064,-0.590999588154458,
-0.147695461859531));
#58119=CARTESIAN_POINT('Ctrl Pts',(-0.222889127189683,-0.793843339715672,
-0.131846091564549));
#58120=CARTESIAN_POINT('Ctrl Pts',(0.183314403237236,-0.803904048814602,
-0.11599672126957));
#58121=CARTESIAN_POINT('Ctrl Pts',(0.545003774088144,-0.618740661204861,
-0.100147350974589));
#58122=CARTESIAN_POINT('Ctrl Pts',(0.774334543703527,-0.28331528999698,
-0.0842979806796076));
#58123=CARTESIAN_POINT('Ctrl Pts',(0.815632750016524,0.120906817907845,
-0.0684486103846281));
#58124=CARTESIAN_POINT('Ctrl Pts',(0.658833433773886,0.495777831801544,
-0.0525992400896487));
#58125=CARTESIAN_POINT('Ctrl Pts',(0.342085277681465,0.750229523914293,
-0.0367498697946663));
#58126=CARTESIAN_POINT('Ctrl Pts',(-0.05783206721409,0.822534563742525,
-0.0209004994996869));
#58127=CARTESIAN_POINT('Ctrl Pts',(-0.314931867400366,0.737493998316566,
-0.0103342526363675));
#58128=CARTESIAN_POINT('Ctrl Pts',(-0.425612326351242,0.666853325445622,
-0.00505112920470729));
#58129=CARTESIAN_POINT('Ctrl Pts',(-0.791044518748003,1.1964098827608E-5,
-0.173133150823703));
#58130=CARTESIAN_POINT('Ctrl Pts',(-0.79100173359616,-0.0794357270706935,
-0.169937044600639));
#58131=CARTESIAN_POINT('Ctrl Pts',(-0.779104790250919,-0.158895943316062,
-0.166740938377575));
#58132=CARTESIAN_POINT('Ctrl Pts',(-0.755543935335212,-0.234732395034678,
-0.163544832154511));
#58133=CARTESIAN_POINT('Ctrl Pts',(-0.716598138172134,-0.360089096935673,
-0.158261708722851));
#58134=CARTESIAN_POINT('Ctrl Pts',(-0.645782248526095,-0.47554434254507,
-0.15297858529119));
#58135=CARTESIAN_POINT('Ctrl Pts',(-0.551694765088015,-0.567079257276634,
-0.14769546185953));
#58136=CARTESIAN_POINT('Ctrl Pts',(-0.457607281649931,-0.6586141720082,
-0.14241233842787));
#58137=CARTESIAN_POINT('Ctrl Pts',(-0.340248204419803,-0.726228755861938,
-0.137129214996209));
#58138=CARTESIAN_POINT('Ctrl Pts',(-0.213868077400249,-0.761712832638628,
-0.131846091564549));
#58139=CARTESIAN_POINT('Ctrl Pts',(-0.0874879503807029,-0.797196909415316,
-0.126562968132889));
#58140=CARTESIAN_POINT('Ctrl Pts',(0.047913226428263,-0.800550479114958,
-0.121279844701229));
#58141=CARTESIAN_POINT('Ctrl Pts',(0.175895376641231,-0.771366699363157,
-0.11599672126957));
#58142=CARTESIAN_POINT('Ctrl Pts',(0.303877526854205,-0.742182919611355,
-0.110713597837909));
#58143=CARTESIAN_POINT('Ctrl Pts',(0.424440650471175,-0.680461790408108,
-0.105430474406249));
#58144=CARTESIAN_POINT('Ctrl Pts',(0.522944007215559,-0.593696997271835,
-0.100147350974589));
#58145=CARTESIAN_POINT('Ctrl Pts',(0.621447363959938,-0.506932204135567,
-0.0948642275429287));
#58146=CARTESIAN_POINT('Ctrl Pts',(0.697890953831734,-0.39512374706627,
-0.089581104111268));
#58147=CARTESIAN_POINT('Ctrl Pts',(0.74299578315313,-0.271849167214156,
-0.084297980679608));
#58148=CARTESIAN_POINT('Ctrl Pts',(0.780555172255761,-0.169196790943382,
-0.079898653786405));
#58149=CARTESIAN_POINT('Ctrl Pts',(0.796383908785544,-0.0585936748802548,
-0.0754993268932024));
#58150=CARTESIAN_POINT('Ctrl Pts',(0.789513386643969,0.0505148782186592,
-0.0710999999999996));
#58151=CARTESIAN_POINT('',(-0.392914082828325,-0.550975096793568,-3.8089));
#58152=CARTESIAN_POINT('Ctrl Pts',(-0.392914082828323,-0.55097509679357,
-3.8089));
#58153=CARTESIAN_POINT('Ctrl Pts',(-0.40918120771343,-0.541286508891915,
-3.8089));
#58154=CARTESIAN_POINT('Ctrl Pts',(-0.425015397297533,-0.530925220216701,
-3.8089));
#58155=CARTESIAN_POINT('Ctrl Pts',(-0.440371919198835,-0.519915908540044,
-3.8089));
#58156=CARTESIAN_POINT('Ctrl Pts',(-0.463863529910594,-0.503074434554289,
-3.8089));
#58157=CARTESIAN_POINT('Ctrl Pts',(-0.486238252705378,-0.484717838355465,
-3.8089));
#58158=CARTESIAN_POINT('Ctrl Pts',(-0.507401942220326,-0.464998685887743,
-3.8089));
#58159=CARTESIAN_POINT('Ctrl Pts',(-0.515792943867532,-0.457180415792574,
-3.8089));
#58160=CARTESIAN_POINT('Ctrl Pts',(-0.523993416640949,-0.449147646509594,
-3.8089));
#58161=CARTESIAN_POINT('Ctrl Pts',(-0.531996773114634,-0.440908761680904,
-3.8089));
#58162=CARTESIAN_POINT('Ctrl Pts',(-0.538443563678603,-0.434272250468907,
-3.8089));
#58163=CARTESIAN_POINT('Ctrl Pts',(-0.544756551181799,-0.427507946632577,
-3.8089));
#58164=CARTESIAN_POINT('Ctrl Pts',(-0.550928946975755,-0.420625294631357,
-3.8089));
#58165=CARTESIAN_POINT('Ctrl Pts',(-0.573001593541319,-0.396012753548773,
-3.8089));
#58166=CARTESIAN_POINT('Ctrl Pts',(-0.593294908866083,-0.369873018445606,
-3.8089));
#58167=CARTESIAN_POINT('Ctrl Pts',(-0.611667100237218,-0.342421230741072,
-3.8089));
#58168=CARTESIAN_POINT('Ctrl Pts',(-0.619162124335873,-0.331222141517567,
-3.8089));
#58169=CARTESIAN_POINT('Ctrl Pts',(-0.62633709313012,-0.319804236221353,
-3.8089));
#58170=CARTESIAN_POINT('Ctrl Pts',(-0.633180820484676,-0.308180442575769,
-3.8089));
#58171=CARTESIAN_POINT('Ctrl Pts',(-0.63932108837351,-0.297751446332822,
-3.8089));
#58172=CARTESIAN_POINT('Ctrl Pts',(-0.64519767546254,-0.287150351905675,
-3.8089));
#58173=CARTESIAN_POINT('Ctrl Pts',(-0.650785040045425,-0.276419954666599,
-3.8089));
#58174=CARTESIAN_POINT('Ctrl Pts',(-0.654235318101704,-0.269793779914632,
-3.8089));
#58175=CARTESIAN_POINT('Ctrl Pts',(-0.657576472430511,-0.263116566740529,
-3.8089));
#58176=CARTESIAN_POINT('Ctrl Pts',(-0.660807074331226,-0.256390831914409,
-3.8089));
#58177=CARTESIAN_POINT('Ctrl Pts',(-0.675536657386884,-0.225725564952934,
-3.8089));
#58178=CARTESIAN_POINT('Ctrl Pts',(-0.68797141621589,-0.194054477335829,
-3.8089));
#58179=CARTESIAN_POINT('Ctrl Pts',(-0.698114300840514,-0.161654804678165,
-3.8089));
#58180=CARTESIAN_POINT('Ctrl Pts',(-0.704963477685347,-0.139776306010412,
-3.8089));
#58181=CARTESIAN_POINT('Ctrl Pts',(-0.710766765544529,-0.117564703199071,
-3.8089));
#58182=CARTESIAN_POINT('Ctrl Pts',(-0.715513681283513,-0.0950982670235596,
-3.8089));
#58183=CARTESIAN_POINT('Ctrl Pts',(-0.719157231569141,-0.0778538931089195,
-3.8089));
#58184=CARTESIAN_POINT('Ctrl Pts',(-0.722178239005175,-0.0604592545141676,
-3.8089));
#58185=CARTESIAN_POINT('Ctrl Pts',(-0.72456797160588,-0.0429485118438729,
-3.8089));
#58186=CARTESIAN_POINT('Ctrl Pts',(-0.725925391688996,-0.0330020292274042,
-3.8089));
#58187=CARTESIAN_POINT('Ctrl Pts',(-0.727079334996212,-0.0230129598479465,
-3.8089));
#58188=CARTESIAN_POINT('Ctrl Pts',(-0.728025398727401,-0.0130183828336468,
-3.8089));
#58189=CARTESIAN_POINT('Ctrl Pts',(-0.731393629154257,0.0225648842268292,
-3.8089));
#58190=CARTESIAN_POINT('Ctrl Pts',(-0.732142255374346,0.0582803512346346,
-3.8089));
#58191=CARTESIAN_POINT('Ctrl Pts',(-0.730254992650321,0.0938353307035594,
-3.8089));
#58192=CARTESIAN_POINT('Ctrl Pts',(-0.72860412584696,0.124936742580253,
-3.8089));
#58193=CARTESIAN_POINT('Ctrl Pts',(-0.724935845899013,0.15591642275622,
-3.8089));
#58194=CARTESIAN_POINT('Ctrl Pts',(-0.719327670522454,0.186600715052318,
-3.8089));
#58195=CARTESIAN_POINT('Ctrl Pts',(-0.716083605646998,0.204350130536374,
-3.8089));
#58196=CARTESIAN_POINT('Ctrl Pts',(-0.712189804953552,0.222000777314424,
-3.8089));
#58197=CARTESIAN_POINT('Ctrl Pts',(-0.707656253686562,0.23951869490032,
-3.8089));
#58198=CARTESIAN_POINT('Ctrl Pts',(-0.7049639395012,0.249921960516378,-3.8089));
#58199=CARTESIAN_POINT('Ctrl Pts',(-0.702043919906257,0.260284226662841,
-3.8089));
#58200=CARTESIAN_POINT('Ctrl Pts',(-0.69890838365347,0.270565505236912,
-3.8089));
#58201=CARTESIAN_POINT('Ctrl Pts',(-0.688429596994019,0.30492496278372,
-3.8089));
#58202=CARTESIAN_POINT('Ctrl Pts',(-0.675536134189328,0.338436818685454,
-3.8089));
#58203=CARTESIAN_POINT('Ctrl Pts',(-0.660358260231301,0.37084656623089,
-3.8089));
#58204=CARTESIAN_POINT('Ctrl Pts',(-0.648063055903144,0.397100867024078,
-3.8089));
#58205=CARTESIAN_POINT('Ctrl Pts',(-0.634267661582395,0.422632407626466,
-3.8089));
#58206=CARTESIAN_POINT('Ctrl Pts',(-0.619016563283335,0.447302153870391,
-3.8089));
#58207=CARTESIAN_POINT('Ctrl Pts',(-0.610140667155518,0.46165955298139,
-3.8089));
#58208=CARTESIAN_POINT('Ctrl Pts',(-0.600771307583703,0.475724949322109,
-3.8089));
#58209=CARTESIAN_POINT('Ctrl Pts',(-0.590928823493088,0.48948061897489,
-3.8089));
#58210=CARTESIAN_POINT('Ctrl Pts',(-0.585588676888875,0.49694390689171,
-3.8089));
#58211=CARTESIAN_POINT('Ctrl Pts',(-0.580109216265542,0.504315997059902,
-3.8089));
#58212=CARTESIAN_POINT('Ctrl Pts',(-0.574493428009887,0.511593875250418,
-3.8089));
#58213=CARTESIAN_POINT('Ctrl Pts',(-0.569979146106706,0.517444237178845,
-3.8089));
#58214=CARTESIAN_POINT('Ctrl Pts',(-0.565377157064798,0.523233006723831,
-3.8089));
#58215=CARTESIAN_POINT('Ctrl Pts',(-0.560697658032463,0.528948601785265,
-3.8089));
#58216=CARTESIAN_POINT('Ctrl Pts',(-0.53768323827103,0.557058684300788,
-3.8089));
#58217=CARTESIAN_POINT('Ctrl Pts',(-0.512747626910434,0.583466684665809,
-3.8089));
#58218=CARTESIAN_POINT('Ctrl Pts',(-0.486128957191253,0.608022959642477,
-3.8089));
#58219=CARTESIAN_POINT('Ctrl Pts',(-0.459292913757588,0.632779766379819,
-3.8089));
#58220=CARTESIAN_POINT('Ctrl Pts',(-0.43074544663,0.655655429636067,-3.8089));
#58221=CARTESIAN_POINT('Ctrl Pts',(-0.400686420987431,0.676468800819551,
-3.8089));
#58222=CARTESIAN_POINT('Ctrl Pts',(-0.38173423202165,0.689591612861925,
-3.8089));
#58223=CARTESIAN_POINT('Ctrl Pts',(-0.362180310994124,0.701894004325692,
-3.8089));
#58224=CARTESIAN_POINT('Ctrl Pts',(-0.342067962509734,0.713322310757514,
-3.8089));
#58225=CARTESIAN_POINT('Ctrl Pts',(-0.392914082828325,-0.550975096793569,
-3.8089));
#58226=CARTESIAN_POINT('Ctrl Pts',(-0.316721006496901,-0.605194430403013,
-3.8045006731068));
#58227=CARTESIAN_POINT('Ctrl Pts',(-0.124097906710261,-0.689702849642968,
-3.79481822278193));
#58228=CARTESIAN_POINT('Ctrl Pts',(0.203771242261294,-0.675228509254,-3.77985264902541));
#58229=CARTESIAN_POINT('Ctrl Pts',(0.501518367203066,-0.495916548685635,
-3.76400327873043));
#58230=CARTESIAN_POINT('Ctrl Pts',(0.677472975891979,-0.19617577998387,
-3.74815390843546));
#58231=CARTESIAN_POINT('Ctrl Pts',(0.688905638980991,0.15120714934306,-3.73230453814047));
#58232=CARTESIAN_POINT('Ctrl Pts',(0.533039672552928,0.46186914013689,-3.71645516784549));
#58233=CARTESIAN_POINT('Ctrl Pts',(0.24772677985824,0.66036808055943,-3.70060579755051));
#58234=CARTESIAN_POINT('Ctrl Pts',(-0.097745794456612,0.698498547043651,
-3.68475642725553));
#58235=CARTESIAN_POINT('Ctrl Pts',(-0.419481102114336,0.567000979985795,
-3.66890705696055));
#58236=CARTESIAN_POINT('Ctrl Pts',(-0.630220227894166,0.308983052482088,
-3.65371558841504));
#58237=CARTESIAN_POINT('Ctrl Pts',(-0.676650477069334,0.0982983612630573,
-3.64380724330119));
#58238=CARTESIAN_POINT('Ctrl Pts',(-0.67673605652177,-1.28860430050285E-5,
-3.639182021619));
#58239=CARTESIAN_POINT('Origin',(-1.87869726832665E-16,-4.25270154953079E-17,
-3.8089));
#58240=CARTESIAN_POINT('',(-0.7911,-9.68818082805471E-17,-3.8089));
#58241=CARTESIAN_POINT('Origin',(0.,0.,-3.8089));
#58242=CARTESIAN_POINT('Origin',(0.,0.,-3.8089));
#58243=CARTESIAN_POINT('',(0.392888236737271,-0.550964357679767,-3.8089));
#58244=CARTESIAN_POINT('Ctrl Pts',(0.342095581308743,0.713339856610552,
-3.8089));
#58245=CARTESIAN_POINT('Ctrl Pts',(0.36121279300994,0.702501567673476,-3.8089));
#58246=CARTESIAN_POINT('Ctrl Pts',(0.37984607702609,0.690878787228922,-3.8089));
#58247=CARTESIAN_POINT('Ctrl Pts',(0.397940630435775,0.678487386031165,
-3.8089));
#58248=CARTESIAN_POINT('Ctrl Pts',(0.424451217565607,0.660332568187579,
-3.8089));
#58249=CARTESIAN_POINT('Ctrl Pts',(0.449806577768339,0.640528540279525,
-3.8089));
#58250=CARTESIAN_POINT('Ctrl Pts',(0.473876877114966,0.619209890699569,
-3.8089));
#58251=CARTESIAN_POINT('Ctrl Pts',(0.483771335729022,0.610446539112668,
-3.8089));
#58252=CARTESIAN_POINT('Ctrl Pts',(0.493448376032635,0.601427032669218,
-3.8089));
#58253=CARTESIAN_POINT('Ctrl Pts',(0.502897725274963,0.592159917140135,
-3.8089));
#58254=CARTESIAN_POINT('Ctrl Pts',(0.509419954580009,0.585763471106973,
-3.8089));
#58255=CARTESIAN_POINT('Ctrl Pts',(0.515830745518692,0.579251786110235,
-3.8089));
#58256=CARTESIAN_POINT('Ctrl Pts',(0.522120551240599,0.572634917336308,
-3.8089));
#58257=CARTESIAN_POINT('Ctrl Pts',(0.547671800606227,0.545755030812409,
-3.8089));
#58258=CARTESIAN_POINT('Ctrl Pts',(0.571263889736759,0.517108988254135,
-3.8089));
#58259=CARTESIAN_POINT('Ctrl Pts',(0.592688323170684,0.486902555544426,
-3.8089));
#58260=CARTESIAN_POINT('Ctrl Pts',(0.6060488685909,0.468065445221511,-3.8089));
#58261=CARTESIAN_POINT('Ctrl Pts',(0.618565526028434,0.448620849726152,
-3.8089));
#58262=CARTESIAN_POINT('Ctrl Pts',(0.630177040564387,0.428614402836241,
-3.8089));
#58263=CARTESIAN_POINT('Ctrl Pts',(0.634151625121932,0.42176625958897,-3.8089));
#58264=CARTESIAN_POINT('Ctrl Pts',(0.638015062537283,0.414860897563193,
-3.8089));
#58265=CARTESIAN_POINT('Ctrl Pts',(0.641765273269331,0.407900970199179,
-3.8089));
#58266=CARTESIAN_POINT('Ctrl Pts',(0.644627675464558,0.402588705692247,
-3.8089));
#58267=CARTESIAN_POINT('Ctrl Pts',(0.647424172391886,0.397244548798339,
-3.8089));
#58268=CARTESIAN_POINT('Ctrl Pts',(0.650153933287359,0.391869417938239,
-3.8089));
#58269=CARTESIAN_POINT('Ctrl Pts',(0.666288679035159,0.360098734310713,
-3.8089));
#58270=CARTESIAN_POINT('Ctrl Pts',(0.680096002267384,0.327247301124806,
-3.8089));
#58271=CARTESIAN_POINT('Ctrl Pts',(0.691525041999413,0.293582472433363,
-3.8089));
#58272=CARTESIAN_POINT('Ctrl Pts',(0.702852857674015,0.260215804447685,
-3.8089));
#58273=CARTESIAN_POINT('Ctrl Pts',(0.711844433318636,0.226048834947817,
-3.8089));
#58274=CARTESIAN_POINT('Ctrl Pts',(0.71839997405433,0.191336560614048,-3.8089));
#58275=CARTESIAN_POINT('Ctrl Pts',(0.720682240379993,0.179251721545355,
-3.8089));
#58276=CARTESIAN_POINT('Ctrl Pts',(0.722668793691289,0.167100828440312,
-3.8089));
#58277=CARTESIAN_POINT('Ctrl Pts',(0.724353936498504,0.154894909635805,
-3.8089));
#58278=CARTESIAN_POINT('Ctrl Pts',(0.725348929252383,0.147687923549573,
-3.8089));
#58279=CARTESIAN_POINT('Ctrl Pts',(0.72623754978894,0.140470862544136,-3.8089));
#58280=CARTESIAN_POINT('Ctrl Pts',(0.727019157369881,0.133248004731528,
-3.8089));
#58281=CARTESIAN_POINT('Ctrl Pts',(0.730644198307119,0.0997488986672927,
-3.8089));
#58282=CARTESIAN_POINT('Ctrl Pts',(0.731972955727726,0.0661109163631112,
-3.8089));
#58283=CARTESIAN_POINT('Ctrl Pts',(0.7309415524454,0.03255904596736,-3.8089));
#58284=CARTESIAN_POINT('Ctrl Pts',(0.730024558511494,0.00272894735187942,
-3.8089));
#58285=CARTESIAN_POINT('Ctrl Pts',(0.727241148278698,-0.0270336586862393,
-3.8089));
#58286=CARTESIAN_POINT('Ctrl Pts',(0.722626861054683,-0.0565585721414304,
-3.8089));
#58287=CARTESIAN_POINT('Ctrl Pts',(0.720147537884213,-0.0724227345747074,
-3.8089));
#58288=CARTESIAN_POINT('Ctrl Pts',(0.717139169466594,-0.088218119370617,
-3.8089));
#58289=CARTESIAN_POINT('Ctrl Pts',(0.71360426348179,-0.103916722064461,
-3.8089));
#58290=CARTESIAN_POINT('Ctrl Pts',(0.712023618639872,-0.110936403911731,
-3.8089));
#58291=CARTESIAN_POINT('Ctrl Pts',(0.710337667999657,-0.117936715941189,
-3.8089));
#58292=CARTESIAN_POINT('Ctrl Pts',(0.708546509596779,-0.124915054508574,
-3.8089));
#58293=CARTESIAN_POINT('Ctrl Pts',(0.706599664866173,-0.132499945742351,
-3.8089));
#58294=CARTESIAN_POINT('Ctrl Pts',(0.704530543424124,-0.140050769984527,
-3.8089));
#58295=CARTESIAN_POINT('Ctrl Pts',(0.702341826791288,-0.147558585047062,
-3.8089));
#58296=CARTESIAN_POINT('Ctrl Pts',(0.692840226549643,-0.180151318314681,
-3.8089));
#58297=CARTESIAN_POINT('Ctrl Pts',(0.681079279247323,-0.211971147619771,
-3.8089));
#58298=CARTESIAN_POINT('Ctrl Pts',(0.66712289065792,-0.242769220807921,
-3.8089));
#58299=CARTESIAN_POINT('Ctrl Pts',(0.656934524727168,-0.265252260570885,
-3.8089));
#58300=CARTESIAN_POINT('Ctrl Pts',(0.645575103228812,-0.287190573685416,
-3.8089));
#58301=CARTESIAN_POINT('Ctrl Pts',(0.633054891849579,-0.308477498341469,
-3.8089));
#58302=CARTESIAN_POINT('Ctrl Pts',(0.624944614015227,-0.322266632404003,
-3.8089));
#58303=CARTESIAN_POINT('Ctrl Pts',(0.61634697984595,-0.335782233726575,
-3.8089));
#58304=CARTESIAN_POINT('Ctrl Pts',(0.607278987278486,-0.349001209705128,
-3.8089));
#58305=CARTESIAN_POINT('Ctrl Pts',(0.602478801187708,-0.355998739109185,
-3.8089));
#58306=CARTESIAN_POINT('Ctrl Pts',(0.597546788253189,-0.362913113695733,
-3.8089));
#58307=CARTESIAN_POINT('Ctrl Pts',(0.592485323085494,-0.369740651388275,
-3.8089));
#58308=CARTESIAN_POINT('Ctrl Pts',(0.588725489253597,-0.374812385827705,
-3.8089));
#58309=CARTESIAN_POINT('Ctrl Pts',(0.584895221083396,-0.379834711363469,
-3.8089));
#58310=CARTESIAN_POINT('Ctrl Pts',(0.581001430593434,-0.384799080112452,
-3.8089));
#58311=CARTESIAN_POINT('Ctrl Pts',(0.560423538217804,-0.411034761280424,
-3.8089));
#58312=CARTESIAN_POINT('Ctrl Pts',(0.53803152477826,-0.435713343348598,
-3.8089));
#58313=CARTESIAN_POINT('Ctrl Pts',(0.514011098046997,-0.458656110995473,
-3.8089));
#58314=CARTESIAN_POINT('Ctrl Pts',(0.490436458056322,-0.48117309180168,
-3.8089));
#58315=CARTESIAN_POINT('Ctrl Pts',(0.465292264875717,-0.50201872351403,
-3.8089));
#58316=CARTESIAN_POINT('Ctrl Pts',(0.438727568397101,-0.520982709860239,
-3.8089));
#58317=CARTESIAN_POINT('Ctrl Pts',(0.423883704104649,-0.531579436986169,
-3.8089));
#58318=CARTESIAN_POINT('Ctrl Pts',(0.40859591590594,-0.541587847856024,
-3.8089));
#58319=CARTESIAN_POINT('Ctrl Pts',(0.392888236737278,-0.550964357679762,
-3.8089));
#58320=CARTESIAN_POINT('Origin',(0.,0.,-3.8089));
#58321=CARTESIAN_POINT('Origin',(0.,0.,-4.178617978381));
#58322=CARTESIAN_POINT('Ctrl Pts',(0.392888236737271,-0.550964357679767,
-3.8089));
#58323=CARTESIAN_POINT('Ctrl Pts',(0.484334114933679,-0.485755039979474,
-3.80361687656834));
#58324=CARTESIAN_POINT('Ctrl Pts',(0.634040615230541,-0.308993274199896,
-3.79305062970502));
#58325=CARTESIAN_POINT('Ctrl Pts',(0.704605176817581,0.0314014527883039,
-3.77720125941004));
#58326=CARTESIAN_POINT('Ctrl Pts',(0.604063223483086,0.364081211703574,
-3.76135188911506));
#58327=CARTESIAN_POINT('Ctrl Pts',(0.356824591291676,0.608388806027088,
-3.74550251882008));
#58328=CARTESIAN_POINT('Ctrl Pts',(0.0229331537905069,0.704928930307171,
-3.7296531485251));
#58329=CARTESIAN_POINT('Ctrl Pts',(-0.316527984197726,0.630290638914377,
-3.71380377823012));
#58330=CARTESIAN_POINT('Ctrl Pts',(-0.57912108147644,0.402582506643355,
-3.69795440793514));
#58331=CARTESIAN_POINT('Ctrl Pts',(-0.669368670582889,0.161732571732784,
-3.68622580798543));
#58332=CARTESIAN_POINT('Ctrl Pts',(-0.676729148312702,0.0247271568507296,
-3.67978033146739));
#58333=CARTESIAN_POINT('Ctrl Pts',(-0.676703788167417,1.73951649275021E-5,
-3.678617978381));
#58334=CARTESIAN_POINT('Ctrl Pts',(0.459308237155087,-0.644108029201225,
-3.87494887079529));
#58335=CARTESIAN_POINT('Ctrl Pts',(0.566213563357509,-0.567874703897988,
-3.86966574736363));
#58336=CARTESIAN_POINT('Ctrl Pts',(0.741228802584419,-0.36123035203125,
-3.85909950050031));
#58337=CARTESIAN_POINT('Ctrl Pts',(0.823722706340163,0.0367100477328463,
-3.84325013020534));
#58338=CARTESIAN_POINT('Ctrl Pts',(0.70618356154496,0.425631220006929,-3.82740075991035));
#58339=CARTESIAN_POINT('Ctrl Pts',(0.417147826467938,0.711240408523754,
-3.81155138961537));
#58340=CARTESIAN_POINT('Ctrl Pts',(0.026810134422462,0.824101192206298,
-3.79570201932039));
#58341=CARTESIAN_POINT('Ctrl Pts',(-0.370038847788994,0.736844871353877,
-3.77985264902541));
#58342=CARTESIAN_POINT('Ctrl Pts',(-0.677024807974,0.470641378758041,-3.76400327873043));
#58343=CARTESIAN_POINT('Ctrl Pts',(-0.819597600423394,0.0901475825088134,
-3.74815390843546));
#58344=CARTESIAN_POINT('Ctrl Pts',(-0.763133668772108,-0.312240026097584,
-3.73230453814046));
#58345=CARTESIAN_POINT('Ctrl Pts',(-0.521345205358778,-0.638800245198537,
-3.7164551678455));
#58346=CARTESIAN_POINT('Ctrl Pts',(-0.152949709560969,-0.810230329040985,
-3.70060579755051));
#58347=CARTESIAN_POINT('Ctrl Pts',(0.252589124028344,-0.784898337362364,
-3.68475642725553));
#58348=CARTESIAN_POINT('Ctrl Pts',(0.596787502422859,-0.568956417209875,
-3.66890705696055));
#58349=CARTESIAN_POINT('Ctrl Pts',(0.796057944200422,-0.214845191751947,
-3.65305768666557));
#58350=CARTESIAN_POINT('Ctrl Pts',(0.802008264329106,0.19144046943575,-3.63720831637059));
#58351=CARTESIAN_POINT('Ctrl Pts',(0.613193444716271,0.551235441505258,
-3.62135894607561));
#58352=CARTESIAN_POINT('Ctrl Pts',(0.275466560722855,0.777164643436226,
-3.60550957578063));
#58353=CARTESIAN_POINT('Ctrl Pts',(-0.12915649571277,0.814361904208446,
-3.58966020548564));
#58354=CARTESIAN_POINT('Ctrl Pts',(-0.502414310616047,0.653793981871771,
-3.57381083519067));
#58355=CARTESIAN_POINT('Ctrl Pts',(-0.753662418874675,0.334454285456363,
-3.55796146489568));
#58356=CARTESIAN_POINT('Ctrl Pts',(-0.821886021785598,-0.06610656386918,
-3.54211209460071));
#58357=CARTESIAN_POINT('Ctrl Pts',(-0.690517235855899,-0.450613645538905,
-3.52626272430572));
#58358=CARTESIAN_POINT('Ctrl Pts',(-0.391458550111,-0.725690646321452,-3.51041335401075));
#58359=CARTESIAN_POINT('Ctrl Pts',(0.00266459114198865,-0.824535997108764,
-3.49456398371576));
#58360=CARTESIAN_POINT('Ctrl Pts',(0.396140644969226,-0.723145421059153,
-3.47871461342078));
#58361=CARTESIAN_POINT('Ctrl Pts',(0.69341521153958,-0.44614129487425,-3.46286524312581));
#58362=CARTESIAN_POINT('Ctrl Pts',(0.822296114184983,-0.0607931837071266,
-3.44701587283082));
#58363=CARTESIAN_POINT('Ctrl Pts',(0.751485038352033,0.339318357478879,
-3.43116650253584));
#58364=CARTESIAN_POINT('Ctrl Pts',(0.498178227082102,0.657027521987999,
-3.41531713224086));
#58365=CARTESIAN_POINT('Ctrl Pts',(0.123890428446799,0.815179656473512,
-3.39946776194588));
#58366=CARTESIAN_POINT('Ctrl Pts',(-0.280483764060795,0.775368021449757,
-3.3836183916509));
#58367=CARTESIAN_POINT('Ctrl Pts',(-0.616743372527332,0.547260745013206,
-3.36776902135592));
#58368=CARTESIAN_POINT('Ctrl Pts',(-0.80322882768251,0.186252948885433,
-3.35191965106094));
#58369=CARTESIAN_POINT('Ctrl Pts',(-0.794652733836475,-0.219985779528958,
-3.33607028076596));
#58370=CARTESIAN_POINT('Ctrl Pts',(-0.593097767920537,-0.572801665741669,
-3.32022091047098));
#58371=CARTESIAN_POINT('Ctrl Pts',(-0.247510908062826,-0.786514501442065,
-3.304371540176));
#58372=CARTESIAN_POINT('Ctrl Pts',(0.158183183330303,-0.809224808752328,
-3.28852216988102));
#58373=CARTESIAN_POINT('Ctrl Pts',(0.525462995127194,-0.63541746225667,
-3.27267279958604));
#58374=CARTESIAN_POINT('Ctrl Pts',(0.765135801000186,-0.307301019550136,
-3.25682342929106));
#58375=CARTESIAN_POINT('Ctrl Pts',(0.818997827434396,0.0954424918287849,
-3.24097405899608));
#58376=CARTESIAN_POINT('Ctrl Pts',(0.673968853767286,0.475008099657638,
-3.2251246887011));
#58377=CARTESIAN_POINT('Ctrl Pts',(0.365268701895915,0.739219511379414,
-3.20927531840612));
#58378=CARTESIAN_POINT('Ctrl Pts',(-0.0321357847028984,0.823913831617287,
-3.19342594811114));
#58379=CARTESIAN_POINT('Ctrl Pts',(-0.421736198879906,0.708523315878227,
-3.17757657781615));
#58380=CARTESIAN_POINT('Ctrl Pts',(-0.708919327486185,0.421070181448749,
-3.16172720752118));
#58381=CARTESIAN_POINT('Ctrl Pts',(-0.823943667251017,0.0313615016492279,
-3.14587783722619));
#58382=CARTESIAN_POINT('Ctrl Pts',(-0.738875925550794,-0.365963218411641,
-3.13002846693122));
#58383=CARTESIAN_POINT('Ctrl Pts',(-0.474374531085041,-0.674414942632945,
-3.11417909663623));
#58384=CARTESIAN_POINT('Ctrl Pts',(-0.094672800611489,-0.819087157397261,
-3.09832972634126));
#58385=CARTESIAN_POINT('Ctrl Pts',(0.308019916364428,-0.764846678564796,
-3.08248035604627));
#58386=CARTESIAN_POINT('Ctrl Pts',(0.635910982878394,-0.524865632751264,
-3.06663098575129));
#58387=CARTESIAN_POINT('Ctrl Pts',(0.809373103278666,-0.157422648554173,
-3.05078161545632));
#58388=CARTESIAN_POINT('Ctrl Pts',(0.786281557022114,0.248249921803872,
-3.03493224516133));
#58389=CARTESIAN_POINT('Ctrl Pts',(0.572244052181956,0.593635793505685,
-3.01908287486635));
#58390=CARTESIAN_POINT('Ctrl Pts',(0.219238911497098,0.794859113475034,
-3.00323350457137));
#58391=CARTESIAN_POINT('Ctrl Pts',(-0.187007696879292,0.803053442740053,
-2.98738413427639));
#58392=CARTESIAN_POINT('Ctrl Pts',(-0.54784008483524,0.616228814675576,
-2.97153476398142));
#58393=CARTESIAN_POINT('Ctrl Pts',(-0.775631262279306,0.279754992026522,
-2.95568539368643));
#58394=CARTESIAN_POINT('Ctrl Pts',(-0.815062871117633,-0.124656434708484,
-2.93983602339145));
#58395=CARTESIAN_POINT('Ctrl Pts',(-0.656559071397106,-0.498795445403142,
-2.92398665309647));
#58396=CARTESIAN_POINT('Ctrl Pts',(-0.338612003377769,-0.751803579239446,
-2.90813728280149));
#58397=CARTESIAN_POINT('Ctrl Pts',(0.0615659054840728,-0.822238621004071,
-2.89228791250651));
#58398=CARTESIAN_POINT('Ctrl Pts',(0.446792731322623,-0.692995646325444,
-2.87643854221153));
#58399=CARTESIAN_POINT('Ctrl Pts',(0.723517372913463,-0.395460897790348,
-2.86058917191655));
#58400=CARTESIAN_POINT('Ctrl Pts',(0.82453813707129,-0.00188973642509855,
-2.84473980162157));
#58401=CARTESIAN_POINT('Ctrl Pts',(0.725322454671599,0.392140341380372,
-2.82889043132659));
#58402=CARTESIAN_POINT('Ctrl Pts',(0.449964536513494,0.690940392847998,
-2.8130410610316));
#58403=CARTESIAN_POINT('Ctrl Pts',(0.0653341713726577,0.821947782185582,
-2.79719169073663));
#58404=CARTESIAN_POINT('Ctrl Pts',(-0.335162388097172,0.753347784355771,
-2.78134232044164));
#58405=CARTESIAN_POINT('Ctrl Pts',(-0.654265834750312,0.501799689186061,
-2.76549295014667));
#58406=CARTESIAN_POINT('Ctrl Pts',(-0.814482918281762,0.128391146174389,
-2.74964357985169));
#58407=CARTESIAN_POINT('Ctrl Pts',(-0.776905432943641,-0.276196775599218,
-2.73379420955671));
#58408=CARTESIAN_POINT('Ctrl Pts',(-0.55065895073362,-0.613711194753442,
-2.71794483926172));
#58409=CARTESIAN_POINT('Ctrl Pts',(-0.190686705453825,-0.802187815260189,
-2.70209546896675));
#58410=CARTESIAN_POINT('Ctrl Pts',(0.21559319569918,-0.795855693299335,
-2.68624609867176));
#58411=CARTESIAN_POINT('Ctrl Pts',(0.569516979569217,-0.596252564414699,
-2.67039672837679));
#58412=CARTESIAN_POINT('Ctrl Pts',(0.78513538844694,-0.251851409360799,
-2.6545473580818));
#58413=CARTESIAN_POINT('Ctrl Pts',(0.810086182109703,0.153711054071187,
-2.63869798778682));
#58414=CARTESIAN_POINT('Ctrl Pts',(0.638310140204678,0.52194528017852,-2.62284861749184));
#58415=CARTESIAN_POINT('Ctrl Pts',(0.311522524510963,0.763426766174114,
-2.60699924719686));
#58416=CARTESIAN_POINT('Ctrl Pts',(-0.090917338818336,0.819512506366401,
-2.59114987690188));
#58417=CARTESIAN_POINT('Ctrl Pts',(-0.471278217517389,0.676582258326644,
-2.5753005066069));
#58418=CARTESIAN_POINT('Ctrl Pts',(-0.737190690044681,0.369346175153063,
-2.55945113631192));
#58419=CARTESIAN_POINT('Ctrl Pts',(-0.824078763853267,-0.0275844440730886,
-2.54360176601694));
#58420=CARTESIAN_POINT('Ctrl Pts',(-0.710841948419499,-0.417816269376767,
-2.52775239572196));
#58421=CARTESIAN_POINT('Ctrl Pts',(-0.424979441806532,-0.706582751438611,
-2.51190302542698));
#58422=CARTESIAN_POINT('Ctrl Pts',(-0.0359120384624134,-0.823757874670842,
-2.496053655132));
#58423=CARTESIAN_POINT('Ctrl Pts',(0.361876488438089,-0.740886035571238,
-2.48020428483702));
#58424=CARTESIAN_POINT('Ctrl Pts',(0.671784468788094,-0.478092394923669,
-2.46435491454204));
#58425=CARTESIAN_POINT('Ctrl Pts',(0.818551741832004,-0.0991955469390545,
-2.44850554424706));
#58426=CARTESIAN_POINT('Ctrl Pts',(0.76653634523485,0.303790622012513,-2.43265617395208));
#58427=CARTESIAN_POINT('Ctrl Pts',(0.528370051515826,0.633002211094015,
-2.4168068036571));
#58428=CARTESIAN_POINT('Ctrl Pts',(0.161890782536823,0.808491239976267,
-2.40095743336211));
#58429=CARTESIAN_POINT('Ctrl Pts',(-0.243903144634621,0.78764075988111,
-2.38510806306714));
#58430=CARTESIAN_POINT('Ctrl Pts',(-0.590465974067748,0.575514243139972,
-2.36925869277216));
#58431=CARTESIAN_POINT('Ctrl Pts',(-0.793636032269693,0.223625935150573,
-2.35340932247718));
#58432=CARTESIAN_POINT('Ctrl Pts',(-0.804074121121928,-0.182569215178101,
-2.3375599521822));
#58433=CARTESIAN_POINT('Ctrl Pts',(-0.619245384167668,-0.544428016156211,
-2.32171058188722));
#58434=CARTESIAN_POINT('Ctrl Pts',(-0.284034888386214,-0.774074216576279,
-2.30586121159224));
#58435=CARTESIAN_POINT('Ctrl Pts',(0.120152570608644,-0.815738971954194,
-2.29001184129726));
#58436=CARTESIAN_POINT('Ctrl Pts',(0.495161362539197,-0.659304129849854,
-2.27416247100227));
#58437=CARTESIAN_POINT('Ctrl Pts',(0.749921802999194,-0.342759390790666,
-2.25831310070729));
#58438=CARTESIAN_POINT('Ctrl Pts',(0.822566134722329,0.0570233688650289,
-2.24246373041231));
#58439=CARTESIAN_POINT('Ctrl Pts',(0.695452914344377,0.442958185970936,
-2.22661436011733));
#58440=CARTESIAN_POINT('Ctrl Pts',(0.399451180439311,0.721322025890232,
-2.21076498982235));
#58441=CARTESIAN_POINT('Ctrl Pts',(0.0064440063389957,0.824515121371981,
-2.19491561952737));
#58442=CARTESIAN_POINT('Ctrl Pts',(-0.388128074068138,0.727477359585098,
-2.17906624923239));
#58443=CARTESIAN_POINT('Ctrl Pts',(-0.688444494407612,0.453774050281193,
-2.16321687893741));
#58444=CARTESIAN_POINT('Ctrl Pts',(-0.821574373561847,0.0698731657734796,
-2.14736750864243));
#58445=CARTESIAN_POINT('Ctrl Pts',(-0.755187546637368,-0.330996193320378,
-2.13151813834745));
#58446=CARTESIAN_POINT('Ctrl Pts',(-0.50540584199351,-0.651484186659646,
-2.11566876805247));
#58447=CARTESIAN_POINT('Ctrl Pts',(-0.132887946844688,-0.813761331209681,
-2.09981939775749));
#58448=CARTESIAN_POINT('Ctrl Pts',(0.271901360710864,-0.778419142000201,
-2.08397002746251));
#58449=CARTESIAN_POINT('Ctrl Pts',(0.610660293399487,-0.554040356521077,
-2.06812065716753));
#58450=CARTESIAN_POINT('Ctrl Pts',(0.801122329065975,-0.195114644403376,
-2.05227128687255));
#58451=CARTESIAN_POINT('Ctrl Pts',(0.797034372175622,0.211194034383928,
-2.03642191657757));
#58452=CARTESIAN_POINT('Ctrl Pts',(0.599389169970311,0.566214918128312,
-2.02057254628259));
#58453=CARTESIAN_POINT('Ctrl Pts',(0.256184226979425,0.78373232192867,-2.00472317598761));
#58454=CARTESIAN_POINT('Ctrl Pts',(-0.149234235275289,0.810922840725644,
-1.98887380569263));
#58455=CARTESIAN_POINT('Ctrl Pts',(-0.518411641315918,0.641183344088789,
-1.97302443539765));
#58456=CARTESIAN_POINT('Ctrl Pts',(-0.761694440128485,0.315734525299501,
-1.95717506510267));
#58457=CARTESIAN_POINT('Ctrl Pts',(-0.820002182971318,-0.0863894120307608,
-1.94132569480769));
#58458=CARTESIAN_POINT('Ctrl Pts',(-0.679175021186466,-0.467533957253495,
-1.92547632451271));
#58459=CARTESIAN_POINT('Ctrl Pts',(-0.373412380108861,-0.735139377921076,
-1.90962695421773));
#58460=CARTESIAN_POINT('Ctrl Pts',(0.0230322618755374,-0.824218554451213,
-1.89377758392274));
#58461=CARTESIAN_POINT('Ctrl Pts',(0.413883592808825,-0.713138894039869,
-1.87792821362777));
#58462=CARTESIAN_POINT('Ctrl Pts',(0.704224618413045,-0.428875736559846,
-1.86207884333278));
#58463=CARTESIAN_POINT('Ctrl Pts',(0.823546950242572,-0.0404614796431028,
-1.8462294730378));
#58464=CARTESIAN_POINT('Ctrl Pts',(0.742873542062324,0.357778718054223,
-1.83038010274282));
#58465=CARTESIAN_POINT('Ctrl Pts',(0.48179567274641,0.669133499618412,-1.81453073244784));
#58466=CARTESIAN_POINT('Ctrl Pts',(0.103715266931461,0.817991353251417,
-1.79868136215286));
#58467=CARTESIAN_POINT('Ctrl Pts',(-0.299552059379227,0.768202625815879,
-1.78283199185788));
#58468=CARTESIAN_POINT('Ctrl Pts',(-0.630074127184189,0.531858350354521,
-1.7669826215629));
#58469=CARTESIAN_POINT('Ctrl Pts',(-0.807584710592181,0.166353977429135,
-1.75113325126792));
#58470=CARTESIAN_POINT('Ctrl Pts',(-0.78897593278113,-0.239548926277902,
-1.73528388097294));
#58471=CARTESIAN_POINT('Ctrl Pts',(-0.578766875860324,-0.587278140233081,
-1.71943451067796));
#58472=CARTESIAN_POINT('Ctrl Pts',(-0.228006136249502,-0.792388738196929,
-1.70358514038298));
#58473=CARTESIAN_POINT('Ctrl Pts',(0.178125163512817,-0.80507026818302,
-1.687735770088));
#58474=CARTESIAN_POINT('Ctrl Pts',(0.540999337642394,-0.622243061238324,
-1.67188639979302));
#58475=CARTESIAN_POINT('Ctrl Pts',(0.77249355481297,-0.288306119187871,
-1.65603702949804));
#58476=CARTESIAN_POINT('Ctrl Pts',(0.816390185589599,0.115645040800419,
-1.64018765920306));
#58477=CARTESIAN_POINT('Ctrl Pts',(0.662029073737689,0.491512172905988,
-1.62433828890808));
#58478=CARTESIAN_POINT('Ctrl Pts',(0.346896321032574,0.748017147559341,
-1.6084889186131));
#58479=CARTESIAN_POINT('Ctrl Pts',(-0.0524790925325479,0.822868552951023,
-1.59263954831812));
#58480=CARTESIAN_POINT('Ctrl Pts',(-0.439110126505229,0.697888964943071,
-1.57679017802314));
#58481=CARTESIAN_POINT('Ctrl Pts',(-0.71910467221172,0.40342927631993,-1.56094080772816));
#58482=CARTESIAN_POINT('Ctrl Pts',(-0.824466950721903,0.010998079654113,
-1.54509143743318));
#58483=CARTESIAN_POINT('Ctrl Pts',(-0.729610070051588,-0.384103965441732,
-1.5292420671382));
#58484=CARTESIAN_POINT('Ctrl Pts',(-0.457569719956044,-0.68592759236533,
-1.51339269684322));
#58485=CARTESIAN_POINT('Ctrl Pts',(-0.0744100284292379,-0.82117589970597,
-1.49754332654823));
#58486=CARTESIAN_POINT('Ctrl Pts',(0.326819900253411,-0.75700426906795,
-1.48169395625326));
#58487=CARTESIAN_POINT('Ctrl Pts',(0.648682662580996,-0.508996575485116,
-1.46584458595827));
#58488=CARTESIAN_POINT('Ctrl Pts',(0.813014917271852,-0.137380693265803,
-1.44999521566329));
#58489=CARTESIAN_POINT('Ctrl Pts',(0.779909102438105,0.267597650443601,
-1.43414584536831));
#58490=CARTESIAN_POINT('Ctrl Pts',(0.557404859212971,0.607590761544741,
-1.41829647507333));
#58491=CARTESIAN_POINT('Ctrl Pts',(0.19953663064309,0.800032401606555,-1.40244710477835));
#58492=CARTESIAN_POINT('Ctrl Pts',(-0.206788429796264,0.798188734505283,
-1.38659773448337));
#58493=CARTESIAN_POINT('Ctrl Pts',(-0.562895582160815,0.602507488893362,
-1.37074836418839));
#58494=CARTESIAN_POINT('Ctrl Pts',(-0.782305344693098,0.260509228729736,
-1.35489899389341));
#58495=CARTESIAN_POINT('Ctrl Pts',(-0.811734759074724,-0.144752863524866,
-1.33904962359843));
#58496=CARTESIAN_POINT('Ctrl Pts',(-0.644036986251071,-0.51486218634639,
-1.32320025330345));
#58497=CARTESIAN_POINT('Ctrl Pts',(-0.319936893412746,-0.759938875714455,
-1.30735088300847));
#58498=CARTESIAN_POINT('Ctrl Pts',(0.0818588496075917,-0.820466842309713,
-1.29150151271349));
#58499=CARTESIAN_POINT('Ctrl Pts',(0.463775433098776,-0.681747063244712,
-1.27565214241851));
#58500=CARTESIAN_POINT('Ctrl Pts',(0.733065637591628,-0.377467192708359,
-1.25980277212353));
#58501=CARTESIAN_POINT('Ctrl Pts',(0.824333199146284,0.0184793769917608,
-1.24395340182855));
#58502=CARTESIAN_POINT('Ctrl Pts',(0.71541408266233,0.409938289157241,-1.22810403153357));
#58503=CARTESIAN_POINT('Ctrl Pts',(0.432758946837499,0.701845000353243,
-1.21225466123859));
#58504=CARTESIAN_POINT('Ctrl Pts',(0.0450096863933985,0.82331090040125,
-1.19640529094361));
#58505=CARTESIAN_POINT('Ctrl Pts',(-0.353670032278012,0.744838384387658,
-1.18055592064863));
#58506=CARTESIAN_POINT('Ctrl Pts',(-0.666462116001734,0.485484251570782,
-1.16470655035365));
#58507=CARTESIAN_POINT('Ctrl Pts',(-0.817406008752267,0.108231822697566,
-1.14885718005867));
#58508=CARTESIAN_POINT('Ctrl Pts',(-0.769845469471702,-0.295304357777947,
-1.13300780976369));
#58509=CARTESIAN_POINT('Ctrl Pts',(-0.535330422843599,-0.627126820481185,
-1.11715843946871));
#58510=CARTESIAN_POINT('Ctrl Pts',(-0.170812097064488,-0.806653542783506,
-1.10130906917372));
#58511=CARTESIAN_POINT('Ctrl Pts',(0.235187399575584,-0.790287034987683,
-1.08545969887875));
#58512=CARTESIAN_POINT('Ctrl Pts',(0.584072389258597,-0.582001851109171,
-1.06961032858376));
#58513=CARTESIAN_POINT('Ctrl Pts',(0.791117269310166,-0.232379381159294,
-1.05376095828878));
#58514=CARTESIAN_POINT('Ctrl Pts',(0.806041853532098,0.173675677466042,
-1.0379115879938));
#58515=CARTESIAN_POINT('Ctrl Pts',(0.625221754432068,0.537554153898595,
-1.02206221769882));
#58516=CARTESIAN_POINT('Ctrl Pts',(0.292568554121453,0.77088932521344,-1.00621284740384));
#58517=CARTESIAN_POINT('Ctrl Pts',(-0.111133982803035,0.817016492156116,
-0.990363477108863));
#58518=CARTESIAN_POINT('Ctrl Pts',(-0.487847987835832,0.664733819925901,
-0.974514106813882));
#58519=CARTESIAN_POINT('Ctrl Pts',(-0.746089671028602,0.351022667890806,
-0.958664736518902));
#58520=CARTESIAN_POINT('Ctrl Pts',(-0.82314586646374,-0.0479332151269538,
-0.942815366223922));
#58521=CARTESIAN_POINT('Ctrl Pts',(-0.700303723800595,-0.435248670325099,
-0.926965995928941));
#58522=CARTESIAN_POINT('Ctrl Pts',(-0.407395064065358,-0.716865379526681,
-0.911116625633962));
#58523=CARTESIAN_POINT('Ctrl Pts',(-0.0155518174312369,-0.824393626590682,
-0.89526725533898));
#58524=CARTESIAN_POINT('Ctrl Pts',(0.380068138271797,-0.731720521004679,
-0.879417885044));
#58525=CARTESIAN_POINT('Ctrl Pts',(0.683389763508767,-0.461351429736789,
-0.86356851474902));
#58526=CARTESIAN_POINT('Ctrl Pts',(0.820752372774903,-0.0789446209257793,
-0.84771914445404));
#58527=CARTESIAN_POINT('Ctrl Pts',(0.758797896221531,0.322633636309872,
-0.831869774159059));
#58528=CARTESIAN_POINT('Ctrl Pts',(0.51257178011198,0.645861347985452,-0.816020403864079));
#58529=CARTESIAN_POINT('Ctrl Pts',(0.141869248369509,0.812243699240455,
-0.800171033569098));
#58530=CARTESIAN_POINT('Ctrl Pts',(-0.263285776098399,0.781375268800473,
-0.784321663274118));
#58531=CARTESIAN_POINT('Ctrl Pts',(-0.604502692836885,0.560752356162417,
-0.768472292979138));
#58532=CARTESIAN_POINT('Ctrl Pts',(-0.798918066134286,0.20395252926356,
-0.752622922684157));
#58533=CARTESIAN_POINT('Ctrl Pts',(-0.799318745070129,-0.202376516345802,
-0.736773552389177));
#58534=CARTESIAN_POINT('Ctrl Pts',(-0.605607426047752,-0.559559072935617,
-0.720924182094196));
#58535=CARTESIAN_POINT('Ctrl Pts',(-0.264826282661191,-0.780854500275564,
-0.705074811799216));
#58536=CARTESIAN_POINT('Ctrl Pts',(0.140267075541125,-0.812521912386299,
-0.689225441504235));
#58537=CARTESIAN_POINT('Ctrl Pts',(0.511297023559492,-0.646870979630369,
-0.673376071209255));
#58538=CARTESIAN_POINT('Ctrl Pts',(0.758160126492153,-0.324129500641566,
-0.657526700914275));
#58539=CARTESIAN_POINT('Ctrl Pts',(0.820906470205391,0.0773257897707563,
-0.641677330619295));
#58540=CARTESIAN_POINT('Ctrl Pts',(0.684298306031528,0.460002759721218,
-0.625827960324314));
#58541=CARTESIAN_POINT('Ctrl Pts',(0.381510489244155,0.730969532323631,
-0.609978590029333));
#58542=CARTESIAN_POINT('Ctrl Pts',(-0.0139259283247104,0.824422694440805,
-0.594129219734354));
#58543=CARTESIAN_POINT('Ctrl Pts',(-0.405980478788452,0.717667444873665,
-0.578279849439372));
#58544=CARTESIAN_POINT('Ctrl Pts',(-0.699443969858383,0.43662895416746,
-0.562430479144393));
#58545=CARTESIAN_POINT('Ctrl Pts',(-0.823049732348623,0.0495565199530879,
-0.546581108849411));
#58546=CARTESIAN_POINT('Ctrl Pts',(-0.746780502601991,-0.349550556460541,
-0.530731738554432));
#58547=CARTESIAN_POINT('Ctrl Pts',(-0.489158018863314,-0.663770399438569,
-0.514882368259451));
#58548=CARTESIAN_POINT('Ctrl Pts',(-0.112745076441616,-0.816795726192998,
-0.499032997964471));
#58549=CARTESIAN_POINT('Ctrl Pts',(0.291047646798618,-0.771464826080581,
-0.48318362766949));
#58550=CARTESIAN_POINT('Ctrl Pts',(0.624160380908134,-0.5387861630555,-0.46733425737451));
#58551=CARTESIAN_POINT('Ctrl Pts',(0.805697764950427,-0.175265005428866,
-0.45148488707953));
#58552=CARTESIAN_POINT('Ctrl Pts',(0.791574026517504,0.230818697588217,
-0.435635516784549));
#58553=CARTESIAN_POINT('Ctrl Pts',(0.58521907015831,0.580848818956341,-0.419786146489568));
#58554=CARTESIAN_POINT('Ctrl Pts',(0.236745536522281,0.789821664383754,
-0.403936776194589));
#58555=CARTESIAN_POINT('Ctrl Pts',(-0.169220892912897,0.806988847559813,
-0.388087405899608));
#58556=CARTESIAN_POINT('Ctrl Pts',(-0.534092569784946,0.628181372808885,
-0.372238035604628));
#58557=CARTESIAN_POINT('Ctrl Pts',(-0.769261577206937,0.29682206327007,
-0.356388665309647));
#58558=CARTESIAN_POINT('Ctrl Pts',(-0.817617871593714,-0.106619534487822,
-0.340539295014668));
#58559=CARTESIAN_POINT('Ctrl Pts',(-0.667418287760902,-0.484168918639777,
-0.324689924719686));
#58560=CARTESIAN_POINT('Ctrl Pts',(-0.355138301822955,-0.744139433149644,
-0.308840554424707));
#58561=CARTESIAN_POINT('Ctrl Pts',(0.04338586818354,-0.823398064963412,
-0.292991184129725));
#58562=CARTESIAN_POINT('Ctrl Pts',(0.431373949250341,-0.702697120842669,
-0.277141813834746));
#58563=CARTESIAN_POINT('Ctrl Pts',(0.714604188710661,-0.411348415639086,
-0.261292443539765));
#58564=CARTESIAN_POINT('Ctrl Pts',(0.824295204963726,-0.0201050945398566,
-0.245443073244786));
#58565=CARTESIAN_POINT('Ctrl Pts',(0.733808542786668,0.376020742711894,
-0.229593702949804));
#58566=CARTESIAN_POINT('Ctrl Pts',(0.465119270428469,0.68083103233261,-0.213744332654824));
#58567=CARTESIAN_POINT('Ctrl Pts',(0.0834764010975726,0.820303909360284,
-0.197894962359843));
#58568=CARTESIAN_POINT('Ctrl Pts',(-0.318436738291248,0.760568170329218,
-0.182045592064863));
#58569=CARTESIAN_POINT('Ctrl Pts',(-0.643021878040478,0.516131744494383,
-0.166196221769882));
#58570=CARTESIAN_POINT('Ctrl Pts',(-0.811444666397369,0.146352696178963,
-0.150346851474902));
#58571=CARTESIAN_POINT('Ctrl Pts',(-0.782823541642527,-0.258964342128821,
-0.134497481179922));
#58572=CARTESIAN_POINT('Ctrl Pts',(-0.564071074017912,-0.601399186478657,
-0.118648110884941));
#58573=CARTESIAN_POINT('Ctrl Pts',(-0.20838535721098,-0.797773318333574,
-0.102798740589961));
#58574=CARTESIAN_POINT('Ctrl Pts',(0.198006948556336,-0.800437851012032,
-0.0869493702949813));
#58575=CARTESIAN_POINT('Ctrl Pts',(0.436718461990072,-0.672574504136354,
-0.0763831234316606));
#58576=CARTESIAN_POINT('Ctrl Pts',(0.533647856309012,-0.584002718706682,
-0.0711000000000004));
#58577=CARTESIAN_POINT('Ctrl Pts',(0.437168237015815,-0.613060138694073,
-3.8529325805302));
#58578=CARTESIAN_POINT('Ctrl Pts',(0.538920413882899,-0.540501482591816,
-3.84764945709854));
#58579=CARTESIAN_POINT('Ctrl Pts',(0.705499406799793,-0.343817992754132,
-3.83708321023521));
#58580=CARTESIAN_POINT('Ctrl Pts',(0.784016863165969,0.0349405160846657,
-3.82123383994024));
#58581=CARTESIAN_POINT('Ctrl Pts',(0.672143448857669,0.405114550572477,
-3.80538446964525));
#58582=CARTESIAN_POINT('Ctrl Pts',(0.397040081409184,0.676956541024866,
-3.78953509935027));
#58583=CARTESIAN_POINT('Ctrl Pts',(0.0255178075451435,0.784377104906589,
-3.7736857290553));
#58584=CARTESIAN_POINT('Ctrl Pts',(-0.352201893258571,0.701326793874043,
-3.75783635876031));
#58585=CARTESIAN_POINT('Ctrl Pts',(-0.644390232474814,0.447955088053146,
-3.74198698846533));
#58586=CARTESIAN_POINT('Ctrl Pts',(-0.780090599417017,0.0858022054224701,
-3.72613761817035));
#58587=CARTESIAN_POINT('Ctrl Pts',(-0.726348394383058,-0.297189143787908,
-3.71028824787537));
#58588=CARTESIAN_POINT('Ctrl Pts',(-0.49621484194368,-0.608008205401332,
-3.69443887758039));
#58589=CARTESIAN_POINT('Ctrl Pts',(-0.145577086304834,-0.771174857906999,
-3.67858950728541));
#58590=CARTESIAN_POINT('Ctrl Pts',(0.240413589629476,-0.747063942303056,
-3.66274013699043));
#58591=CARTESIAN_POINT('Ctrl Pts',(0.568020599681037,-0.541531054158926,
-3.64689076669545));
#58592=CARTESIAN_POINT('Ctrl Pts',(0.757685623458616,-0.204489025259539,
-3.63104139640047));
#58593=CARTESIAN_POINT('Ctrl Pts',(0.76334912075718,0.182212478999042,-3.61519202610549));
#58594=CARTESIAN_POINT('Ctrl Pts',(0.58363572758167,0.524664281302926,-3.59934265581051));
#58595=CARTESIAN_POINT('Ctrl Pts',(0.26218826697714,0.739703035039015,-3.58349328551553));
#58596=CARTESIAN_POINT('Ctrl Pts',(-0.122930774940204,0.775107279069842,
-3.56764391522055));
#58597=CARTESIAN_POINT('Ctrl Pts',(-0.478196471685247,0.622279200122251,
-3.55179454492557));
#58598=CARTESIAN_POINT('Ctrl Pts',(-0.717333686426498,0.318332610886684,
-3.53594517463059));
#58599=CARTESIAN_POINT('Ctrl Pts',(-0.782268712177764,-0.0629200341819831,
-3.52009580433561));
#58600=CARTESIAN_POINT('Ctrl Pts',(-0.657232285878265,-0.428892750140244,
-3.50424643404063));
#58601=CARTESIAN_POINT('Ctrl Pts',(-0.37258910329319,-0.690710235105353,
-3.48839706374565));
#58602=CARTESIAN_POINT('Ctrl Pts',(0.00253615005715591,-0.784790950941299,
-3.47254769345067));
#58603=CARTESIAN_POINT('Ctrl Pts',(0.377045507487883,-0.688287697143436,
-3.45669832315569));
#58604=CARTESIAN_POINT('Ctrl Pts',(0.659990570659741,-0.424635979855658,
-3.44084895286071));
#58605=CARTESIAN_POINT('Ctrl Pts',(0.782659036924308,-0.0578627744811105,
-3.42499958256572));
#58606=CARTESIAN_POINT('Ctrl Pts',(0.715261262012136,0.322962220414213,
-3.40915021227075));
#58607=CARTESIAN_POINT('Ctrl Pts',(0.474164579764779,0.625356874149369,
-3.39330084197576));
#58608=CARTESIAN_POINT('Ctrl Pts',(0.11791854751547,0.775885613284464,-3.37745147168079));
#58609=CARTESIAN_POINT('Ctrl Pts',(-0.266963626442902,0.73799301548597,
-3.3616021013858));
#58610=CARTESIAN_POINT('Ctrl Pts',(-0.58701453849155,0.520881176804586,
-3.34575273109083));
#58611=CARTESIAN_POINT('Ctrl Pts',(-0.764510849387783,0.17727501210858,
-3.32990336079584));
#58612=CARTESIAN_POINT('Ctrl Pts',(-0.756348148343323,-0.209381821673607,
-3.31405399050086));
#58613=CARTESIAN_POINT('Ctrl Pts',(-0.564508721171237,-0.545190950467224,
-3.29820462020588));
#58614=CARTESIAN_POINT('Ctrl Pts',(-0.235580158523199,-0.748602202548133,
-3.2823552499109));
#58615=CARTESIAN_POINT('Ctrl Pts',(0.150558291334779,-0.770217806636597,
-3.26650587961592));
#58616=CARTESIAN_POINT('Ctrl Pts',(0.500134142204031,-0.604788482489186,
-3.25065650932094));
#58617=CARTESIAN_POINT('Ctrl Pts',(0.728254017983114,-0.292488211798675,
-3.23480713902596));
#58618=CARTESIAN_POINT('Ctrl Pts',(0.779519737239942,0.0908418846298628,
-3.21895776873098));
#58619=CARTESIAN_POINT('Ctrl Pts',(0.641481584197075,0.452111320236231,
-3.203108398436));
#58620=CARTESIAN_POINT('Ctrl Pts',(0.347661682346383,0.703586969306436,
-3.18725902814102));
#58621=CARTESIAN_POINT('Ctrl Pts',(-0.030586745908813,0.784198775645847,
-3.17140965784604));
#58622=CARTESIAN_POINT('Ctrl Pts',(-0.401407280853592,0.674370420190166,
-3.15556028755106));
#58623=CARTESIAN_POINT('Ctrl Pts',(-0.674747342880608,0.400773367410177,
-3.13971091725608));
#58624=CARTESIAN_POINT('Ctrl Pts',(-0.784227173114788,0.0298497855624786,
-3.1238615469611));
#58625=CARTESIAN_POINT('Ctrl Pts',(-0.703259945319463,-0.348322721135155,
-3.10801217666612));
#58626=CARTESIAN_POINT('Ctrl Pts',(-0.451508291521506,-0.641906170274961,
-3.09216280637114));
#58627=CARTESIAN_POINT('Ctrl Pts',(-0.0901092947799612,-0.77960476123738,
-3.07631343607616));
#58628=CARTESIAN_POINT('Ctrl Pts',(0.293172455684328,-0.727978832094557,
-3.06046406578118));
#58629=CARTESIAN_POINT('Ctrl Pts',(0.605258213973796,-0.49956557444142,
-3.0446146954862));
#58630=CARTESIAN_POINT('Ctrl Pts',(0.770358952933123,-0.149834416558805,
-3.02876532519122));
#58631=CARTESIAN_POINT('Ctrl Pts',(0.748380486730397,0.236283549640911,
-3.01291595489624));
#58632=CARTESIAN_POINT('Ctrl Pts',(0.544660215511656,0.565020812349893,
-2.99706658460126));
#58633=CARTESIAN_POINT('Ctrl Pts',(0.208670954864866,0.756544579879811,
-2.98121721430628));
#58634=CARTESIAN_POINT('Ctrl Pts',(-0.177993379042111,0.764343918512411,
-2.96536784401129));
#58635=CARTESIAN_POINT('Ctrl Pts',(-0.521432590753099,0.586524783832913,
-2.94951847371632));
#58636=CARTESIAN_POINT('Ctrl Pts',(-0.738243567337769,0.266269983351747,
-2.93366910342133));
#58637=CARTESIAN_POINT('Ctrl Pts',(-0.775774457324241,-0.118647630035396,
-2.91781973312635));
#58638=CARTESIAN_POINT('Ctrl Pts',(-0.624911004246794,-0.474752046357884,
-2.90197036283137));
#58639=CARTESIAN_POINT('Ctrl Pts',(-0.322289914646288,-0.715564448297303,
-2.88612099253639));
#58640=CARTESIAN_POINT('Ctrl Pts',(0.0585982488088245,-0.782604315082835,
-2.87027162224141));
#58641=CARTESIAN_POINT('Ctrl Pts',(0.425256015162297,-0.659591229715815,
-2.85442225194643));
#58642=CARTESIAN_POINT('Ctrl Pts',(0.688641719830713,-0.376398526110735,
-2.83857288165145));
#58643=CARTESIAN_POINT('Ctrl Pts',(0.784792987751374,-0.00179864560344054,
-2.82272351135647));
#58644=CARTESIAN_POINT('Ctrl Pts',(0.690359791369684,0.373238030229693,
-2.80687414106149));
#58645=CARTESIAN_POINT('Ctrl Pts',(0.428274930067974,0.657635045465955,
-2.79102477076651));
#58646=CARTESIAN_POINT('Ctrl Pts',(0.0621848732624137,0.782327495545869,
-2.77517540047153));
#58647=CARTESIAN_POINT('Ctrl Pts',(-0.319006580909582,0.717034218211455,
-2.75932603017655));
#58648=CARTESIAN_POINT('Ctrl Pts',(-0.62272830831226,0.477611476805454,
-2.74347665988157));
#58649=CARTESIAN_POINT('Ctrl Pts',(-0.775222459910957,0.122202317487599,
-2.72762728958659));
#58650=CARTESIAN_POINT('Ctrl Pts',(-0.739456319250153,-0.262883283361178,
-2.71177791929161));
#58651=CARTESIAN_POINT('Ctrl Pts',(-0.524115579072248,-0.584128520553051,
-2.69592854899663));
#58652=CARTESIAN_POINT('Ctrl Pts',(-0.181495048645192,-0.763520016808344,
-2.68007917870165));
#58653=CARTESIAN_POINT('Ctrl Pts',(0.205200973229211,-0.757493121642381,
-2.66422980840667));
#58654=CARTESIAN_POINT('Ctrl Pts',(0.542064595773359,-0.567511447249129,
-2.64838043811169));
#58655=CARTESIAN_POINT('Ctrl Pts',(0.747289566832173,-0.239711434966122,
-2.63253106781671));
#58656=CARTESIAN_POINT('Ctrl Pts',(0.771037659279318,0.146301731783345,
-2.61668169752172));
#58657=CARTESIAN_POINT('Ctrl Pts',(0.607541724901335,0.49678599140238,-2.60083232722675));
#58658=CARTESIAN_POINT('Ctrl Pts',(0.296506227875872,0.726627363633215,
-2.58498295693176));
#58659=CARTESIAN_POINT('Ctrl Pts',(-0.0865348572269629,0.780009607142402,
-2.56913358663679));
#58660=CARTESIAN_POINT('Ctrl Pts',(-0.448561229322056,0.643969015014557,
-2.5532842163418));
#58661=CARTESIAN_POINT('Ctrl Pts',(-0.701655943092713,0.351542609469197,
-2.53743484604683));
#58662=CARTESIAN_POINT('Ctrl Pts',(-0.784355757665757,-0.0262547932063836,
-2.52158547575184));
#58663=CARTESIAN_POINT('Ctrl Pts',(-0.676577287862808,-0.397676303415155,
-2.50573610545686));
#58664=CARTESIAN_POINT('Ctrl Pts',(-0.404494189987261,-0.67252339663114,
-2.48988673516188));
#58665=CARTESIAN_POINT('Ctrl Pts',(-0.0341809731945969,-0.78405033628027,
-2.4740373648669));
#58666=CARTESIAN_POINT('Ctrl Pts',(0.344432983496739,-0.705173162158963,
-2.45818799457192));
#58667=CARTESIAN_POINT('Ctrl Pts',(0.639402492961459,-0.455046943451341,
-2.44233862427694));
#58668=CARTESIAN_POINT('Ctrl Pts',(0.779095154268031,-0.0944140315091314,
-2.42648925398196));
#58669=CARTESIAN_POINT('Ctrl Pts',(0.729587051890194,0.289147025687472,
-2.41063988368698));
#58670=CARTESIAN_POINT('Ctrl Pts',(0.502901069973915,0.602489653495249,
-2.394790513392));
#58671=CARTESIAN_POINT('Ctrl Pts',(0.154087173417781,0.769519598020644,
-2.37894114309702));
#58672=CARTESIAN_POINT('Ctrl Pts',(-0.232146299842057,0.74967417203701,
-2.36309177280204));
#58673=CARTESIAN_POINT('Ctrl Pts',(-0.562003787478044,0.547772773702808,
-2.34724240250706));
#58674=CARTESIAN_POINT('Ctrl Pts',(-0.7553804547651,0.212846511149716,-2.33139303221208));
#58675=CARTESIAN_POINT('Ctrl Pts',(-0.765315397211613,-0.17376884513792,
-2.3155436619171));
#58676=CARTESIAN_POINT('Ctrl Pts',(-0.589395945854437,-0.518184993761964,
-2.29969429162212));
#58677=CARTESIAN_POINT('Ctrl Pts',(-0.270343576191636,-0.736761575790739,
-2.28384492132714));
#58678=CARTESIAN_POINT('Ctrl Pts',(0.11436086535536,-0.776417968123425,
-2.26799555103216));
#58679=CARTESIAN_POINT('Ctrl Pts',(0.47129313691476,-0.627523742855025,
-2.25214618073718));
#58680=CARTESIAN_POINT('Ctrl Pts',(0.713773379174517,-0.326237385858098,
-2.23629681044219));
#58681=CARTESIAN_POINT('Ctrl Pts',(0.78291604168216,0.0542746757380962,
-2.22044744014722));
#58682=CARTESIAN_POINT('Ctrl Pts',(0.661930050230694,0.421606306109533,
-2.20459806985223));
#58683=CARTESIAN_POINT('Ctrl Pts',(0.380196465467641,0.686552194953631,
-2.18874869955726));
#58684=CARTESIAN_POINT('Ctrl Pts',(0.00613338638989894,0.784771081476074,
-2.17289932926227));
#58685=CARTESIAN_POINT('Ctrl Pts',(-0.369419165934574,0.692410823564984,
-2.1570499589673));
#58686=CARTESIAN_POINT('Ctrl Pts',(-0.655259456628897,0.431900814132295,
-2.14120058867231));
#58687=CARTESIAN_POINT('Ctrl Pts',(-0.781972086309719,0.0665050748601965,
-2.12535121837733));
#58688=CARTESIAN_POINT('Ctrl Pts',(-0.71878529857125,-0.31504120890381,
-2.10950184808236));
#58689=CARTESIAN_POINT('Ctrl Pts',(-0.481043802502479,-0.620080743793654,
-2.09365247778737));
#58690=CARTESIAN_POINT('Ctrl Pts',(-0.126482359216051,-0.774535655445814,
-2.07780310749239));
#58691=CARTESIAN_POINT('Ctrl Pts',(0.258794920031087,-0.740897063103801,
-2.06195373719741));
#58692=CARTESIAN_POINT('Ctrl Pts',(0.581224681565798,-0.527333991212848,
-2.04610436690243));
#58693=CARTESIAN_POINT('Ctrl Pts',(0.762505890164385,-0.185709547989203,
-2.03025499660745));
#58694=CARTESIAN_POINT('Ctrl Pts',(0.758614984750142,0.201013864353375,
-2.01440562631247));
#58695=CARTESIAN_POINT('Ctrl Pts',(0.570496859244902,0.538921703349788,
-1.99855625601749));
#58696=CARTESIAN_POINT('Ctrl Pts',(0.243835398105513,0.745954132222929,
-1.98270688572251));
#58697=CARTESIAN_POINT('Ctrl Pts',(-0.142040708744516,0.771833988503416,
-1.96685751542753));
#58698=CARTESIAN_POINT('Ctrl Pts',(-0.493422684266016,0.610276431956415,
-1.95100814513255));
#58699=CARTESIAN_POINT('Ctrl Pts',(-0.724978540768651,0.300515197909675,
-1.93515877483757));
#58700=CARTESIAN_POINT('Ctrl Pts',(-0.78047567990305,-0.0822251897511038,
-1.91930940454259));
#58701=CARTESIAN_POINT('Ctrl Pts',(-0.646436799122784,-0.444997453351843,
-1.90346003424761));
#58702=CARTESIAN_POINT('Ctrl Pts',(-0.355412811455735,-0.699703510211908,
-1.88761066395263));
#58703=CARTESIAN_POINT('Ctrl Pts',(0.0219220395022374,-0.784488809948108,
-1.87176129365765));
#58704=CARTESIAN_POINT('Ctrl Pts',(0.393933193357716,-0.67876351398755,
-1.85591192336267));
#58705=CARTESIAN_POINT('Ctrl Pts',(0.670278932513053,-0.408202671939927,
-1.84006255306768));
#58706=CARTESIAN_POINT('Ctrl Pts',(0.783849579026228,-0.038511118006908,
-1.82421318277271));
#58707=CARTESIAN_POINT('Ctrl Pts',(0.707064865025314,0.340532737628068,
-1.80836381247773));
#58708=CARTESIAN_POINT('Ctrl Pts',(0.458571712453908,0.636879308257715,
-1.79251444218274));
#58709=CARTESIAN_POINT('Ctrl Pts',(0.098715887781345,0.778561778055715,
-1.77666507188777));
#58710=CARTESIAN_POINT('Ctrl Pts',(-0.285112774167507,0.731173012874683,
-1.76081570159278));
#58711=CARTESIAN_POINT('Ctrl Pts',(-0.599702711792176,0.506221222608107,
-1.74496633129781));
#58712=CARTESIAN_POINT('Ctrl Pts',(-0.768656766003741,0.158335229265017,
-1.72911696100282));
#58713=CARTESIAN_POINT('Ctrl Pts',(-0.750944985698939,-0.22800196754273,
-1.71326759070784));
#58714=CARTESIAN_POINT('Ctrl Pts',(-0.550868620014696,-0.558969616556067,
-1.69741822041286));
#58715=CARTESIAN_POINT('Ctrl Pts',(-0.217015573747099,-0.754193283913979,
-1.68156885011788));
#58716=CARTESIAN_POINT('Ctrl Pts',(0.16953900975819,-0.766263527071429,
-1.6657194798229));
#58717=CARTESIAN_POINT('Ctrl Pts',(0.514921587578651,-0.592249126124486,
-1.64987010952792));
#58718=CARTESIAN_POINT('Ctrl Pts',(0.73525710654659,-0.274408921178727,
-1.63402073923294));
#58719=CARTESIAN_POINT('Ctrl Pts',(0.777037791357327,0.110070611664803,
-1.61817136893796));
#58720=CARTESIAN_POINT('Ctrl Pts',(0.630117336479189,0.467819848892825,
-1.60232199864298));
#58721=CARTESIAN_POINT('Ctrl Pts',(0.330174903965143,0.711960533696457,
-1.586472628348));
#58722=CARTESIAN_POINT('Ctrl Pts',(-0.0499494468132064,0.783203882467899,
-1.57062325805302));
#58723=CARTESIAN_POINT('Ctrl Pts',(-0.417943734362563,0.664248676067036,
-1.55477388775804));
#58724=CARTESIAN_POINT('Ctrl Pts',(-0.684441724206405,0.383982805494072,
-1.53892451746306));
#58725=CARTESIAN_POINT('Ctrl Pts',(-0.784725232792191,0.0104679400542139,
-1.52307514716808));
#58726=CARTESIAN_POINT('Ctrl Pts',(-0.694440731150519,-0.365589031111253,
-1.5072257768731));
#58727=CARTESIAN_POINT('Ctrl Pts',(-0.435513521429528,-0.652863876624973,
-1.49137640657812));
#58728=CARTESIAN_POINT('Ctrl Pts',(-0.0708232474692601,-0.781592820058913,
-1.47552703628314));
#58729=CARTESIAN_POINT('Ctrl Pts',(0.311066225374979,-0.72051444966822,
-1.45967766598816));
#58730=CARTESIAN_POINT('Ctrl Pts',(0.617414261367809,-0.484461452139772,
-1.44382829569317));
#58731=CARTESIAN_POINT('Ctrl Pts',(0.77382522084245,-0.130758542121987,
-1.4279789253982));
#58732=CARTESIAN_POINT('Ctrl Pts',(0.742315203091658,0.254698661183609,
-1.41212955510321));
#58733=CARTESIAN_POINT('Ctrl Pts',(0.53053631503652,0.578303110122371,-1.39628018480824));
#58734=CARTESIAN_POINT('Ctrl Pts',(0.189918381561399,0.761468500395673,
-1.38043081451325));
#58735=CARTESIAN_POINT('Ctrl Pts',(-0.196820622789698,0.759713703439929,
-1.36458144421828));
#58736=CARTESIAN_POINT('Ctrl Pts',(-0.53576236908232,0.57346486607728,-1.34873207392329));
#58737=CARTESIAN_POINT('Ctrl Pts',(-0.744595939462876,0.247951922124295,
-1.33288270362831));
#58738=CARTESIAN_POINT('Ctrl Pts',(-0.772606770013859,-0.137775352216883,
-1.31703333333333));
#58739=CARTESIAN_POINT('Ctrl Pts',(-0.612992520221859,-0.49004432340533,
-1.30118396303835));
#58740=CARTESIAN_POINT('Ctrl Pts',(-0.304514999591304,-0.723307599692996,
-1.28533459274337));
#58741=CARTESIAN_POINT('Ctrl Pts',(0.0779130136849949,-0.780917941302578,
-1.26948522244839));
#58742=CARTESIAN_POINT('Ctrl Pts',(0.441420101052052,-0.648884861232661,
-1.25363585215341));
#58743=CARTESIAN_POINT('Ctrl Pts',(0.697729730230368,-0.359272170230862,
-1.23778648185843));
#58744=CARTESIAN_POINT('Ctrl Pts',(0.784597928433633,0.0175886169833986,
-1.22193711156345));
#58745=CARTESIAN_POINT('Ctrl Pts',(0.680929031865307,0.390178064878987,
-1.20608774126847));
#58746=CARTESIAN_POINT('Ctrl Pts',(0.41189870012692,0.668014019002212,-1.19023837097349));
#58747=CARTESIAN_POINT('Ctrl Pts',(0.042840087891981,0.783624907477514,
-1.17438900067851));
#58748=CARTESIAN_POINT('Ctrl Pts',(-0.336622102520883,0.708934996204979,
-1.15853963038353));
#58749=CARTESIAN_POINT('Ctrl Pts',(-0.634336693143016,0.462082490992808,
-1.14269026008855));
#58750=CARTESIAN_POINT('Ctrl Pts',(-0.778004648873088,0.103014732352219,
-1.12684088979357));
#58751=CARTESIAN_POINT('Ctrl Pts',(-0.732736666662294,-0.281069824204532,
-1.11099151949859));
#58752=CARTESIAN_POINT('Ctrl Pts',(-0.509525931050183,-0.596897473890766,
-1.09514214920361));
#58753=CARTESIAN_POINT('Ctrl Pts',(-0.162578454497519,-0.767770483206364,
-1.07929277890863));
#58754=CARTESIAN_POINT('Ctrl Pts',(0.223850679181434,-0.752192888945213,
-1.06344340861365));
#58755=CARTESIAN_POINT('Ctrl Pts',(0.555918392152804,-0.55394765999684,
-1.04759403831867));
#58756=CARTESIAN_POINT('Ctrl Pts',(0.752983103545585,-0.221178015464003,
-1.03174466802369));
#58757=CARTESIAN_POINT('Ctrl Pts',(0.767188279165573,0.165304001950049,
-1.01589529772871));
#58758=CARTESIAN_POINT('Ctrl Pts',(0.595084237596002,0.511642471765704,
-1.00004592743373));
#58759=CARTESIAN_POINT('Ctrl Pts',(0.278465894284304,0.733730205504842,
-0.984196557138746));
#58760=CARTESIAN_POINT('Ctrl Pts',(-0.105776999854121,0.777633908115894,
-0.968347186843765));
#58761=CARTESIAN_POINT('Ctrl Pts',(-0.464332288257856,0.632691705991915,
-0.952497816548785));
#58762=CARTESIAN_POINT('Ctrl Pts',(-0.710125967170823,0.334102348838551,
-0.936648446253805));
#58763=CARTESIAN_POINT('Ctrl Pts',(-0.783467828658384,-0.0456226939916094,
-0.920799075958824));
#58764=CARTESIAN_POINT('Ctrl Pts',(-0.666547036486394,-0.414268411661978,
-0.904949705663843));
#58765=CARTESIAN_POINT('Ctrl Pts',(-0.387757430673421,-0.68231037197692,
-0.889100335368864));
#58766=CARTESIAN_POINT('Ctrl Pts',(-0.0148021743544479,-0.784655443098508,
-0.873250965073883));
#58767=CARTESIAN_POINT('Ctrl Pts',(0.361747742612468,-0.696449452196295,
-0.857401594778902));
#58768=CARTESIAN_POINT('Ctrl Pts',(0.650448378540411,-0.439112941740372,
-0.841552224483922));
#58769=CARTESIAN_POINT('Ctrl Pts',(0.7811897083644,-0.0751392593474202,
-0.825702854188942));
#58770=CARTESIAN_POINT('Ctrl Pts',(0.722221618748077,0.307081751594985,
-0.809853483893961));
#58771=CARTESIAN_POINT('Ctrl Pts',(0.487864321449014,0.614728942385853,
-0.794004113598982));
#58772=CARTESIAN_POINT('Ctrl Pts',(0.135030735744269,0.77309117777536,-0.778154743304));
#58773=CARTESIAN_POINT('Ctrl Pts',(-0.250594631790622,0.743710695948,-0.762305373009021));
#58774=CARTESIAN_POINT('Ctrl Pts',(-0.575363895356359,0.533722452844257,
-0.746456002714039));
#58775=CARTESIAN_POINT('Ctrl Pts',(-0.760407879151704,0.194121420955399,
-0.730606632419061));
#58776=CARTESIAN_POINT('Ctrl Pts',(-0.760789244191175,-0.192621376468859,
-0.714757262124078));
#58777=CARTESIAN_POINT('Ctrl Pts',(-0.576415377195997,-0.532586689358392,
-0.698907891829099));
#58778=CARTESIAN_POINT('Ctrl Pts',(-0.252060881432333,-0.743215029988824,
-0.683058521534118));
#58779=CARTESIAN_POINT('Ctrl Pts',(0.133505792331293,-0.773355980234025,
-0.667209151239137));
#58780=CARTESIAN_POINT('Ctrl Pts',(0.486651011890002,-0.615689906833116,
-0.651359780944158));
#58781=CARTESIAN_POINT('Ctrl Pts',(0.721614591384625,-0.30850551089168,
-0.635510410649176));
#58782=CARTESIAN_POINT('Ctrl Pts',(0.781336377848125,0.0735984605878615,
-0.619661040354197));
#58783=CARTESIAN_POINT('Ctrl Pts',(0.651313126656813,0.437829281563337,
-0.603811670059216));
#58784=CARTESIAN_POINT('Ctrl Pts',(0.36312056805023,0.695734663365716,-0.587962299764236));
#58785=CARTESIAN_POINT('Ctrl Pts',(-0.0132546578572862,0.784683109793256,
-0.572112929469256));
#58786=CARTESIAN_POINT('Ctrl Pts',(-0.386411032543397,0.683073775428778,
-0.556263559174275));
#58787=CARTESIAN_POINT('Ctrl Pts',(-0.665728725198291,0.415582161786907,
-0.540414188879295));
#58788=CARTESIAN_POINT('Ctrl Pts',(-0.783376328488732,0.0471677507782503,
-0.524564818584314));
#58789=CARTESIAN_POINT('Ctrl Pts',(-0.710783498642241,-0.332701197483979,
-0.508715448289334));
#58790=CARTESIAN_POINT('Ctrl Pts',(-0.465579171959016,-0.63177472518931,
-0.492866077994354));
#58791=CARTESIAN_POINT('Ctrl Pts',(-0.107310434068157,-0.777423783717762,
-0.477016707699373));
#58792=CARTESIAN_POINT('Ctrl Pts',(0.277018299141874,-0.734277965547306,
-0.461167337404393));
#58793=CARTESIAN_POINT('Ctrl Pts',(0.594074025379593,-0.5128150944786,-0.445317967109412));
#58794=CARTESIAN_POINT('Ctrl Pts',(0.766860776659725,-0.166816719657547,
-0.429468596814432));
#58795=CARTESIAN_POINT('Ctrl Pts',(0.753417843719877,0.219692561404809,
-0.413619226519451));
#58796=CARTESIAN_POINT('Ctrl Pts',(0.557009799680024,0.552850207365477,
-0.397769856224471));
#58797=CARTESIAN_POINT('Ctrl Pts',(0.225333709370989,0.751749950565232,
-0.381920485929491));
#58798=CARTESIAN_POINT('Ctrl Pts',(-0.16106395103904,0.768089625311954,
-0.36607111563451));
#58799=CARTESIAN_POINT('Ctrl Pts',(-0.508347746128691,0.597901193712546,
-0.35022174533953));
#58800=CARTESIAN_POINT('Ctrl Pts',(-0.732180919712112,0.282514371853855,
-0.33437237504455));
#58801=CARTESIAN_POINT('Ctrl Pts',(-0.778206299306046,-0.101480161148845,
-0.31852300474957));
#58802=CARTESIAN_POINT('Ctrl Pts',(-0.635246774627353,-0.460830560955378,
-0.302673634454589));
#58803=CARTESIAN_POINT('Ctrl Pts',(-0.33801959718024,-0.708269736460514,
-0.286824264159609));
#58804=CARTESIAN_POINT('Ctrl Pts',(0.0412945424682123,-0.783707870452892,
-0.270974893864628));
#58805=CARTESIAN_POINT('Ctrl Pts',(0.410580463473477,-0.668825064792273,
-0.255125523569648));
#58806=CARTESIAN_POINT('Ctrl Pts',(0.680158177170402,-0.39152021914091,
-0.239276153274668));
#58807=CARTESIAN_POINT('Ctrl Pts',(0.784561765681778,-0.0191359701917467,
-0.223426782979687));
#58808=CARTESIAN_POINT('Ctrl Pts',(0.698436825222601,0.357895443353941,
-0.207577412684706));
#58809=CARTESIAN_POINT('Ctrl Pts',(0.442699161492799,0.648012985689183,
-0.191728042389726));
#58810=CARTESIAN_POINT('Ctrl Pts',(0.0794525944631093,0.780762862197761,
-0.175878672094745));
#58811=CARTESIAN_POINT('Ctrl Pts',(-0.303087156333423,0.72390656046714,
-0.160029301799766));
#58812=CARTESIAN_POINT('Ctrl Pts',(-0.612026343195399,0.491252685138143,
-0.144179931504784));
#58813=CARTESIAN_POINT('Ctrl Pts',(-0.772330660651845,0.139298068258817,
-0.128330561209805));
#58814=CARTESIAN_POINT('Ctrl Pts',(-0.745089157804027,-0.246481503575108,
-0.112481190914824));
#58815=CARTESIAN_POINT('Ctrl Pts',(-0.53688119879453,-0.572409987079866,
-0.0966318206198436));
#58816=CARTESIAN_POINT('Ctrl Pts',(-0.198340573633284,-0.759318311542457,
-0.0807824503248633));
#58817=CARTESIAN_POINT('Ctrl Pts',(0.188462434624327,-0.761854405954189,
-0.0649330800298836));
#58818=CARTESIAN_POINT('Ctrl Pts',(0.415667355070738,-0.640154446295708,
-0.0543668331665629));
#58819=CARTESIAN_POINT('Ctrl Pts',(0.507924469142727,-0.555852079925217,
-0.0490837097349027));
#58820=CARTESIAN_POINT('Ctrl Pts',(0.415028236876543,-0.58201224818692,
-3.8309162902651));
#58821=CARTESIAN_POINT('Ctrl Pts',(0.511627264408289,-0.513128261285645,
-3.82563316683344));
#58822=CARTESIAN_POINT('Ctrl Pts',(0.669770011015167,-0.326405633477014,
-3.81506691997012));
#58823=CARTESIAN_POINT('Ctrl Pts',(0.744311019991775,0.0331709844364849,
-3.79921754967514));
#58824=CARTESIAN_POINT('Ctrl Pts',(0.638103336170378,0.384597881138026,
-3.78336817938015));
#58825=CARTESIAN_POINT('Ctrl Pts',(0.37693233635043,0.642672673525976,-3.76751880908518));
#58826=CARTESIAN_POINT('Ctrl Pts',(0.0242254806678254,0.74465301760688,
-3.75166943879019));
#58827=CARTESIAN_POINT('Ctrl Pts',(-0.334364938728149,0.66580871639421,
-3.73582006849522));
#58828=CARTESIAN_POINT('Ctrl Pts',(-0.611755656975627,0.425268797348251,
-3.71997069820023));
#58829=CARTESIAN_POINT('Ctrl Pts',(-0.74058359841064,0.0814568283361267,
-3.70412132790526));
#58830=CARTESIAN_POINT('Ctrl Pts',(-0.689563119994008,-0.282138261478232,
-3.68827195761027));
#58831=CARTESIAN_POINT('Ctrl Pts',(-0.471084478528582,-0.577216165604128,
-3.6724225873153));
#58832=CARTESIAN_POINT('Ctrl Pts',(-0.138204463048699,-0.732119386773014,
-3.65657321702031));
#58833=CARTESIAN_POINT('Ctrl Pts',(0.228238055230608,-0.709229547243747,
-3.64072384672533));
#58834=CARTESIAN_POINT('Ctrl Pts',(0.539253696939214,-0.514105691107978,
-3.62487447643035));
#58835=CARTESIAN_POINT('Ctrl Pts',(0.719313302716812,-0.194132858767131,
-3.60902510613537));
#58836=CARTESIAN_POINT('Ctrl Pts',(0.724689977185254,0.172984488562333,
-3.59317573584039));
#58837=CARTESIAN_POINT('Ctrl Pts',(0.55407801044707,0.498093121100594,-3.57732636554541));
#58838=CARTESIAN_POINT('Ctrl Pts',(0.248909973231426,0.702241426641804,
-3.56147699525043));
#58839=CARTESIAN_POINT('Ctrl Pts',(-0.116705054167638,0.735852653931238,
-3.54562762495545));
#58840=CARTESIAN_POINT('Ctrl Pts',(-0.453978632754447,0.590764418372731,
-3.52977825466047));
#58841=CARTESIAN_POINT('Ctrl Pts',(-0.681004953978322,0.302210936317006,
-3.51392888436549));
#58842=CARTESIAN_POINT('Ctrl Pts',(-0.742651402569929,-0.0597335044947861,
-3.49807951407051));
#58843=CARTESIAN_POINT('Ctrl Pts',(-0.62394733590063,-0.407171854741584,
-3.48223014377553));
#58844=CARTESIAN_POINT('Ctrl Pts',(-0.353719656475381,-0.655729823889253,
-3.46638077348055));
#58845=CARTESIAN_POINT('Ctrl Pts',(0.00240770897232327,-0.745045904773835,
-3.45053140318557));
#58846=CARTESIAN_POINT('Ctrl Pts',(0.357950370006541,-0.653429973227718,
-3.43468203289059));
#58847=CARTESIAN_POINT('Ctrl Pts',(0.626565929779902,-0.403130664837067,
-3.41883266259561));
#58848=CARTESIAN_POINT('Ctrl Pts',(0.743021959663633,-0.0549323652550938,
-3.40298329230063));
#58849=CARTESIAN_POINT('Ctrl Pts',(0.67903748567224,0.306606083349546,-3.38713392200565));
#58850=CARTESIAN_POINT('Ctrl Pts',(0.450150932447457,0.593686226310738,
-3.37128455171067));
#58851=CARTESIAN_POINT('Ctrl Pts',(0.111946666584141,0.736591570095416,
-3.35543518141568));
#58852=CARTESIAN_POINT('Ctrl Pts',(-0.253443488825009,0.700618009522183,
-3.33958581112071));
#58853=CARTESIAN_POINT('Ctrl Pts',(-0.557285704455768,0.494501608595965,
-3.32373644082573));
#58854=CARTESIAN_POINT('Ctrl Pts',(-0.725792871093056,0.168297075331728,
-3.30788707053075));
#58855=CARTESIAN_POINT('Ctrl Pts',(-0.718043562850171,-0.198777863818256,
-3.29203770023576));
#58856=CARTESIAN_POINT('Ctrl Pts',(-0.535919674421936,-0.51758023519278,
-3.27618832994079));
#58857=CARTESIAN_POINT('Ctrl Pts',(-0.223649408983571,-0.7106899036542,
-3.2603389596458));
#58858=CARTESIAN_POINT('Ctrl Pts',(0.142933399339255,-0.731210804520864,
-3.24448958935082));
#58859=CARTESIAN_POINT('Ctrl Pts',(0.474805289280868,-0.574159502721701,
-3.22864021905584));
#58860=CARTESIAN_POINT('Ctrl Pts',(0.691372234966041,-0.277675404047213,
-3.21279084876086));
#58861=CARTESIAN_POINT('Ctrl Pts',(0.74004164704549,0.0862412774309402,
-3.19694147846588));
#58862=CARTESIAN_POINT('Ctrl Pts',(0.608994314626862,0.429214540814824,
-3.1810921081709));
#58863=CARTESIAN_POINT('Ctrl Pts',(0.330054662796853,0.667954427233457,
-3.16524273787592));
#58864=CARTESIAN_POINT('Ctrl Pts',(-0.029037707114729,0.744483719674407,
-3.14939336758094));
#58865=CARTESIAN_POINT('Ctrl Pts',(-0.381078362827277,0.640217524502105,
-3.13354399728596));
#58866=CARTESIAN_POINT('Ctrl Pts',(-0.640575358275033,0.380476553371603,
-3.11769462699098));
#58867=CARTESIAN_POINT('Ctrl Pts',(-0.744510678978556,0.0283380694757298,
-3.101845256696));
#58868=CARTESIAN_POINT('Ctrl Pts',(-0.667643965088134,-0.330682223858671,
-3.08599588640102));
#58869=CARTESIAN_POINT('Ctrl Pts',(-0.428642051957971,-0.609397397916976,
-3.07014651610604));
#58870=CARTESIAN_POINT('Ctrl Pts',(-0.0855457889484339,-0.740122365077501,
-3.05429714581106));
#58871=CARTESIAN_POINT('Ctrl Pts',(0.278324995004228,-0.691110985624318,
-3.03844777551607));
#58872=CARTESIAN_POINT('Ctrl Pts',(0.574605445069199,-0.474265516131577,
-3.0225984052211));
#58873=CARTESIAN_POINT('Ctrl Pts',(0.731344802587579,-0.142246184563437,
-3.00674903492611));
#58874=CARTESIAN_POINT('Ctrl Pts',(0.71047941643868,0.224317177477952,-2.99089966463114));
#58875=CARTESIAN_POINT('Ctrl Pts',(0.517076378841355,0.536405831194099,
-2.97505029433616));
#58876=CARTESIAN_POINT('Ctrl Pts',(0.198102998232633,0.71823004628459,-2.95920092404118));
#58877=CARTESIAN_POINT('Ctrl Pts',(-0.16897906120493,0.725634394284768,
-2.9433515537462));
#58878=CARTESIAN_POINT('Ctrl Pts',(-0.495025096670959,0.55682075299025,
-2.92750218345121));
#58879=CARTESIAN_POINT('Ctrl Pts',(-0.700855872396232,0.252784974676972,
-2.91165281315624));
#58880=CARTESIAN_POINT('Ctrl Pts',(-0.736486043530848,-0.112638825362308,
-2.89580344286125));
#58881=CARTESIAN_POINT('Ctrl Pts',(-0.593262937096482,-0.450708647312625,
-2.87995407256628));
#58882=CARTESIAN_POINT('Ctrl Pts',(-0.305967825914806,-0.67932531735516,
-2.8641047022713));
#58883=CARTESIAN_POINT('Ctrl Pts',(0.0556305921335755,-0.742970009161601,
-2.84825533197631));
#58884=CARTESIAN_POINT('Ctrl Pts',(0.403719299001972,-0.626186813106183,
-2.83240596168134));
#58885=CARTESIAN_POINT('Ctrl Pts',(0.65376606674796,-0.357336154431123,
-2.81655659138635));
#58886=CARTESIAN_POINT('Ctrl Pts',(0.745047838431459,-0.0017075547817826,
-2.80070722109137));
#58887=CARTESIAN_POINT('Ctrl Pts',(0.655397128067767,0.354335719079015,
-2.78485785079639));
#58888=CARTESIAN_POINT('Ctrl Pts',(0.406585323622455,0.624329698083909,
-2.76900848050141));
#58889=CARTESIAN_POINT('Ctrl Pts',(0.0590355751521699,0.742707208906157,
-2.75315911020644));
#58890=CARTESIAN_POINT('Ctrl Pts',(-0.302850773721993,0.680720652067139,
-2.73730973991145));
#58891=CARTESIAN_POINT('Ctrl Pts',(-0.591190781874206,0.453423264424848,
-2.72146036961647));
#58892=CARTESIAN_POINT('Ctrl Pts',(-0.735962001540153,0.116013488800808,
-2.70561099932149));
#58893=CARTESIAN_POINT('Ctrl Pts',(-0.702007205556663,-0.249569791123137,
-2.68976162902651));
#58894=CARTESIAN_POINT('Ctrl Pts',(-0.497572207410877,-0.554545846352661,
-2.67391225873153));
#58895=CARTESIAN_POINT('Ctrl Pts',(-0.17230339183656,-0.724852218356499,
-2.65806288843655));
#58896=CARTESIAN_POINT('Ctrl Pts',(0.194808750759242,-0.719130549985429,
-2.64221351814157));
#58897=CARTESIAN_POINT('Ctrl Pts',(0.514612211977501,-0.538770330083558,
-2.62636414784659));
#58898=CARTESIAN_POINT('Ctrl Pts',(0.709443745217406,-0.227571460571446,
-2.61051477755161));
#58899=CARTESIAN_POINT('Ctrl Pts',(0.731989136448934,0.138892409495504,
-2.59466540725663));
#58900=CARTESIAN_POINT('Ctrl Pts',(0.576773309597993,0.471626702626239,
-2.57881603696165));
#58901=CARTESIAN_POINT('Ctrl Pts',(0.28148993124078,0.689827961092316,-2.56296666666667));
#58902=CARTESIAN_POINT('Ctrl Pts',(-0.0821523756355886,0.740506707918403,
-2.54711729637169));
#58903=CARTESIAN_POINT('Ctrl Pts',(-0.425844241126725,0.611355771702471,
-2.5312679260767));
#58904=CARTESIAN_POINT('Ctrl Pts',(-0.666121196140744,0.333739043785331,
-2.51541855578173));
#58905=CARTESIAN_POINT('Ctrl Pts',(-0.744632751478249,-0.0249251423396785,
-2.49956918548675));
#58906=CARTESIAN_POINT('Ctrl Pts',(-0.642312627306116,-0.377536337453543,
-2.48371981519176));
#58907=CARTESIAN_POINT('Ctrl Pts',(-0.38400893816799,-0.638464041823668,
-2.46787044489678));
#58908=CARTESIAN_POINT('Ctrl Pts',(-0.0324499079267794,-0.744342797889699,
-2.45202107460181));
#58909=CARTESIAN_POINT('Ctrl Pts',(0.326989478555387,-0.669460288746687,
-2.43617170430682));
#58910=CARTESIAN_POINT('Ctrl Pts',(0.607020517134824,-0.432001491979012,
-2.42032233401185));
#58911=CARTESIAN_POINT('Ctrl Pts',(0.739638566704057,-0.0896325160792074,
-2.40447296371686));
#58912=CARTESIAN_POINT('Ctrl Pts',(0.692637758545539,0.274503429362429,
-2.38862359342189));
#58913=CARTESIAN_POINT('Ctrl Pts',(0.477432088432004,0.571977095896485,
-2.3727742231269));
#58914=CARTESIAN_POINT('Ctrl Pts',(0.146283564298739,0.730547956065019,
-2.35692485283192));
#58915=CARTESIAN_POINT('Ctrl Pts',(-0.220389455049494,0.71170758419291,
-2.34107548253694));
#58916=CARTESIAN_POINT('Ctrl Pts',(-0.533541600888341,0.520031304265645,
-2.32522611224196));
#58917=CARTESIAN_POINT('Ctrl Pts',(-0.717124877260507,0.202067087148858,
-2.30937674194698));
#58918=CARTESIAN_POINT('Ctrl Pts',(-0.726556673301297,-0.164968475097737,
-2.293527371652));
#58919=CARTESIAN_POINT('Ctrl Pts',(-0.559546507541209,-0.491941971367719,
-2.27767800135702));
#58920=CARTESIAN_POINT('Ctrl Pts',(-0.256652263997058,-0.699448935005199,
-2.26182863106204));
#58921=CARTESIAN_POINT('Ctrl Pts',(0.108569160102076,-0.737096964292657,
-2.24597926076706));
#58922=CARTESIAN_POINT('Ctrl Pts',(0.447424911290323,-0.595743355860196,
-2.23012989047208));
#58923=CARTESIAN_POINT('Ctrl Pts',(0.677624955349841,-0.309715380925531,
-2.2142805201771));
#58924=CARTESIAN_POINT('Ctrl Pts',(0.743265948641989,0.0515259826111631,
-2.19843114988212));
#58925=CARTESIAN_POINT('Ctrl Pts',(0.628407186117013,0.400254426248131,
-2.18258177958713));
#58926=CARTESIAN_POINT('Ctrl Pts',(0.360941750495969,0.651782364017028,
-2.16673240929216));
#58927=CARTESIAN_POINT('Ctrl Pts',(0.00582276644080296,0.745027041580168,
-2.15088303899718));
#58928=CARTESIAN_POINT('Ctrl Pts',(-0.350710257801012,0.657344287544868,
-2.1350336687022));
#58929=CARTESIAN_POINT('Ctrl Pts',(-0.622074418850181,0.410027577983399,
-2.11918429840722));
#58930=CARTESIAN_POINT('Ctrl Pts',(-0.742369799057592,0.0631369839469131,
-2.10333492811223));
#58931=CARTESIAN_POINT('Ctrl Pts',(-0.68238305050513,-0.299086224487242,
-2.08748555781726));
#58932=CARTESIAN_POINT('Ctrl Pts',(-0.456681763011447,-0.588677300927662,
-2.07163618752227));
#58933=CARTESIAN_POINT('Ctrl Pts',(-0.120076771587415,-0.735309979681948,
-2.0557868172273));
#58934=CARTESIAN_POINT('Ctrl Pts',(0.245688479351311,-0.7033749842074,-2.03993744693231));
#58935=CARTESIAN_POINT('Ctrl Pts',(0.551789069732108,-0.50062762590462,
-2.02408807663734));
#58936=CARTESIAN_POINT('Ctrl Pts',(0.723889451262795,-0.17630445157503,
-2.00823870634235));
#58937=CARTESIAN_POINT('Ctrl Pts',(0.72019559732466,0.190833694322822,-1.99238933604737));
#58938=CARTESIAN_POINT('Ctrl Pts',(0.541604548519495,0.511628488571264,
-1.97653996575239));
#58939=CARTESIAN_POINT('Ctrl Pts',(0.231486569231601,0.708175942517187,
-1.96069059545741));
#58940=CARTESIAN_POINT('Ctrl Pts',(-0.134847182213743,0.732745136281187,
-1.94484122516244));
#58941=CARTESIAN_POINT('Ctrl Pts',(-0.468433727216114,0.579369519824041,
-1.92899185486745));
#58942=CARTESIAN_POINT('Ctrl Pts',(-0.688262641408817,0.285295870519851,
-1.91314248457247));
#58943=CARTESIAN_POINT('Ctrl Pts',(-0.740949176834782,-0.0780609674714476,
-1.89729311427749));
#58944=CARTESIAN_POINT('Ctrl Pts',(-0.613698577059101,-0.42246094945019,
-1.88144374398251));
#58945=CARTESIAN_POINT('Ctrl Pts',(-0.33741324280261,-0.664267642502741,
-1.86559437368753));
#58946=CARTESIAN_POINT('Ctrl Pts',(0.0208118171289387,-0.744759065445003,
-1.84974500339255));
#58947=CARTESIAN_POINT('Ctrl Pts',(0.373982793906604,-0.644388133935232,
-1.83389563309757));
#58948=CARTESIAN_POINT('Ctrl Pts',(0.636333246613063,-0.387529607320008,
-1.81804626280259));
#58949=CARTESIAN_POINT('Ctrl Pts',(0.744152207809883,-0.0365607563707129,
-1.80219689250761));
#58950=CARTESIAN_POINT('Ctrl Pts',(0.671256187988306,0.323286757201912,
-1.78634752221263));
#58951=CARTESIAN_POINT('Ctrl Pts',(0.435347752161404,0.60462511689702,-1.77049815191765));
#58952=CARTESIAN_POINT('Ctrl Pts',(0.0937165086312298,0.739132202860013,
-1.75464878162267));
#58953=CARTESIAN_POINT('Ctrl Pts',(-0.270673488955788,0.694143399933487,
-1.73879941132769));
#58954=CARTESIAN_POINT('Ctrl Pts',(-0.569331296400163,0.480584094861693,
-1.72295004103271));
#58955=CARTESIAN_POINT('Ctrl Pts',(-0.729728821415302,0.150316481100898,
-1.70710067073772));
#58956=CARTESIAN_POINT('Ctrl Pts',(-0.712914038616748,-0.216455008807559,
-1.69125130044275));
#58957=CARTESIAN_POINT('Ctrl Pts',(-0.522970364169069,-0.530661092879054,
-1.67540193014776));
#58958=CARTESIAN_POINT('Ctrl Pts',(-0.206025011244697,-0.715997829631028,
-1.65955255985279));
#58959=CARTESIAN_POINT('Ctrl Pts',(0.160952856003563,-0.727456785959838,
-1.6437031895578));
#58960=CARTESIAN_POINT('Ctrl Pts',(0.488843837514907,-0.562255191010648,
-1.62785381926283));
#58961=CARTESIAN_POINT('Ctrl Pts',(0.69802065828021,-0.260511723169583,
-1.61200444896784));
#58962=CARTESIAN_POINT('Ctrl Pts',(0.737685397125054,0.104496182529187,
-1.59615507867287));
#58963=CARTESIAN_POINT('Ctrl Pts',(0.59820559922069,0.444127524879664,-1.58030570837788));
#58964=CARTESIAN_POINT('Ctrl Pts',(0.313453486897711,0.675903919833572,
-1.5644563380829));
#58965=CARTESIAN_POINT('Ctrl Pts',(-0.0474198010938648,0.743539211984775,
-1.54860696778792));
#58966=CARTESIAN_POINT('Ctrl Pts',(-0.396777342219896,0.630608387191001,
-1.53275759749294));
#58967=CARTESIAN_POINT('Ctrl Pts',(-0.649778776201089,0.364536334668214,
-1.51690822719796));
#58968=CARTESIAN_POINT('Ctrl Pts',(-0.744983514862478,0.00993780045431491,
-1.50105885690298));
#58969=CARTESIAN_POINT('Ctrl Pts',(-0.65927139224945,-0.347074096780775,
-1.485209486608));
#58970=CARTESIAN_POINT('Ctrl Pts',(-0.413457322903013,-0.619800160884617,
-1.46936011631302));
#58971=CARTESIAN_POINT('Ctrl Pts',(-0.0672364665092823,-0.742009740411855,
-1.45351074601804));
#58972=CARTESIAN_POINT('Ctrl Pts',(0.295312550496548,-0.684024630268491,
-1.43766137572306));
#58973=CARTESIAN_POINT('Ctrl Pts',(0.586145860154621,-0.459926328794428,
-1.42181200542808));
#58974=CARTESIAN_POINT('Ctrl Pts',(0.734635524413049,-0.124136390978171,
-1.4059626351331));
#58975=CARTESIAN_POINT('Ctrl Pts',(0.704721303745212,0.241799671923618,
-1.39011326483812));
#58976=CARTESIAN_POINT('Ctrl Pts',(0.503667770860069,0.5490154587,-1.37426389454314));
#58977=CARTESIAN_POINT('Ctrl Pts',(0.180300132479707,0.72290459918479,-1.35841452424816));
#58978=CARTESIAN_POINT('Ctrl Pts',(-0.186852815783132,0.721238672374574,
-1.34256515395318));
#58979=CARTESIAN_POINT('Ctrl Pts',(-0.508629156003826,0.544422243261198,
-1.3267157836582));
#58980=CARTESIAN_POINT('Ctrl Pts',(-0.706886534232653,0.235394615518856,
-1.31086641336322));
#58981=CARTESIAN_POINT('Ctrl Pts',(-0.733478780952995,-0.130797840908901,
-1.29501704306824));
#58982=CARTESIAN_POINT('Ctrl Pts',(-0.581948054192647,-0.465226460464269,
-1.27916767277326));
#58983=CARTESIAN_POINT('Ctrl Pts',(-0.289093105769863,-0.686676323671537,
-1.26331830247828));
#58984=CARTESIAN_POINT('Ctrl Pts',(0.0739671777623989,-0.741369040295444,
-1.2474689321833));
#58985=CARTESIAN_POINT('Ctrl Pts',(0.419064769005327,-0.61602265922061,
-1.23161956188832));
#58986=CARTESIAN_POINT('Ctrl Pts',(0.662393822869109,-0.341077147753364,
-1.21577019159333));
#58987=CARTESIAN_POINT('Ctrl Pts',(0.744862657720982,0.0166978569750356,
-1.19992082129835));
#58988=CARTESIAN_POINT('Ctrl Pts',(0.646443981068284,0.370417840600733,
-1.18407145100337));
#58989=CARTESIAN_POINT('Ctrl Pts',(0.39103845341634,0.634183037651179,-1.16822208070839));
#58990=CARTESIAN_POINT('Ctrl Pts',(0.040670489390563,0.743938914553779,
-1.15237271041341));
#58991=CARTESIAN_POINT('Ctrl Pts',(-0.319574172763753,0.6730316080223,-1.13652334011843));
#58992=CARTESIAN_POINT('Ctrl Pts',(-0.6022112702843,0.438680730414834,-1.12067396982345));
#58993=CARTESIAN_POINT('Ctrl Pts',(-0.738603288993907,0.097797642006873,
-1.10482459952847));
#58994=CARTESIAN_POINT('Ctrl Pts',(-0.695627863852887,-0.266835290631117,
-1.08897522923349));
#58995=CARTESIAN_POINT('Ctrl Pts',(-0.483721439256766,-0.566668127300346,
-1.07312585893851));
#58996=CARTESIAN_POINT('Ctrl Pts',(-0.15434481193055,-0.728887423629223,
-1.05727648864353));
#58997=CARTESIAN_POINT('Ctrl Pts',(0.212513958787283,-0.714098742902743,
-1.04142711834855));
#58998=CARTESIAN_POINT('Ctrl Pts',(0.527764395047013,-0.525893468884509,
-1.02557774805357));
#58999=CARTESIAN_POINT('Ctrl Pts',(0.714848937781003,-0.209976649768712,
-1.00972837775859));
#59000=CARTESIAN_POINT('Ctrl Pts',(0.728334704799049,0.156932326434056,
-0.993879007463609));
#59001=CARTESIAN_POINT('Ctrl Pts',(0.564946720759936,0.485730789632812,
-0.978029637168628));
#59002=CARTESIAN_POINT('Ctrl Pts',(0.264363234447157,0.696571085796245,
-0.962180266873649));
#59003=CARTESIAN_POINT('Ctrl Pts',(-0.100420016905207,0.738251324075671,
-0.946330896578666));
#59004=CARTESIAN_POINT('Ctrl Pts',(-0.44081658867988,0.600649592057928,
-0.930481526283688));
#59005=CARTESIAN_POINT('Ctrl Pts',(-0.674162263313043,0.317182029786296,
-0.914632155988704));
#59006=CARTESIAN_POINT('Ctrl Pts',(-0.743789790853027,-0.0433121728562648,
-0.898782785693728));
#59007=CARTESIAN_POINT('Ctrl Pts',(-0.632790349172193,-0.393288152998858,
-0.882933415398745));
#59008=CARTESIAN_POINT('Ctrl Pts',(-0.368119797281484,-0.64775536442716,
-0.867084045103766));
#59009=CARTESIAN_POINT('Ctrl Pts',(-0.0140525312776586,-0.744917259606335,
-0.851234674808785));
#59010=CARTESIAN_POINT('Ctrl Pts',(0.343427346953139,-0.661178383387911,
-0.835385304513805));
#59011=CARTESIAN_POINT('Ctrl Pts',(0.617506993572057,-0.416874453743954,
-0.819535934218824));
#59012=CARTESIAN_POINT('Ctrl Pts',(0.741627043953897,-0.0713338977690619,
-0.803686563923845));
#59013=CARTESIAN_POINT('Ctrl Pts',(0.685645341274624,0.291529866880099,
-0.787837193628863));
#59014=CARTESIAN_POINT('Ctrl Pts',(0.463156862786047,0.583596536786253,
-0.771987823333884));
#59015=CARTESIAN_POINT('Ctrl Pts',(0.128192223119029,0.733938656310268,
-0.756138453038902));
#59016=CARTESIAN_POINT('Ctrl Pts',(-0.237903487482845,0.706046123095525,
-0.740289082743923));
#59017=CARTESIAN_POINT('Ctrl Pts',(-0.546225097875833,0.506692549526098,
-0.724439712448941));
#59018=CARTESIAN_POINT('Ctrl Pts',(-0.721897692169123,0.184290312647237,
-0.708590342153963));
#59019=CARTESIAN_POINT('Ctrl Pts',(-0.722259743312219,-0.182866236591916,
-0.692740971858981));
#59020=CARTESIAN_POINT('Ctrl Pts',(-0.547223328344242,-0.505614305781167,
-0.676891601564001));
#59021=CARTESIAN_POINT('Ctrl Pts',(-0.239295480203475,-0.705575559702084,
-0.66104223126902));
#59022=CARTESIAN_POINT('Ctrl Pts',(0.126744509121461,-0.734190048081749,
-0.64519286097404));
#59023=CARTESIAN_POINT('Ctrl Pts',(0.462005000220514,-0.584508834035863,
-0.62934349067906));
#59024=CARTESIAN_POINT('Ctrl Pts',(0.685069056277096,-0.292881521141793,
-0.613494120384079));
#59025=CARTESIAN_POINT('Ctrl Pts',(0.74176628549086,0.0698711314049664,
-0.597644750089099));
#59026=CARTESIAN_POINT('Ctrl Pts',(0.618327947282097,0.415655803405456,
-0.58179537979412));
#59027=CARTESIAN_POINT('Ctrl Pts',(0.344730646856306,0.660499794407802,
-0.565946009499137));
#59028=CARTESIAN_POINT('Ctrl Pts',(-0.0125833873898627,0.744943525145706,
-0.550096639204159));
#59029=CARTESIAN_POINT('Ctrl Pts',(-0.366841586298341,0.64848010598389,
-0.534247268909176));
#59030=CARTESIAN_POINT('Ctrl Pts',(-0.632013480538201,0.394535369406354,
-0.518397898614198));
#59031=CARTESIAN_POINT('Ctrl Pts',(-0.743702924628839,0.044778981603412,
-0.502548528319216));
#59032=CARTESIAN_POINT('Ctrl Pts',(-0.674786494682493,-0.315851838507415,
-0.486699158024237));
#59033=CARTESIAN_POINT('Ctrl Pts',(-0.442000325054718,-0.599779050940051,
-0.470849787729256));
#59034=CARTESIAN_POINT('Ctrl Pts',(-0.101875791694698,-0.738051841242525,
-0.455000417434276));
#59035=CARTESIAN_POINT('Ctrl Pts',(0.262988951485128,-0.697091105014031,
-0.439151047139295));
#59036=CARTESIAN_POINT('Ctrl Pts',(0.563987669851054,-0.4868440259017,-0.423301676844314));
#59037=CARTESIAN_POINT('Ctrl Pts',(0.72802378836902,-0.158368433886228,
-0.407452306549335));
#59038=CARTESIAN_POINT('Ctrl Pts',(0.715261660922253,0.208566425221401,
-0.391602936254353));
#59039=CARTESIAN_POINT('Ctrl Pts',(0.528800529201736,0.524851595774613,
-0.375753565959374));
#59040=CARTESIAN_POINT('Ctrl Pts',(0.213921882219699,0.713678236746709,
-0.359904195664393));
#59041=CARTESIAN_POINT('Ctrl Pts',(-0.152907009165183,0.729190403064095,
-0.344054825369413));
#59042=CARTESIAN_POINT('Ctrl Pts',(-0.482602922472436,0.567621014616206,
-0.328205455074432));
#59043=CARTESIAN_POINT('Ctrl Pts',(-0.695100262217286,0.268206680437639,
-0.312356084779452));
#59044=CARTESIAN_POINT('Ctrl Pts',(-0.738794727018378,-0.096340787809866,
-0.296506714484472));
#59045=CARTESIAN_POINT('Ctrl Pts',(-0.603075261493803,-0.437492203270981,
-0.280657344189491));
#59046=CARTESIAN_POINT('Ctrl Pts',(-0.320900892537525,-0.672400039771382,
-0.264807973894511));
#59047=CARTESIAN_POINT('Ctrl Pts',(0.0392032167528849,-0.744017675942373,
-0.24895860359953));
#59048=CARTESIAN_POINT('Ctrl Pts',(0.389786977696613,-0.634953008741876,
-0.23310923330455));
#59049=CARTESIAN_POINT('Ctrl Pts',(0.645712165630145,-0.371692022642734,
-0.21725986300957));
#59050=CARTESIAN_POINT('Ctrl Pts',(0.744828326399828,-0.0181668458436364,
-0.20141049271459));
#59051=CARTESIAN_POINT('Ctrl Pts',(0.663065107658535,0.339770143995986,
-0.185561122419609));
#59052=CARTESIAN_POINT('Ctrl Pts',(0.420279052557129,0.615194939045757,
-0.169711752124629));
#59053=CARTESIAN_POINT('Ctrl Pts',(0.0754287878286457,0.741221815035238,
-0.153862381829648));
#59054=CARTESIAN_POINT('Ctrl Pts',(-0.287737574375596,0.687244950605065,
-0.138013011534668));
#59055=CARTESIAN_POINT('Ctrl Pts',(-0.581030808350321,0.466373625781902,
-0.122163641239687));
#59056=CARTESIAN_POINT('Ctrl Pts',(-0.733216654906317,0.132243440338671,
-0.106314270944707));
#59057=CARTESIAN_POINT('Ctrl Pts',(-0.70735477396553,-0.233998665021394,
-0.0904649006497263));
#59058=CARTESIAN_POINT('Ctrl Pts',(-0.509691323571145,-0.543420787681075,
-0.0746155303547458));
#59059=CARTESIAN_POINT('Ctrl Pts',(-0.188295790055588,-0.720863304751339,
-0.0587661600597657));
#59060=CARTESIAN_POINT('Ctrl Pts',(0.17891792069232,-0.723270960896346,
-0.0429167897647859));
#59061=CARTESIAN_POINT('Ctrl Pts',(0.394616248151404,-0.607734388455063,
-0.0323505429014652));
#59062=CARTESIAN_POINT('Ctrl Pts',(0.482201081976442,-0.527701441143752,
-0.027067419469805));
#59063=CARTESIAN_POINT('Ctrl Pts',(0.392888236737271,-0.550964357679767,
-3.8089));
#59064=CARTESIAN_POINT('Ctrl Pts',(0.484334114933679,-0.485755039979474,
-3.80361687656834));
#59065=CARTESIAN_POINT('Ctrl Pts',(0.634040615230541,-0.308993274199896,
-3.79305062970502));
#59066=CARTESIAN_POINT('Ctrl Pts',(0.704605176817581,0.0314014527883039,
-3.77720125941004));
#59067=CARTESIAN_POINT('Ctrl Pts',(0.604063223483086,0.364081211703574,
-3.76135188911506));
#59068=CARTESIAN_POINT('Ctrl Pts',(0.356824591291676,0.608388806027088,
-3.74550251882008));
#59069=CARTESIAN_POINT('Ctrl Pts',(0.0229331537905069,0.704928930307171,
-3.7296531485251));
#59070=CARTESIAN_POINT('Ctrl Pts',(-0.316527984197726,0.630290638914377,
-3.71380377823012));
#59071=CARTESIAN_POINT('Ctrl Pts',(-0.57912108147644,0.402582506643355,
-3.69795440793514));
#59072=CARTESIAN_POINT('Ctrl Pts',(-0.701076597404263,0.077111451249784,
-3.68210503764016));
#59073=CARTESIAN_POINT('Ctrl Pts',(-0.652777845604957,-0.267087379168557,
-3.66625566734518));
#59074=CARTESIAN_POINT('Ctrl Pts',(-0.445954115113484,-0.546424125806921,
-3.6504062970502));
#59075=CARTESIAN_POINT('Ctrl Pts',(-0.130831839792564,-0.693063915639031,
-3.63455692675522));
#59076=CARTESIAN_POINT('Ctrl Pts',(0.21606252083174,-0.671395152184437,
-3.61870755646024));
#59077=CARTESIAN_POINT('Ctrl Pts',(0.510486794197391,-0.48668032805703,
-3.60285818616526));
#59078=CARTESIAN_POINT('Ctrl Pts',(0.680940981975007,-0.183776692274722,
-3.58700881587028));
#59079=CARTESIAN_POINT('Ctrl Pts',(0.686030833613329,0.163756498125624,
-3.5711594455753));
#59080=CARTESIAN_POINT('Ctrl Pts',(0.524520293312469,0.471521960898263,
-3.55531007528032));
#59081=CARTESIAN_POINT('Ctrl Pts',(0.235631679485712,0.664779818244593,
-3.53946070498533));
#59082=CARTESIAN_POINT('Ctrl Pts',(-0.110479333395072,0.696598028792635,
-3.52361133469035));
#59083=CARTESIAN_POINT('Ctrl Pts',(-0.429760793823647,0.55924963662321,
-3.50776196439537));
#59084=CARTESIAN_POINT('Ctrl Pts',(-0.644676221530144,0.286089261747328,
-3.49191259410039));
#59085=CARTESIAN_POINT('Ctrl Pts',(-0.703034092962096,-0.0565469748075895,
-3.47606322380541));
#59086=CARTESIAN_POINT('Ctrl Pts',(-0.590662385922995,-0.385450959342922,
-3.46021385351043));
#59087=CARTESIAN_POINT('Ctrl Pts',(-0.334850209657572,-0.620749412673154,
-3.44436448321545));
#59088=CARTESIAN_POINT('Ctrl Pts',(0.00227926788749094,-0.70530085860637,
-3.42851511292047));
#59089=CARTESIAN_POINT('Ctrl Pts',(0.338855232525197,-0.618572249312001,
-3.41266574262549));
#59090=CARTESIAN_POINT('Ctrl Pts',(0.593141288900064,-0.381625349818476,
-3.39681637233051));
#59091=CARTESIAN_POINT('Ctrl Pts',(0.703384882402956,-0.0520019560290773,
-3.38096700203553));
#59092=CARTESIAN_POINT('Ctrl Pts',(0.642813709332344,0.290249946284879,
-3.36511763174055));
#59093=CARTESIAN_POINT('Ctrl Pts',(0.426137285130135,0.562015578472108,
-3.34926826144557));
#59094=CARTESIAN_POINT('Ctrl Pts',(0.105974785652812,0.697297526906368,
-3.33341889115059));
#59095=CARTESIAN_POINT('Ctrl Pts',(-0.239923351207117,0.663243003558396,
-3.31756952085561));
#59096=CARTESIAN_POINT('Ctrl Pts',(-0.527556870419987,0.468122040387345,
-3.30172015056063));
#59097=CARTESIAN_POINT('Ctrl Pts',(-0.687074892798328,0.159319138554876,
-3.28587078026565));
#59098=CARTESIAN_POINT('Ctrl Pts',(-0.679738977357021,-0.188173905962906,
-3.27002140997067));
#59099=CARTESIAN_POINT('Ctrl Pts',(-0.507330627672634,-0.489969519918335,
-3.25417203967569));
#59100=CARTESIAN_POINT('Ctrl Pts',(-0.211718659443945,-0.672777604760268,
-3.23832266938071));
#59101=CARTESIAN_POINT('Ctrl Pts',(0.135308507343731,-0.692203802405131,
-3.22247329908573));
#59102=CARTESIAN_POINT('Ctrl Pts',(0.449476436357704,-0.543530522954218,
-3.20662392879074));
#59103=CARTESIAN_POINT('Ctrl Pts',(0.65449045194897,-0.262862596295751,
-3.19077455849577));
#59104=CARTESIAN_POINT('Ctrl Pts',(0.700563556851036,0.0816406702320175,
-3.17492518820078));
#59105=CARTESIAN_POINT('Ctrl Pts',(0.576507045056651,0.406317761393417,
-3.1590758179058));
#59106=CARTESIAN_POINT('Ctrl Pts',(0.312447643247322,0.632321885160478,
-3.14322644761082));
#59107=CARTESIAN_POINT('Ctrl Pts',(-0.0274886683206437,0.704768663702968,
-3.12737707731584));
#59108=CARTESIAN_POINT('Ctrl Pts',(-0.360749444800962,0.606064628814044,
-3.11152770702087));
#59109=CARTESIAN_POINT('Ctrl Pts',(-0.606403373669456,0.360179739333031,
-3.09567833672588));
#59110=CARTESIAN_POINT('Ctrl Pts',(-0.704794184842326,0.0268263533889801,
-3.0798289664309));
#59111=CARTESIAN_POINT('Ctrl Pts',(-0.632027984856805,-0.313041726582184,
-3.06397959613592));
#59112=CARTESIAN_POINT('Ctrl Pts',(-0.405775812394436,-0.576888625558993,
-3.04813022584094));
#59113=CARTESIAN_POINT('Ctrl Pts',(-0.0809822831169064,-0.700639968917618,
-3.03228085554596));
#59114=CARTESIAN_POINT('Ctrl Pts',(0.263477534324128,-0.654243139154081,
-3.01643148525098));
#59115=CARTESIAN_POINT('Ctrl Pts',(0.543952676164601,-0.448965457821732,
-3.000582114956));
#59116=CARTESIAN_POINT('Ctrl Pts',(0.692330652242036,-0.134657952568069,
-2.98473274466102));
#59117=CARTESIAN_POINT('Ctrl Pts',(0.672578346146962,0.212350805314992,
-2.96888337436604));
#59118=CARTESIAN_POINT('Ctrl Pts',(0.489492542171056,0.507790850038306,
-2.95303400407106));
#59119=CARTESIAN_POINT('Ctrl Pts',(0.1875350416004,0.679915512689367,-2.93718463377608));
#59120=CARTESIAN_POINT('Ctrl Pts',(-0.159964743367749,0.686924870057126,
-2.9213352634811));
#59121=CARTESIAN_POINT('Ctrl Pts',(-0.468617602588818,0.527116722147587,
-2.90548589318612));
#59122=CARTESIAN_POINT('Ctrl Pts',(-0.663468177454696,0.239299966002197,
-2.88963652289114));
#59123=CARTESIAN_POINT('Ctrl Pts',(-0.697197629737455,-0.106630020689219,
-2.87378715259615));
#59124=CARTESIAN_POINT('Ctrl Pts',(-0.56161486994617,-0.426665248267367,
-2.85793778230118));
#59125=CARTESIAN_POINT('Ctrl Pts',(-0.289645737183324,-0.643086186413016,
-2.84208841200619));
#59126=CARTESIAN_POINT('Ctrl Pts',(0.0526629354583269,-0.703335703240367,
-2.82623904171122));
#59127=CARTESIAN_POINT('Ctrl Pts',(0.382182582841647,-0.592782396496553,
-2.81038967141623));
#59128=CARTESIAN_POINT('Ctrl Pts',(0.618890413665208,-0.33827378275151,
-2.79454030112126));
#59129=CARTESIAN_POINT('Ctrl Pts',(0.705302689111543,-0.0016164639601243,
-2.77869093082627));
#59130=CARTESIAN_POINT('Ctrl Pts',(0.620434464765853,0.335433407928336,
-2.7628415605313));
#59131=CARTESIAN_POINT('Ctrl Pts',(0.384895717176935,0.591024350701866,
-2.74699219023631));
#59132=CARTESIAN_POINT('Ctrl Pts',(0.0558862770419258,0.703086922266445,
-2.73114281994134));
#59133=CARTESIAN_POINT('Ctrl Pts',(-0.286694966534403,0.644407085922823,
-2.71529344964635));
#59134=CARTESIAN_POINT('Ctrl Pts',(-0.559653255436154,0.429235052044242,
-2.69944407935137));
#59135=CARTESIAN_POINT('Ctrl Pts',(-0.696701543169347,0.109824660114017,
-2.68359470905639));
#59136=CARTESIAN_POINT('Ctrl Pts',(-0.664558091863175,-0.236256298885097,
-2.66774533876141));
#59137=CARTESIAN_POINT('Ctrl Pts',(-0.471028835749505,-0.52496317215227,
-2.65189596846643));
#59138=CARTESIAN_POINT('Ctrl Pts',(-0.163111735027927,-0.686184419904654,
-2.63604659817145));
#59139=CARTESIAN_POINT('Ctrl Pts',(0.184416528289274,-0.680767978328477,
-2.62019722787647));
#59140=CARTESIAN_POINT('Ctrl Pts',(0.487159828181642,-0.510029212917986,
-2.60434785758149));
#59141=CARTESIAN_POINT('Ctrl Pts',(0.671597923602639,-0.21543148617677,
-2.58849848728651));
#59142=CARTESIAN_POINT('Ctrl Pts',(0.692940613618548,0.131483087207663,
-2.57264911699153));
#59143=CARTESIAN_POINT('Ctrl Pts',(0.546004894294652,0.446467413850098,
-2.55679974669655));
#59144=CARTESIAN_POINT('Ctrl Pts',(0.266473634605688,0.653028558551418,
-2.54095037640157));
#59145=CARTESIAN_POINT('Ctrl Pts',(-0.0777698940442144,0.701003808694404,
-2.52510100610659));
#59146=CARTESIAN_POINT('Ctrl Pts',(-0.403127252931393,0.578742528390386,
-2.50925163581161));
#59147=CARTESIAN_POINT('Ctrl Pts',(-0.630586449188775,0.315935478101465,
-2.49340226551663));
#59148=CARTESIAN_POINT('Ctrl Pts',(-0.704909745290741,-0.0235954914729733,
-2.47755289522165));
#59149=CARTESIAN_POINT('Ctrl Pts',(-0.608047966749425,-0.357396371491931,
-2.46170352492667));
#59150=CARTESIAN_POINT('Ctrl Pts',(-0.363523686348719,-0.604404687016196,
-2.44585415463169));
#59151=CARTESIAN_POINT('Ctrl Pts',(-0.0307188426589624,-0.704635259499128,
-2.43000478433671));
#59152=CARTESIAN_POINT('Ctrl Pts',(0.309545973614037,-0.633747415334411,
-2.41415541404173));
#59153=CARTESIAN_POINT('Ctrl Pts',(0.574638541308189,-0.408956040506685,
-2.39830604374675));
#59154=CARTESIAN_POINT('Ctrl Pts',(0.700181979140083,-0.0848510006492837,
-2.38245667345177));
#59155=CARTESIAN_POINT('Ctrl Pts',(0.655688465200883,0.259859833037388,
-2.36660730315679));
#59156=CARTESIAN_POINT('Ctrl Pts',(0.451963106890093,0.54146453829772,-2.35075793286181));
#59157=CARTESIAN_POINT('Ctrl Pts',(0.138479955179697,0.691576314109395,
-2.33490856256682));
#59158=CARTESIAN_POINT('Ctrl Pts',(-0.20863261025693,0.673740996348811,
-2.31905919227184));
#59159=CARTESIAN_POINT('Ctrl Pts',(-0.505079414298638,0.492289834828481,
-2.30320982197686));
#59160=CARTESIAN_POINT('Ctrl Pts',(-0.678869299755915,0.191287663148,-2.28736045168189));
#59161=CARTESIAN_POINT('Ctrl Pts',(-0.687797949390983,-0.156168105057554,
-2.2715110813869));
#59162=CARTESIAN_POINT('Ctrl Pts',(-0.529697069227978,-0.465698948973474,
-2.25566171109192));
#59163=CARTESIAN_POINT('Ctrl Pts',(-0.24296095180248,-0.662136294219658,
-2.23981234079694));
#59164=CARTESIAN_POINT('Ctrl Pts',(0.102777454848793,-0.69777596046189,
-2.22396297050196));
#59165=CARTESIAN_POINT('Ctrl Pts',(0.423556685665886,-0.563962968865366,
-2.20811360020698));
#59166=CARTESIAN_POINT('Ctrl Pts',(0.641476531525165,-0.293193375992965,
-2.192264229912));
#59167=CARTESIAN_POINT('Ctrl Pts',(0.70361585560182,0.048777289484231,-2.17641485961702));
#59168=CARTESIAN_POINT('Ctrl Pts',(0.59488432200333,0.378902546386728,-2.16056548932204));
#59169=CARTESIAN_POINT('Ctrl Pts',(0.341687035524299,0.617012533080427,
-2.14471611902706));
#59170=CARTESIAN_POINT('Ctrl Pts',(0.00551214649170594,0.70528300168426,
-2.12886674873208));
#59171=CARTESIAN_POINT('Ctrl Pts',(-0.332001349667448,0.622277751524753,
-2.1130173784371));
#59172=CARTESIAN_POINT('Ctrl Pts',(-0.588889381071465,0.388154341834502,
-2.09716800814212));
#59173=CARTESIAN_POINT('Ctrl Pts',(-0.702767511805465,0.0597688930336289,
-2.08131863784714));
#59174=CARTESIAN_POINT('Ctrl Pts',(-0.645980802439012,-0.283131240070673,
-2.06546926755216));
#59175=CARTESIAN_POINT('Ctrl Pts',(-0.432319723520416,-0.557273858061672,
-2.04961989725718));
#59176=CARTESIAN_POINT('Ctrl Pts',(-0.113671183958779,-0.69608430391808,
-2.0337705269622));
#59177=CARTESIAN_POINT('Ctrl Pts',(0.232582038671535,-0.665852905311,-2.01792115666722));
#59178=CARTESIAN_POINT('Ctrl Pts',(0.522353457898419,-0.473921260596391,
-2.00207178637224));
#59179=CARTESIAN_POINT('Ctrl Pts',(0.685273012361204,-0.166899355160858,
-1.98622241607726));
#59180=CARTESIAN_POINT('Ctrl Pts',(0.681776209899179,0.180653524292269,
-1.97037304578227));
#59181=CARTESIAN_POINT('Ctrl Pts',(0.512712237794087,0.484335273792739,
-1.9545236754873));
#59182=CARTESIAN_POINT('Ctrl Pts',(0.219137740357689,0.670397752811446,
-1.93867430519231));
#59183=CARTESIAN_POINT('Ctrl Pts',(-0.12765365568297,0.693656284058958,
-1.92282493489733));
#59184=CARTESIAN_POINT('Ctrl Pts',(-0.443444770166212,0.548462607691666,
-1.90697556460235));
#59185=CARTESIAN_POINT('Ctrl Pts',(-0.651546742048982,0.270076543130026,
-1.89112619430737));
#59186=CARTESIAN_POINT('Ctrl Pts',(-0.701422673766515,-0.0738967451917915,
-1.87527682401239));
#59187=CARTESIAN_POINT('Ctrl Pts',(-0.580960354995419,-0.399924445548537,
-1.85942745371742));
#59188=CARTESIAN_POINT('Ctrl Pts',(-0.319413674149484,-0.628831774793575,
-1.84357808342243));
#59189=CARTESIAN_POINT('Ctrl Pts',(0.0197015947556392,-0.705029320941897,
-1.82772871312745));
#59190=CARTESIAN_POINT('Ctrl Pts',(0.354032394455494,-0.610012753882915,
-1.81187934283247));
#59191=CARTESIAN_POINT('Ctrl Pts',(0.602387560713073,-0.366856542700088,
-1.79602997253749));
#59192=CARTESIAN_POINT('Ctrl Pts',(0.704454836593539,-0.0346103947345185,
-1.78018060224251));
#59193=CARTESIAN_POINT('Ctrl Pts',(0.635447510951297,0.306040776775757,
-1.76433123194753));
#59194=CARTESIAN_POINT('Ctrl Pts',(0.412123791868901,0.572370925536324,
-1.74848186165255));
#59195=CARTESIAN_POINT('Ctrl Pts',(0.0887171294811145,0.699702627664309,
-1.73263249135757));
#59196=CARTESIAN_POINT('Ctrl Pts',(-0.256234203744069,0.657113786992292,
-1.71678312106259));
#59197=CARTESIAN_POINT('Ctrl Pts',(-0.53895988100815,0.454946967115278,
-1.70093375076761));
#59198=CARTESIAN_POINT('Ctrl Pts',(-0.690800876826863,0.142297732936779,
-1.68508438047263));
#59199=CARTESIAN_POINT('Ctrl Pts',(-0.674883091534556,-0.204908050072388,
-1.66923501017765));
#59200=CARTESIAN_POINT('Ctrl Pts',(-0.495072108323442,-0.502352569202039,
-1.65338563988267));
#59201=CARTESIAN_POINT('Ctrl Pts',(-0.195034448742293,-0.677802375348079,
-1.63753626958769));
#59202=CARTESIAN_POINT('Ctrl Pts',(0.152366702248935,-0.688650044848245,
-1.62168689929271));
#59203=CARTESIAN_POINT('Ctrl Pts',(0.462766087451164,-0.532261255896812,
-1.60583752899773));
#59204=CARTESIAN_POINT('Ctrl Pts',(0.660784210013829,-0.246614525160438,
-1.58998815870274));
#59205=CARTESIAN_POINT('Ctrl Pts',(0.698333002892782,0.0989217533935704,
-1.57413878840777));
#59206=CARTESIAN_POINT('Ctrl Pts',(0.566293861962189,0.420435200866502,
-1.55828941811278));
#59207=CARTESIAN_POINT('Ctrl Pts',(0.296732069830279,0.639847305970687,
-1.54244004781781));
#59208=CARTESIAN_POINT('Ctrl Pts',(-0.0448901553745235,0.703874541501651,
-1.52659067752282));
#59209=CARTESIAN_POINT('Ctrl Pts',(-0.37561095007723,0.596968098314967,
-1.51074130722784));
#59210=CARTESIAN_POINT('Ctrl Pts',(-0.615115828195774,0.345089863842356,
-1.49489193693286));
#59211=CARTESIAN_POINT('Ctrl Pts',(-0.705241796932766,0.00940766085441594,
-1.47904256663788));
#59212=CARTESIAN_POINT('Ctrl Pts',(-0.624102053348382,-0.328559162450296,
-1.4631931963429));
#59213=CARTESIAN_POINT('Ctrl Pts',(-0.391401124376496,-0.58673644514426,
-1.44734382604792));
#59214=CARTESIAN_POINT('Ctrl Pts',(-0.0636496855493053,-0.702426660764798,
-1.43149445575294));
#59215=CARTESIAN_POINT('Ctrl Pts',(0.279558875618117,-0.647534810868762,
-1.41564508545796));
#59216=CARTESIAN_POINT('Ctrl Pts',(0.554877458941432,-0.435391205449084,
-1.39979571516298));
#59217=CARTESIAN_POINT('Ctrl Pts',(0.695445827983648,-0.117514239834355,
-1.383946344868));
#59218=CARTESIAN_POINT('Ctrl Pts',(0.667127404398765,0.228900682663626,
-1.36809697457302));
#59219=CARTESIAN_POINT('Ctrl Pts',(0.476799226683618,0.51972780727763,-1.35224760427804));
#59220=CARTESIAN_POINT('Ctrl Pts',(0.170681883398015,0.684340697973908,
-1.33639823398306));
#59221=CARTESIAN_POINT('Ctrl Pts',(-0.176885008776566,0.682763641309219,
-1.32054886368808));
#59222=CARTESIAN_POINT('Ctrl Pts',(-0.481495942925332,0.515379620445116,
-1.3046994933931));
#59223=CARTESIAN_POINT('Ctrl Pts',(-0.669177129002431,0.222837308913415,
-1.28885012309812));
#59224=CARTESIAN_POINT('Ctrl Pts',(-0.69435079189213,-0.123820329600919,
-1.27300075280314));
#59225=CARTESIAN_POINT('Ctrl Pts',(-0.550903588163435,-0.440408597523208,
-1.25715138250816));
#59226=CARTESIAN_POINT('Ctrl Pts',(-0.273671211948421,-0.650045047650077,
-1.24130201221318));
#59227=CARTESIAN_POINT('Ctrl Pts',(0.0700213418398019,-0.70182013928831,
-1.2254526419182));
#59228=CARTESIAN_POINT('Ctrl Pts',(0.396709436958603,-0.583160457208559,
-1.20960327162322));
#59229=CARTESIAN_POINT('Ctrl Pts',(0.627057915507849,-0.322882125275867,
-1.19375390132824));
#59230=CARTESIAN_POINT('Ctrl Pts',(0.705127387008331,0.0158070969666729,
-1.17790453103325));
#59231=CARTESIAN_POINT('Ctrl Pts',(0.611958930271261,0.35065761632248,-1.16205516073828));
#59232=CARTESIAN_POINT('Ctrl Pts',(0.37017820670576,0.600352056300146,-1.14620579044329));
#59233=CARTESIAN_POINT('Ctrl Pts',(0.0385008908891459,0.704252921630042,
-1.13035642014832));
#59234=CARTESIAN_POINT('Ctrl Pts',(-0.302526243006624,0.637128219839621,
-1.11450704985333));
#59235=CARTESIAN_POINT('Ctrl Pts',(-0.570085847425583,0.41527896983686,
-1.09865767955835));
#59236=CARTESIAN_POINT('Ctrl Pts',(-0.699201929114728,0.0925805516615262,
-1.08280830926337));
#59237=CARTESIAN_POINT('Ctrl Pts',(-0.658519061043479,-0.2526007570577,
-1.06695893896839));
#59238=CARTESIAN_POINT('Ctrl Pts',(-0.45791694746335,-0.536438780709928,
-1.05110956867341));
#59239=CARTESIAN_POINT('Ctrl Pts',(-0.146111169363581,-0.69000436405208,
-1.03526019837843));
#59240=CARTESIAN_POINT('Ctrl Pts',(0.201177238393133,-0.676004596860274,
-1.01941082808345));
#59241=CARTESIAN_POINT('Ctrl Pts',(0.49961039794122,-0.497839277772177,
-1.00356145778847));
#59242=CARTESIAN_POINT('Ctrl Pts',(0.676714772016422,-0.198775284073422,
-0.987712087493491));
#59243=CARTESIAN_POINT('Ctrl Pts',(0.689481130432523,0.148560650918064,
-0.971862717198511));
#59244=CARTESIAN_POINT('Ctrl Pts',(0.53480920392387,0.459819107499921,-0.956013346903531));
#59245=CARTESIAN_POINT('Ctrl Pts',(0.250260574610009,0.659411966087648,
-0.94016397660855));
#59246=CARTESIAN_POINT('Ctrl Pts',(-0.0950630339562937,0.698868740035448,
-0.92431460631357));
#59247=CARTESIAN_POINT('Ctrl Pts',(-0.417300889101903,0.568607478123943,
-0.908465236018589));
#59248=CARTESIAN_POINT('Ctrl Pts',(-0.638198559455265,0.30026171073404,
-0.892615865723609));
#59249=CARTESIAN_POINT('Ctrl Pts',(-0.70411175304767,-0.0410016517209196,
-0.876766495428628));
#59250=CARTESIAN_POINT('Ctrl Pts',(-0.599033661857993,-0.372307894335739,
-0.860917125133648));
#59251=CARTESIAN_POINT('Ctrl Pts',(-0.348482163889545,-0.613200356877398,
-0.845067754838668));
#59252=CARTESIAN_POINT('Ctrl Pts',(-0.0133028882008698,-0.705179076114163,
-0.829218384543688));
#59253=CARTESIAN_POINT('Ctrl Pts',(0.325106951293811,-0.625907314579525,
-0.813369014248707));
#59254=CARTESIAN_POINT('Ctrl Pts',(0.584565608603702,-0.394635965747537,
-0.797519643953726));
#59255=CARTESIAN_POINT('Ctrl Pts',(0.702064379543393,-0.067528536190703,
-0.781670273658747));
#59256=CARTESIAN_POINT('Ctrl Pts',(0.64906906380117,0.275977982165213,-0.765820903363766));
#59257=CARTESIAN_POINT('Ctrl Pts',(0.438449404123081,0.552464131186653,
-0.749971533068786));
#59258=CARTESIAN_POINT('Ctrl Pts',(0.121353710493789,0.694786134845175,
-0.734122162773805));
#59259=CARTESIAN_POINT('Ctrl Pts',(-0.225212343175068,0.66838155024305,
-0.718272792478825));
#59260=CARTESIAN_POINT('Ctrl Pts',(-0.517086300395306,0.479662646207939,
-0.702423422183845));
#59261=CARTESIAN_POINT('Ctrl Pts',(-0.683387505186542,0.174459204339074,
-0.686574051888864));
#59262=CARTESIAN_POINT('Ctrl Pts',(-0.683730242433263,-0.173111096714972,
-0.670724681593884));
#59263=CARTESIAN_POINT('Ctrl Pts',(-0.518031279492488,-0.478641922203943,
-0.654875311298903));
#59264=CARTESIAN_POINT('Ctrl Pts',(-0.226530078974616,-0.667936089415343,
-0.639025941003923));
#59265=CARTESIAN_POINT('Ctrl Pts',(0.119983225911628,-0.695024115929475,
-0.623176570708943));
#59266=CARTESIAN_POINT('Ctrl Pts',(0.437358988551026,-0.553327761238609,
-0.607327200413961));
#59267=CARTESIAN_POINT('Ctrl Pts',(0.648523521169567,-0.277257531391908,
-0.591477830118983));
#59268=CARTESIAN_POINT('Ctrl Pts',(0.702196193133595,0.0661438022220719,
-0.575628459824));
#59269=CARTESIAN_POINT('Ctrl Pts',(0.585342767907381,0.393482325247575,
-0.559779089529022));
#59270=CARTESIAN_POINT('Ctrl Pts',(0.326340725662382,0.625264925449887,
-0.54392971923404));
#59271=CARTESIAN_POINT('Ctrl Pts',(-0.011912116922439,0.705203940498158,
-0.528080348939061));
#59272=CARTESIAN_POINT('Ctrl Pts',(-0.347272140053286,0.613886436539002,
-0.51223097864408));
#59273=CARTESIAN_POINT('Ctrl Pts',(-0.59829823587811,0.373488577025802,
-0.496381608349099));
#59274=CARTESIAN_POINT('Ctrl Pts',(-0.704029520768948,0.0423902124285739,
-0.480532238054118));
#59275=CARTESIAN_POINT('Ctrl Pts',(-0.638789490722744,-0.299002479530853,
-0.464682867759139));
#59276=CARTESIAN_POINT('Ctrl Pts',(-0.41842147815042,-0.567783376690792,
-0.448833497464158));
#59277=CARTESIAN_POINT('Ctrl Pts',(-0.0964411493212378,-0.698679898767291,
-0.432984127169178));
#59278=CARTESIAN_POINT('Ctrl Pts',(0.248959603828383,-0.659904244480755,
-0.417134756874197));
#59279=CARTESIAN_POINT('Ctrl Pts',(0.533901314322515,-0.4608729573248,-0.401285386579217));
#59280=CARTESIAN_POINT('Ctrl Pts',(0.689186800078316,-0.149920148114908,
-0.385436016284236));
#59281=CARTESIAN_POINT('Ctrl Pts',(0.677105478124627,0.197440289037993,
-0.369586645989256));
#59282=CARTESIAN_POINT('Ctrl Pts',(0.50059125872345,0.496852984183748,-0.353737275694276));
#59283=CARTESIAN_POINT('Ctrl Pts',(0.202510055068408,0.675606522928187,
-0.337887905399296));
#59284=CARTESIAN_POINT('Ctrl Pts',(-0.144750067291325,0.690291180816235,
-0.322038535104314));
#59285=CARTESIAN_POINT('Ctrl Pts',(-0.456858098816181,0.537340835519866,
-0.306189164809335));
#59286=CARTESIAN_POINT('Ctrl Pts',(-0.65801960472246,0.253898989021423,
-0.290339794514354));
#59287=CARTESIAN_POINT('Ctrl Pts',(-0.699383154730711,-0.091201414470888,
-0.274490424219375));
#59288=CARTESIAN_POINT('Ctrl Pts',(-0.570903748360253,-0.414153845586582,
-0.258641053924393));
#59289=CARTESIAN_POINT('Ctrl Pts',(-0.303782187894811,-0.636530343082252,
-0.242791683629414));
#59290=CARTESIAN_POINT('Ctrl Pts',(0.0371118910375575,-0.704327481431854,
-0.226942313334432));
#59291=CARTESIAN_POINT('Ctrl Pts',(0.36899349191975,-0.601080952691479,
-0.211092943039453));
#59292=CARTESIAN_POINT('Ctrl Pts',(0.611266154089886,-0.351863826144559,
-0.195243572744473));
#59293=CARTESIAN_POINT('Ctrl Pts',(0.705094887117879,-0.0171977214955263,
-0.179394202449492));
#59294=CARTESIAN_POINT('Ctrl Pts',(0.627693390094468,0.321644844638033,
-0.163544832154511));
#59295=CARTESIAN_POINT('Ctrl Pts',(0.39785894362146,0.58237689240233,-0.147695461859531));
#59296=CARTESIAN_POINT('Ctrl Pts',(0.071404981194182,0.701680767872716,
-0.13184609156455));
#59297=CARTESIAN_POINT('Ctrl Pts',(-0.272387992417769,0.650583340742987,
-0.11599672126957));
#59298=CARTESIAN_POINT('Ctrl Pts',(-0.550035273505243,0.441494566425662,
-0.100147350974589));
#59299=CARTESIAN_POINT('Ctrl Pts',(-0.694102649160791,0.125188812418524,
-0.084297980679609));
#59300=CARTESIAN_POINT('Ctrl Pts',(-0.669620390127032,-0.221515826467681,
-0.0684486103846286));
#59301=CARTESIAN_POINT('Ctrl Pts',(-0.482501448347761,-0.514431588282284,
-0.0525992400896481));
#59302=CARTESIAN_POINT('Ctrl Pts',(-0.178251006477893,-0.682408297960222,
-0.036749869794668));
#59303=CARTESIAN_POINT('Ctrl Pts',(0.169373406760312,-0.684687515838503,
-0.0209004994996882));
#59304=CARTESIAN_POINT('Ctrl Pts',(0.37356514123207,-0.575314330614417,
-0.0103342526363675));
#59305=CARTESIAN_POINT('Ctrl Pts',(0.456477694810158,-0.499550802362287,
-0.00505112920470729));
#59306=CARTESIAN_POINT('Ctrl Pts',(0.533647856309012,-0.584002718706682,
-0.0711000000000004));
#59307=CARTESIAN_POINT('Ctrl Pts',(0.436718461990072,-0.672574504136354,
-0.0763831234316606));
#59308=CARTESIAN_POINT('Ctrl Pts',(0.317362705273201,-0.736506177574195,
-0.0816662468633211));
#59309=CARTESIAN_POINT('Ctrl Pts',(0.189952775953544,-0.768027925513371,
-0.0869493702949814));
#59310=CARTESIAN_POINT('Ctrl Pts',(0.0625428466338946,-0.799549673452546,
-0.0922324937266413));
#59311=CARTESIAN_POINT('Ctrl Pts',(-0.0729212552885391,-0.79866149589306,
-0.0975156171583011));
#59312=CARTESIAN_POINT('Ctrl Pts',(-0.199934259050909,-0.7654883851375,
-0.102798740589961));
#59313=CARTESIAN_POINT('Ctrl Pts',(-0.326947262813287,-0.732315274381938,
-0.108081864021621));
#59314=CARTESIAN_POINT('Ctrl Pts',(-0.4455091684156,-0.666857230430297,
-0.113364987453281));
#59315=CARTESIAN_POINT('Ctrl Pts',(-0.541248865820859,-0.57705573439617,
-0.118648110884941));
#59316=CARTESIAN_POINT('Ctrl Pts',(-0.636988563226119,-0.487254238362043,
-0.123931234316602));
#59317=CARTESIAN_POINT('Ctrl Pts',(-0.709906052434325,-0.373109290245429,
-0.129214357748262));
#59318=CARTESIAN_POINT('Ctrl Pts',(-0.751134984497568,-0.248483976469156,
-0.134497481179922));
#59319=CARTESIAN_POINT('Ctrl Pts',(-0.777588539083348,-0.168521135430888,
-0.137887270512046));
#59320=CARTESIAN_POINT('Ctrl Pts',(-0.79099642429751,-0.0842436963923346,
-0.14127705984417));
#59321=CARTESIAN_POINT('Ctrl Pts',(-0.791054317571617,1.54395522024842E-5,
-0.144666849176294));
#59322=CARTESIAN_POINT('Origin',(0.,0.,-0.599));
#59323=CARTESIAN_POINT('',(0.23094010767585,-0.4,-0.599));
#59324=CARTESIAN_POINT('',(-0.230940107675851,-0.4,-0.599));
#59325=CARTESIAN_POINT('',(0.115470053837925,-0.4,-0.599));
#59326=CARTESIAN_POINT('Origin',(0.,0.,-0.599));
#59327=CARTESIAN_POINT('Origin',(0.,0.,-0.599));
#59328=CARTESIAN_POINT('',(-0.461880215351701,1.11022302462516E-16,-0.599));
#59329=CARTESIAN_POINT('',(-0.288675134594813,-0.3,-0.599));
#59330=CARTESIAN_POINT('Origin',(0.,0.,-0.599));
#59331=CARTESIAN_POINT('Origin',(0.,0.,-0.599));
#59332=CARTESIAN_POINT('',(-0.23094010767585,0.4,-0.599));
#59333=CARTESIAN_POINT('',(-0.404145188432738,0.1,-0.599));
#59334=CARTESIAN_POINT('Origin',(0.,0.,-0.599));
#59335=CARTESIAN_POINT('Origin',(0.,0.,-0.599));
#59336=CARTESIAN_POINT('',(0.23094010767585,0.4,-0.599));
#59337=CARTESIAN_POINT('',(-0.115470053837925,0.4,-0.599));
#59338=CARTESIAN_POINT('Origin',(0.,0.,-0.599));
#59339=CARTESIAN_POINT('Origin',(0.,0.,-0.599));
#59340=CARTESIAN_POINT('',(0.461880215351701,0.,-0.599));
#59341=CARTESIAN_POINT('',(0.288675134594813,0.3,-0.599));
#59342=CARTESIAN_POINT('Origin',(0.,0.,-0.599));
#59343=CARTESIAN_POINT('Origin',(0.,0.,-0.599));
#59344=CARTESIAN_POINT('',(0.404145188432738,-0.1,-0.599));
#59345=CARTESIAN_POINT('Origin',(0.,0.,-0.599));
#59346=CARTESIAN_POINT('Origin',(0.,0.,-0.73806406460551));
#59347=CARTESIAN_POINT('',(0.,0.,-0.87712812921102));
#59348=CARTESIAN_POINT('',(-0.460219541126976,-5.63606387946214E-17,-0.6));
#59349=CARTESIAN_POINT('',(-0.23094010767585,-2.82820063659975E-17,-0.73806406460551));
#59350=CARTESIAN_POINT('',(-0.460210453731243,-0.00289211196316049,-0.6));
#59351=CARTESIAN_POINT('Origin',(0.,0.,-0.6));
#59352=CARTESIAN_POINT('Ctrl Pts',(-0.4618802153517,-6.93889390390722E-16,
-0.599));
#59353=CARTESIAN_POINT('Ctrl Pts',(-0.461043830945924,-0.00144866028546382,
-0.599503641468823));
#59354=CARTESIAN_POINT('Ctrl Pts',(-0.460210453731243,-0.00289211196316079,
-0.6));
#59355=CARTESIAN_POINT('',(-0.232609869296308,-0.397107888036839,-0.6));
#59356=CARTESIAN_POINT('Ctrl Pts',(-0.232609869296308,-0.397107888036839,
-0.6));
#59357=CARTESIAN_POINT('Ctrl Pts',(-0.231776492081632,-0.398551339714529,
-0.599503641468825));
#59358=CARTESIAN_POINT('Ctrl Pts',(-0.230940107675851,-0.399999999999999,
-0.599));
#59359=CARTESIAN_POINT('',(-0.227600584434936,-0.4,-0.6));
#59360=CARTESIAN_POINT('Origin',(0.,0.,-0.6));
#59361=CARTESIAN_POINT('Ctrl Pts',(-0.23094010767585,-0.4,-0.599));
#59362=CARTESIAN_POINT('Ctrl Pts',(-0.229267338864258,-0.4,-0.599503641468835));
#59363=CARTESIAN_POINT('Ctrl Pts',(-0.227600584434936,-0.4,-0.6));
#59364=CARTESIAN_POINT('',(0.227600584434936,-0.4,-0.6));
#59365=CARTESIAN_POINT('Ctrl Pts',(0.227600584434936,-0.4,-0.6));
#59366=CARTESIAN_POINT('Ctrl Pts',(0.229267338864223,-0.4,-0.599503641468845));
#59367=CARTESIAN_POINT('Ctrl Pts',(0.23094010767585,-0.4,-0.599));
#59368=CARTESIAN_POINT('',(0.232609869296308,-0.397107888036839,-0.6));
#59369=CARTESIAN_POINT('Origin',(0.,0.,-0.6));
#59370=CARTESIAN_POINT('Ctrl Pts',(0.230940107675851,-0.399999999999999,
-0.599));
#59371=CARTESIAN_POINT('Ctrl Pts',(0.231776492081654,-0.39855133971449,
-0.599503641468839));
#59372=CARTESIAN_POINT('Ctrl Pts',(0.232609869296308,-0.397107888036839,
-0.6));
#59373=CARTESIAN_POINT('',(0.460210453731243,-0.0028921119631606,-0.6));
#59374=CARTESIAN_POINT('Ctrl Pts',(0.460210453731243,-0.00289211196316057,
-0.6));
#59375=CARTESIAN_POINT('Ctrl Pts',(0.461043830945901,-0.00144866028550258,
-0.599503641468836));
#59376=CARTESIAN_POINT('Ctrl Pts',(0.4618802153517,-7.21644966006351E-16,
-0.599));
#59377=CARTESIAN_POINT('',(0.460210453731243,0.0028921119631606,-0.6));
#59378=CARTESIAN_POINT('Origin',(0.,0.,-0.6));
#59379=CARTESIAN_POINT('Ctrl Pts',(0.4618802153517,9.15933995315753E-16,
-0.599));
#59380=CARTESIAN_POINT('Ctrl Pts',(0.461043830945894,0.00144866028551485,
-0.59950364146884));
#59381=CARTESIAN_POINT('Ctrl Pts',(0.460210453731243,0.0028921119631606,
-0.6));
#59382=CARTESIAN_POINT('',(0.232609869296308,0.397107888036839,-0.6));
#59383=CARTESIAN_POINT('Ctrl Pts',(0.232609869296308,0.397107888036839,
-0.6));
#59384=CARTESIAN_POINT('Ctrl Pts',(0.231776492081656,0.398551339714487,
-0.59950364146884));
#59385=CARTESIAN_POINT('Ctrl Pts',(0.230940107675851,0.399999999999999,
-0.599));
#59386=CARTESIAN_POINT('',(0.227600584434936,0.4,-0.6));
#59387=CARTESIAN_POINT('Origin',(0.,0.,-0.6));
#59388=CARTESIAN_POINT('Ctrl Pts',(0.23094010767585,0.4,-0.599));
#59389=CARTESIAN_POINT('Ctrl Pts',(0.229267338864267,0.4,-0.599503641468832));
#59390=CARTESIAN_POINT('Ctrl Pts',(0.227600584434936,0.4,-0.6));
#59391=CARTESIAN_POINT('',(-0.227600584434936,0.4,-0.6));
#59392=CARTESIAN_POINT('Ctrl Pts',(-0.227600584434935,0.4,-0.6));
#59393=CARTESIAN_POINT('Ctrl Pts',(-0.22926733886426,0.4,-0.599503641468834));
#59394=CARTESIAN_POINT('Ctrl Pts',(-0.230940107675849,0.4,-0.599));
#59395=CARTESIAN_POINT('',(-0.232609869296308,0.397107888036839,-0.6));
#59396=CARTESIAN_POINT('Origin',(0.,0.,-0.6));
#59397=CARTESIAN_POINT('Ctrl Pts',(-0.230940107675851,0.399999999999999,
-0.599));
#59398=CARTESIAN_POINT('Ctrl Pts',(-0.231776492081655,0.398551339714488,
-0.599503641468839));
#59399=CARTESIAN_POINT('Ctrl Pts',(-0.232609869296308,0.397107888036839,
-0.6));
#59400=CARTESIAN_POINT('',(-0.460210453731243,0.00289211196316071,-0.6));
#59401=CARTESIAN_POINT('Ctrl Pts',(-0.460210453731243,0.00289211196316076,
-0.6));
#59402=CARTESIAN_POINT('Ctrl Pts',(-0.461043830945898,0.00144866028550932,
-0.599503641468838));
#59403=CARTESIAN_POINT('Ctrl Pts',(-0.4618802153517,9.15933995315753E-16,
-0.599));
#59404=CARTESIAN_POINT('Origin',(0.,0.,-0.6));
#59405=CARTESIAN_POINT('Origin',(-0.461880215351701,5.55111512312578E-17,
0.));
#59406=CARTESIAN_POINT('',(-0.23094010767585,0.4,0.));
#59407=CARTESIAN_POINT('',(-0.23094010767585,0.4,0.));
#59408=CARTESIAN_POINT('',(-0.461880215351701,5.6564012731995E-17,0.));
#59409=CARTESIAN_POINT('',(-0.404145188432738,0.1,0.));
#59410=CARTESIAN_POINT('',(-0.461880215351701,5.6564012731995E-17,0.));
#59411=CARTESIAN_POINT('Origin',(-0.461880215351701,5.55111512312578E-17,
0.));
#59412=CARTESIAN_POINT('',(-0.461880215351701,5.55111512312578E-17,-0.6));
#59413=CARTESIAN_POINT('',(-0.461880215351701,5.6564012731995E-17,0.));
#59414=CARTESIAN_POINT('',(-0.23094010767585,0.4,-0.6));
#59415=CARTESIAN_POINT('Origin',(-0.23094010767585,0.4,0.));
#59416=CARTESIAN_POINT('',(0.23094010767585,0.4,0.));
#59417=CARTESIAN_POINT('',(0.23094010767585,0.4,0.));
#59418=CARTESIAN_POINT('',(-0.115470053837925,0.4,0.));
#59419=CARTESIAN_POINT('Origin',(-0.23094010767585,0.4,0.));
#59420=CARTESIAN_POINT('',(0.23094010767585,0.4,-0.6));
#59421=CARTESIAN_POINT('',(0.23094010767585,0.4,-0.6));
#59422=CARTESIAN_POINT('',(0.23094010767585,0.4,0.));
#59423=CARTESIAN_POINT('Origin',(-0.23094010767585,0.4,0.));
#59424=CARTESIAN_POINT('',(-0.23094010767585,0.4,-0.6));
#59425=CARTESIAN_POINT('',(-0.23094010767585,0.4,0.));
#59426=CARTESIAN_POINT('',(0.23094010767585,0.4,-0.6));
#59427=CARTESIAN_POINT('Origin',(-0.230940107675851,-0.4,0.));
#59428=CARTESIAN_POINT('',(-0.230940107675851,-0.4,0.));
#59429=CARTESIAN_POINT('',(-0.288675134594813,-0.3,0.));
#59430=CARTESIAN_POINT('',(-0.230940107675851,-0.4,0.));
#59431=CARTESIAN_POINT('Origin',(-0.230940107675851,-0.4,0.));
#59432=CARTESIAN_POINT('',(-0.230940107675851,-0.4,-0.6));
#59433=CARTESIAN_POINT('',(-0.230940107675851,-0.4,0.));
#59434=CARTESIAN_POINT('',(-0.461880215351701,5.6564012731995E-17,-0.6));
#59435=CARTESIAN_POINT('Origin',(0.23094010767585,0.4,0.));
#59436=CARTESIAN_POINT('',(0.461880215351701,0.,0.));
#59437=CARTESIAN_POINT('',(0.461880215351701,0.,0.));
#59438=CARTESIAN_POINT('',(0.288675134594813,0.3,0.));
#59439=CARTESIAN_POINT('Origin',(0.23094010767585,0.4,0.));
#59440=CARTESIAN_POINT('',(0.461880215351701,0.,-0.6));
#59441=CARTESIAN_POINT('',(0.461880215351701,0.,-0.6));
#59442=CARTESIAN_POINT('',(0.461880215351701,0.,0.));
#59443=CARTESIAN_POINT('Origin',(0.23094010767585,0.4,0.));
#59444=CARTESIAN_POINT('',(0.461880215351701,0.,-0.6));
#59445=CARTESIAN_POINT('Origin',(0.,0.,-0.6));
#59446=CARTESIAN_POINT('',(-0.23094010767585,0.4,-0.6));
#59447=CARTESIAN_POINT('Origin',(0.,0.,-0.6));
#59448=CARTESIAN_POINT('Origin',(0.,0.,-0.6));
#59449=CARTESIAN_POINT('',(0.23094010767585,-0.4,-0.6));
#59450=CARTESIAN_POINT('Origin',(0.,0.,-0.6));
#59451=CARTESIAN_POINT('',(0.23094010767585,-0.4,-0.6));
#59452=CARTESIAN_POINT('',(-0.230940107675851,-0.4,-0.6));
#59453=CARTESIAN_POINT('',(0.23094010767585,-0.4,-0.6));
#59454=CARTESIAN_POINT('Origin',(0.,0.,-0.6));
#59455=CARTESIAN_POINT('',(-0.230940107675851,-0.4,-0.6));
#59456=CARTESIAN_POINT('Origin',(0.,0.,-0.6));
#59457=CARTESIAN_POINT('',(-0.461880215351701,5.6564012731995E-17,-0.6));
#59458=CARTESIAN_POINT('Origin',(0.461880215351701,0.,0.));
#59459=CARTESIAN_POINT('',(0.23094010767585,-0.4,0.));
#59460=CARTESIAN_POINT('',(0.23094010767585,-0.4,0.));
#59461=CARTESIAN_POINT('',(0.404145188432738,-0.1,0.));
#59462=CARTESIAN_POINT('Origin',(0.461880215351701,0.,0.));
#59463=CARTESIAN_POINT('',(0.23094010767585,-0.4,0.));
#59464=CARTESIAN_POINT('Origin',(0.461880215351701,0.,0.));
#59465=CARTESIAN_POINT('Origin',(0.23094010767585,-0.4,0.));
#59466=CARTESIAN_POINT('Origin',(0.23094010767585,-0.4,0.));
#59467=CARTESIAN_POINT('',(0.115470053837925,-0.4,0.));
#59468=CARTESIAN_POINT('Origin',(-0.461880215351701,5.55111512312578E-17,
0.));
#59469=CARTESIAN_POINT('Origin',(-0.230940107675851,-0.4,0.));
#59470=CARTESIAN_POINT('Origin',(0.23094010767585,-0.4,0.));
#59471=CARTESIAN_POINT('Origin',(0.6,0.,-4.));
#59472=CARTESIAN_POINT('',(-0.6,-7.34788079488412E-17,-4.));
#59473=CARTESIAN_POINT('Origin',(0.,0.,-4.));
#59474=CARTESIAN_POINT('Origin',(0.,0.,-3.9));
#59475=CARTESIAN_POINT('',(-0.7,-8.57252759403147E-17,-3.9));
#59476=CARTESIAN_POINT('Origin',(0.,0.,-1.94));
#59477=CARTESIAN_POINT('Origin',(0.,0.,-0.0711000000000002));
#59478=CARTESIAN_POINT('Origin',(0.,0.,-0.04));
#59479=CARTESIAN_POINT('',(-0.72,-8.81745695386094E-17,-6.93889390390723E-18));
#59480=CARTESIAN_POINT('Origin',(0.,0.,0.));
#59481=CARTESIAN_POINT('',(-0.76,-9.30731567351988E-17,-0.04));
#59482=CARTESIAN_POINT('Origin',(0.,0.,0.));
#59483=CARTESIAN_POINT('',(0.,0.,0.));
#59484=CARTESIAN_POINT('Ctrl Pts',(9.74287700479826,-21.5,70.5125025877322));
#59485=CARTESIAN_POINT('Ctrl Pts',(9.74287700479826,-21.656214196966,70.5125025877322));
#59486=CARTESIAN_POINT('Ctrl Pts',(9.77861943028971,-21.9803373691276,70.5144059476976));
#59487=CARTESIAN_POINT('Ctrl Pts',(9.92068473931345,-22.3731848943024,70.5242594183206));
#59488=CARTESIAN_POINT('Ctrl Pts',(10.083942330172,-22.6596849246672,70.5396163501376));
#59489=CARTESIAN_POINT('Ctrl Pts',(10.2764424102782,-22.9226724124575,70.5614144955755));
#59490=CARTESIAN_POINT('Ctrl Pts',(10.5505406389766,-23.1948597886741,70.600128983041));
#59491=CARTESIAN_POINT('Ctrl Pts',(10.8954109293732,-23.4174824644433,70.6667169758025));
#59492=CARTESIAN_POINT('Ctrl Pts',(11.1554284786727,-23.5274756480171,70.7298614280393));
#59493=CARTESIAN_POINT('Ctrl Pts',(11.2883532161314,-23.5711895983197,70.7654371551999));
#59494=CARTESIAN_POINT('Ctrl Pts',(11.3646737922248,-23.5926452515457,70.7868530255724));
#59495=CARTESIAN_POINT('Ctrl Pts',(11.5562073871596,-23.6406588378193,70.8422231900863));
#59496=CARTESIAN_POINT('Ctrl Pts',(11.7658252370385,-23.664271882774,70.9111982308898));
#59497=CARTESIAN_POINT('Ctrl Pts',(12.0578852179822,-23.6557172786385,71.0201457155622));
#59498=CARTESIAN_POINT('Ctrl Pts',(12.2208094014591,-23.6319919884316,71.0867018338967));
#59499=CARTESIAN_POINT('Ctrl Pts',(12.3543904463612,-23.5975235527391,71.1456250307213));
#59500=CARTESIAN_POINT('Ctrl Pts',(12.4027779159087,-23.5839664204326,71.167268720936));
#59501=CARTESIAN_POINT('Ctrl Pts',(12.4866718330575,-23.5575942766802,71.2055992342487));
#59502=CARTESIAN_POINT('Ctrl Pts',(12.6510577647346,-23.4940583870137,71.2838949455475));
#59503=CARTESIAN_POINT('Ctrl Pts',(12.8719512966863,-23.3748625900797,71.3976849620357));
#59504=CARTESIAN_POINT('Ctrl Pts',(13.1084649034627,-23.1892327479386,71.5314239215564));
#59505=CARTESIAN_POINT('Ctrl Pts',(13.3051919767247,-22.9780992092235,71.6514654851331));
#59506=CARTESIAN_POINT('Ctrl Pts',(13.4763850760173,-22.7304324210399,71.7627534820972));
#59507=CARTESIAN_POINT('Ctrl Pts',(13.6168015105668,-22.4461912796831,71.8592569555153));
#59508=CARTESIAN_POINT('Ctrl Pts',(13.709674381118,-22.1641725337909,71.9258725275639));
#59509=CARTESIAN_POINT('Ctrl Pts',(13.7535308851104,-21.9512225876456,71.9580350138515));
#59510=CARTESIAN_POINT('Ctrl Pts',(13.7979233224896,-21.6302708884948,71.9909065809688));
#59511=CARTESIAN_POINT('Ctrl Pts',(13.7985524061519,-21.2911597238678,71.9912918069344));
#59512=CARTESIAN_POINT('Ctrl Pts',(13.7183983186692,-20.8609704899414,71.932093483098));
#59513=CARTESIAN_POINT('Ctrl Pts',(13.6166712998014,-20.5540190040535,71.8591758531238));
#59514=CARTESIAN_POINT('Ctrl Pts',(13.4764722169006,-20.2695559196014,71.7628122981255));
#59515=CARTESIAN_POINT('Ctrl Pts',(13.30479452339,-20.0214367560947,71.6512132027746));
#59516=CARTESIAN_POINT('Ctrl Pts',(13.108633737568,-19.8110230421895,71.5315418245281));
#59517=CARTESIAN_POINT('Ctrl Pts',(12.9112681237482,-19.656071853345,71.4199434952884));
#59518=CARTESIAN_POINT('Ctrl Pts',(12.6535693601998,-19.5026800844597,71.2842239697829));
#59519=CARTESIAN_POINT('Ctrl Pts',(12.3693061289729,-19.3924814953289,71.1481752603989));
#59520=CARTESIAN_POINT('Ctrl Pts',(12.0216107241993,-19.338052834614,71.005036372742));
#59521=CARTESIAN_POINT('Ctrl Pts',(11.6310650689274,-19.3376578948939,70.8625951386498));
#59522=CARTESIAN_POINT('Ctrl Pts',(11.1091117678361,-19.4569229967783,70.7097325311002));
#59523=CARTESIAN_POINT('Ctrl Pts',(10.5875357806613,-19.7677773346453,70.6053394071194));
#59524=CARTESIAN_POINT('Ctrl Pts',(10.3040349212154,-20.0501861211832,70.5653346387674));
#59525=CARTESIAN_POINT('Ctrl Pts',(10.1066531997307,-20.305521444769,70.5419005952258));
#59526=CARTESIAN_POINT('Ctrl Pts',(9.93487527850697,-20.5875814819759,70.5252370307246));
#59527=CARTESIAN_POINT('Ctrl Pts',(9.77867795084425,-21.0196494588534,70.5144182338898));
#59528=CARTESIAN_POINT('Ctrl Pts',(9.74287700479826,-21.3437858030339,70.5125025877322));
#59529=CARTESIAN_POINT('Ctrl Pts',(9.74287700479826,-21.5,70.5125025877322));
#59530=CARTESIAN_POINT('Ctrl Pts',(9.77566129268524,-21.5,70.5628720876684));
#59531=CARTESIAN_POINT('Ctrl Pts',(9.77566129268524,-21.6534741316411,70.5628720876684));
#59532=CARTESIAN_POINT('Ctrl Pts',(9.81099168028511,-21.9719192919697,70.5650519513878));
#59533=CARTESIAN_POINT('Ctrl Pts',(9.95117347313436,-22.3572458209345,70.5758665902743));
#59534=CARTESIAN_POINT('Ctrl Pts',(10.1118579963003,-22.6376328078247,70.5920838302201));
#59535=CARTESIAN_POINT('Ctrl Pts',(10.3009739420384,-22.8945540804684,70.6146705888467));
#59536=CARTESIAN_POINT('Ctrl Pts',(10.5695498424849,-23.1596691288769,70.6540368613604));
#59537=CARTESIAN_POINT('Ctrl Pts',(10.9060823062057,-23.3756123556826,70.7203264012894));
#59538=CARTESIAN_POINT('Ctrl Pts',(11.1590889733824,-23.4820149939127,70.7824430077388));
#59539=CARTESIAN_POINT('Ctrl Pts',(11.2883004649771,-23.5242631039492,70.8172953874664));
#59540=CARTESIAN_POINT('Ctrl Pts',(11.3624559776584,-23.5449889102041,70.838237600039));
#59541=CARTESIAN_POINT('Ctrl Pts',(11.5485093899437,-23.5913547053039,70.8923250019762));
#59542=CARTESIAN_POINT('Ctrl Pts',(11.7519243617111,-23.6141195484566,70.959414244256));
#59543=CARTESIAN_POINT('Ctrl Pts',(12.0354296368004,-23.6058714701567,71.0651137905936));
#59544=CARTESIAN_POINT('Ctrl Pts',(12.193665998477,-23.5829845184256,71.1295980617617));
#59545=CARTESIAN_POINT('Ctrl Pts',(12.3235593632531,-23.5497000132635,71.1866674340606));
#59546=CARTESIAN_POINT('Ctrl Pts',(12.3706227200289,-23.5366057407861,71.2076295818757));
#59547=CARTESIAN_POINT('Ctrl Pts',(12.4522536209234,-23.5111271728441,71.2447520528871));
#59548=CARTESIAN_POINT('Ctrl Pts',(12.6123491063975,-23.4497024850363,71.3205844405804));
#59549=CARTESIAN_POINT('Ctrl Pts',(12.8279339405974,-23.3343024876679,71.4308465647072));
#59550=CARTESIAN_POINT('Ctrl Pts',(13.0595565632642,-23.1540884860638,71.5606184977724));
#59551=CARTESIAN_POINT('Ctrl Pts',(13.2528809724359,-22.9485568459442,71.6772866701138));
#59552=CARTESIAN_POINT('Ctrl Pts',(13.4216736669167,-22.7068367362783,71.785623374226));
#59553=CARTESIAN_POINT('Ctrl Pts',(13.5605733827612,-22.4287379648088,71.8797176190141));
#59554=CARTESIAN_POINT('Ctrl Pts',(13.6526950213329,-22.1522500472725,71.9447564871425));
#59555=CARTESIAN_POINT('Ctrl Pts',(13.6962620308405,-21.9432179955209,71.976180116676));
#59556=CARTESIAN_POINT('Ctrl Pts',(13.740391047937,-21.6280318714313,72.0083066859187));
#59557=CARTESIAN_POINT('Ctrl Pts',(13.7410087312265,-21.2947483967792,72.0086804998937));
#59558=CARTESIAN_POINT('Ctrl Pts',(13.6613448700357,-20.8723984338637,71.9508289201672));
#59559=CARTESIAN_POINT('Ctrl Pts',(13.5604453574354,-20.5714697858188,71.8796387836749));
#59560=CARTESIAN_POINT('Ctrl Pts',(13.4217594678946,-20.2931514421549,71.7856804754748));
#59561=CARTESIAN_POINT('Ctrl Pts',(13.2524898178296,-20.0509908996673,71.6770412767522));
#59562=CARTESIAN_POINT('Ctrl Pts',(13.0597225605965,-19.8461608875654,71.5607328512164));
#59563=CARTESIAN_POINT('Ctrl Pts',(12.8664408368138,-19.695729310016,71.4524457223248));
#59564=CARTESIAN_POINT('Ctrl Pts',(12.6147312978391,-19.5471004559845,71.320886585664));
#59565=CARTESIAN_POINT('Ctrl Pts',(12.3379146864166,-19.4406307679279,71.1891521581768));
#59566=CARTESIAN_POINT('Ctrl Pts',(12.0001882251287,-19.3881193545174,71.0504767635001));
#59567=CARTESIAN_POINT('Ctrl Pts',(11.621154655613,-19.3877604898925,70.9122445590948));
#59568=CARTESIAN_POINT('Ctrl Pts',(11.1144403261534,-19.5027306944885,70.7630434730559));
#59569=CARTESIAN_POINT('Ctrl Pts',(10.6058218204276,-19.8039173677725,70.659337688344));
#59570=CARTESIAN_POINT('Ctrl Pts',(10.3280066988785,-20.0790135058352,70.6186547075878));
#59571=CARTESIAN_POINT('Ctrl Pts',(10.134197724029,-20.3283456136423,70.5944789024564));
#59572=CARTESIAN_POINT('Ctrl Pts',(9.96517644530526,-20.6042709357116,70.5769404654071));
#59573=CARTESIAN_POINT('Ctrl Pts',(9.8110491734264,-21.0280688465375,70.5650642368601));
#59574=CARTESIAN_POINT('Ctrl Pts',(9.77566129268524,-21.3465258683589,70.5628720876684));
#59575=CARTESIAN_POINT('Ctrl Pts',(9.77566129268524,-21.5,70.5628720876684));
#59576=CARTESIAN_POINT('Ctrl Pts',(9.80844558057222,-21.5,70.6132415876045));
#59577=CARTESIAN_POINT('Ctrl Pts',(9.80844558057222,-21.6507340663161,70.6132415876045));
#59578=CARTESIAN_POINT('Ctrl Pts',(9.84336393028051,-21.9635012148119,70.615697955078));
#59579=CARTESIAN_POINT('Ctrl Pts',(9.98166220695528,-22.3413067475665,70.6274737622279));
#59580=CARTESIAN_POINT('Ctrl Pts',(10.1397736624286,-22.6155806909822,70.6445513103028));
#59581=CARTESIAN_POINT('Ctrl Pts',(10.3255054737985,-22.8664357484793,70.667926682118));
#59582=CARTESIAN_POINT('Ctrl Pts',(10.5885590459932,-23.1244784690798,70.7079447396797));
#59583=CARTESIAN_POINT('Ctrl Pts',(10.9167536830382,-23.333742246922,70.7739358267763));
#59584=CARTESIAN_POINT('Ctrl Pts',(11.1627494680922,-23.4365543398082,70.8350245874384));
#59585=CARTESIAN_POINT('Ctrl Pts',(11.2882477138228,-23.4773366095787,70.869153619733));
#59586=CARTESIAN_POINT('Ctrl Pts',(11.360238163092,-23.4973325688625,70.8896221745056));
#59587=CARTESIAN_POINT('Ctrl Pts',(11.5408113927277,-23.5420505727884,70.9424268138662));
#59588=CARTESIAN_POINT('Ctrl Pts',(11.7380234863837,-23.5639672141393,71.0076302576221));
#59589=CARTESIAN_POINT('Ctrl Pts',(12.0129740556185,-23.5560256616749,71.1100818656249));
#59590=CARTESIAN_POINT('Ctrl Pts',(12.1665225954948,-23.5339770484196,71.1724942896266));
#59591=CARTESIAN_POINT('Ctrl Pts',(12.2927282801449,-23.5018764737878,71.2277098374));
#59592=CARTESIAN_POINT('Ctrl Pts',(12.3384675241492,-23.4892450611396,71.2479904428155));
#59593=CARTESIAN_POINT('Ctrl Pts',(12.4178354087892,-23.4646600690079,71.2839048715255));
#59594=CARTESIAN_POINT('Ctrl Pts',(12.5736404480604,-23.4053465830588,71.3572739356134));
#59595=CARTESIAN_POINT('Ctrl Pts',(12.7839165845085,-23.2937423852561,71.4640081673788));
#59596=CARTESIAN_POINT('Ctrl Pts',(13.0106482230657,-23.118944224189,71.5898130739885));
#59597=CARTESIAN_POINT('Ctrl Pts',(13.2005699681471,-22.919014482665,71.7031078550945));
#59598=CARTESIAN_POINT('Ctrl Pts',(13.366962257816,-22.6832410515167,71.8084932663548));
#59599=CARTESIAN_POINT('Ctrl Pts',(13.5043452549556,-22.4112846499345,71.9001782825129));
#59600=CARTESIAN_POINT('Ctrl Pts',(13.5957156615478,-22.1403275607541,71.9636404467212));
#59601=CARTESIAN_POINT('Ctrl Pts',(13.6389931765705,-21.9352134033963,71.9943252195005));
#59602=CARTESIAN_POINT('Ctrl Pts',(13.6828587733844,-21.6257928543678,72.0257067908687));
#59603=CARTESIAN_POINT('Ctrl Pts',(13.6834650563012,-21.2983370696906,72.0260691928531));
#59604=CARTESIAN_POINT('Ctrl Pts',(13.6042914214022,-20.883826377786,71.9695643572363));
#59605=CARTESIAN_POINT('Ctrl Pts',(13.5042194150694,-20.588920567584,71.900101714226));
#59606=CARTESIAN_POINT('Ctrl Pts',(13.3670467188885,-20.3167469647085,71.808548652824));
#59607=CARTESIAN_POINT('Ctrl Pts',(13.2001851122691,-20.0805450432399,71.7028693507298));
#59608=CARTESIAN_POINT('Ctrl Pts',(13.0108113836249,-19.8812987329413,71.5899238779046));
#59609=CARTESIAN_POINT('Ctrl Pts',(12.8216135498794,-19.7353867666869,71.4849479493612));
#59610=CARTESIAN_POINT('Ctrl Pts',(12.5758932354784,-19.5915208275092,71.3575492015453));
#59611=CARTESIAN_POINT('Ctrl Pts',(12.3065232438603,-19.4887800405268,71.2301290559547));
#59612=CARTESIAN_POINT('Ctrl Pts',(11.9787657260582,-19.4381858744207,71.0959171542583));
#59613=CARTESIAN_POINT('Ctrl Pts',(11.6112442422986,-19.4378630848911,70.9618939795399));
#59614=CARTESIAN_POINT('Ctrl Pts',(11.1197688844706,-19.5485383921987,70.8163544150116));
#59615=CARTESIAN_POINT('Ctrl Pts',(10.624107860194,-19.8400574008998,70.7133359695685));
#59616=CARTESIAN_POINT('Ctrl Pts',(10.3519784765416,-20.1078408904872,70.6719747764082));
#59617=CARTESIAN_POINT('Ctrl Pts',(10.1617422483273,-20.3511697825156,70.6470572096869));
#59618=CARTESIAN_POINT('Ctrl Pts',(9.99547761210354,-20.6209603894473,70.6286439000895));
#59619=CARTESIAN_POINT('Ctrl Pts',(9.84342039600855,-21.0364882342215,70.6157102398303));
#59620=CARTESIAN_POINT('Ctrl Pts',(9.80844558057223,-21.3492659336839,70.6132415876045));
#59621=CARTESIAN_POINT('Ctrl Pts',(9.80844558057223,-21.5,70.6132415876045));
#59622=CARTESIAN_POINT('Ctrl Pts',(9.8412298684592,-21.5,70.6636110875407));
#59623=CARTESIAN_POINT('Ctrl Pts',(9.8412298684592,-21.6479940009911,70.6636110875407));
#59624=CARTESIAN_POINT('Ctrl Pts',(9.87573618027591,-21.9550831376541,70.6663439587683));
#59625=CARTESIAN_POINT('Ctrl Pts',(10.0121509407762,-22.3253676741985,70.6790809341815));
#59626=CARTESIAN_POINT('Ctrl Pts',(10.1676893285569,-22.5935285741397,70.6970187903853));
#59627=CARTESIAN_POINT('Ctrl Pts',(10.3500370055587,-22.8383174164902,70.7211827753892));
#59628=CARTESIAN_POINT('Ctrl Pts',(10.6075682495015,-23.0892878092826,70.7618526179991));
#59629=CARTESIAN_POINT('Ctrl Pts',(10.9274250598707,-23.2918721381614,70.8275452522632));
#59630=CARTESIAN_POINT('Ctrl Pts',(11.1664099628019,-23.3910936857038,70.8876061671379));
#59631=CARTESIAN_POINT('Ctrl Pts',(11.2881949626684,-23.4304101152083,70.9210118519996));
#59632=CARTESIAN_POINT('Ctrl Pts',(11.3580203485256,-23.4496762275209,70.9410067489722));
#59633=CARTESIAN_POINT('Ctrl Pts',(11.5331133955118,-23.4927464402729,70.9925286257561));
#59634=CARTESIAN_POINT('Ctrl Pts',(11.7241226110564,-23.513814879822,71.0558462709882));
#59635=CARTESIAN_POINT('Ctrl Pts',(11.9905184744366,-23.5061798531931,71.1550499406563));
#59636=CARTESIAN_POINT('Ctrl Pts',(12.1393791925127,-23.4849695784135,71.2153905174916));
#59637=CARTESIAN_POINT('Ctrl Pts',(12.2618971970367,-23.4540529343121,71.2687522407393));
#59638=CARTESIAN_POINT('Ctrl Pts',(12.3063123282695,-23.4418843814931,71.2883513037553));
#59639=CARTESIAN_POINT('Ctrl Pts',(12.3834171966551,-23.4181929651718,71.3230576901639));
#59640=CARTESIAN_POINT('Ctrl Pts',(12.5349317897233,-23.3609906810814,71.3939634306464));
#59641=CARTESIAN_POINT('Ctrl Pts',(12.7398992284196,-23.2531822828443,71.4971697700503));
#59642=CARTESIAN_POINT('Ctrl Pts',(12.9617398828672,-23.0837999623142,71.6190076502045));
#59643=CARTESIAN_POINT('Ctrl Pts',(13.1482589638583,-22.8894721193857,71.7289290400752));
#59644=CARTESIAN_POINT('Ctrl Pts',(13.3122508487154,-22.6596453667551,71.8313631584836));
#59645=CARTESIAN_POINT('Ctrl Pts',(13.4481171271501,-22.3938313350602,71.9206389460116));
#59646=CARTESIAN_POINT('Ctrl Pts',(13.5387363017626,-22.1284050742357,71.9825244062999));
#59647=CARTESIAN_POINT('Ctrl Pts',(13.5817243223006,-21.9272088112716,72.012470322325));
#59648=CARTESIAN_POINT('Ctrl Pts',(13.6253264988318,-21.6235538373044,72.0431068958186));
#59649=CARTESIAN_POINT('Ctrl Pts',(13.6259213813758,-21.301925742602,72.0434578858125));
#59650=CARTESIAN_POINT('Ctrl Pts',(13.5472379727687,-20.8952543217083,71.9882997943055));
#59651=CARTESIAN_POINT('Ctrl Pts',(13.4479934727035,-20.6063713493493,71.9205646447771));
#59652=CARTESIAN_POINT('Ctrl Pts',(13.3123339698825,-20.340342487262,71.8314168301733));
#59653=CARTESIAN_POINT('Ctrl Pts',(13.1478804067087,-20.1100991868126,71.7286974247074));
#59654=CARTESIAN_POINT('Ctrl Pts',(12.9619002066534,-19.9164365783173,71.6191149045929));
#59655=CARTESIAN_POINT('Ctrl Pts',(12.7767862629449,-19.7750442233578,71.5174501763976));
#59656=CARTESIAN_POINT('Ctrl Pts',(12.5370551731176,-19.6359411990339,71.3942118174265));
#59657=CARTESIAN_POINT('Ctrl Pts',(12.275131801304,-19.5369293131258,71.2711059537325));
#59658=CARTESIAN_POINT('Ctrl Pts',(11.9573432269876,-19.4882523943241,71.1413575450164));
#59659=CARTESIAN_POINT('Ctrl Pts',(11.6013338289841,-19.4879656798897,71.011543399985));
#59660=CARTESIAN_POINT('Ctrl Pts',(11.1250974427879,-19.5943460899089,70.8696653569674));
#59661=CARTESIAN_POINT('Ctrl Pts',(10.6423938999603,-19.876197434027,70.7673342507931));
#59662=CARTESIAN_POINT('Ctrl Pts',(10.3759502542046,-20.1366682751392,70.7252948452286));
#59663=CARTESIAN_POINT('Ctrl Pts',(10.1892867726256,-20.3739939513888,70.6996355169175));
#59664=CARTESIAN_POINT('Ctrl Pts',(10.0257787789018,-20.637649843183,70.6803473347719));
#59665=CARTESIAN_POINT('Ctrl Pts',(9.8757916185907,-21.0449076219056,70.6663562428006));
#59666=CARTESIAN_POINT('Ctrl Pts',(9.84122986845921,-21.3520059990089,70.6636110875407));
#59667=CARTESIAN_POINT('Ctrl Pts',(9.84122986845921,-21.5,70.6636110875407));
#59668=CARTESIAN_POINT('',(9.74287700479826,-21.5,70.5125025877322));
#59669=CARTESIAN_POINT('',(9.8412298684592,-21.5,70.6636110875407));
#59670=CARTESIAN_POINT('',(9.74287700479826,-21.5,70.5125025877322));
#59671=CARTESIAN_POINT('Ctrl Pts',(9.8412298684592,-21.5,70.6636110875407));
#59672=CARTESIAN_POINT('Ctrl Pts',(9.8412298684592,-21.6479940009911,70.6636110875407));
#59673=CARTESIAN_POINT('Ctrl Pts',(9.87573618027591,-21.9550831376541,70.6663439587683));
#59674=CARTESIAN_POINT('Ctrl Pts',(10.0121509407762,-22.3253676741985,70.6790809341815));
#59675=CARTESIAN_POINT('Ctrl Pts',(10.1676893285569,-22.5935285741397,70.6970187903853));
#59676=CARTESIAN_POINT('Ctrl Pts',(10.3500370055587,-22.8383174164902,70.7211827753892));
#59677=CARTESIAN_POINT('Ctrl Pts',(10.6075682495015,-23.0892878092826,70.7618526179991));
#59678=CARTESIAN_POINT('Ctrl Pts',(10.9274250598707,-23.2918721381614,70.8275452522632));
#59679=CARTESIAN_POINT('Ctrl Pts',(11.1664099628019,-23.3910936857038,70.8876061671379));
#59680=CARTESIAN_POINT('Ctrl Pts',(11.2881949626684,-23.4304101152083,70.9210118519996));
#59681=CARTESIAN_POINT('Ctrl Pts',(11.3580203485256,-23.4496762275209,70.9410067489722));
#59682=CARTESIAN_POINT('Ctrl Pts',(11.5331133955118,-23.4927464402729,70.9925286257561));
#59683=CARTESIAN_POINT('Ctrl Pts',(11.7241226110564,-23.513814879822,71.0558462709882));
#59684=CARTESIAN_POINT('Ctrl Pts',(11.9905184744366,-23.5061798531931,71.1550499406563));
#59685=CARTESIAN_POINT('Ctrl Pts',(12.1393791925127,-23.4849695784135,71.2153905174916));
#59686=CARTESIAN_POINT('Ctrl Pts',(12.2618971970367,-23.4540529343121,71.2687522407393));
#59687=CARTESIAN_POINT('Ctrl Pts',(12.3063123282695,-23.4418843814931,71.2883513037553));
#59688=CARTESIAN_POINT('Ctrl Pts',(12.3834171966551,-23.4181929651718,71.3230576901639));
#59689=CARTESIAN_POINT('Ctrl Pts',(12.5349317897233,-23.3609906810814,71.3939634306464));
#59690=CARTESIAN_POINT('Ctrl Pts',(12.7398992284196,-23.2531822828443,71.4971697700503));
#59691=CARTESIAN_POINT('Ctrl Pts',(12.9617398828672,-23.0837999623142,71.6190076502045));
#59692=CARTESIAN_POINT('Ctrl Pts',(13.1482589638583,-22.8894721193857,71.7289290400752));
#59693=CARTESIAN_POINT('Ctrl Pts',(13.3122508487154,-22.6596453667551,71.8313631584836));
#59694=CARTESIAN_POINT('Ctrl Pts',(13.4481171271501,-22.3938313350602,71.9206389460116));
#59695=CARTESIAN_POINT('Ctrl Pts',(13.5387363017626,-22.1284050742357,71.9825244062999));
#59696=CARTESIAN_POINT('Ctrl Pts',(13.5817243223006,-21.9272088112716,72.012470322325));
#59697=CARTESIAN_POINT('Ctrl Pts',(13.6253264988318,-21.6235538373044,72.0431068958186));
#59698=CARTESIAN_POINT('Ctrl Pts',(13.6259213813758,-21.301925742602,72.0434578858125));
#59699=CARTESIAN_POINT('Ctrl Pts',(13.5472379727687,-20.8952543217083,71.9882997943055));
#59700=CARTESIAN_POINT('Ctrl Pts',(13.4479934727035,-20.6063713493493,71.9205646447771));
#59701=CARTESIAN_POINT('Ctrl Pts',(13.3123339698825,-20.340342487262,71.8314168301733));
#59702=CARTESIAN_POINT('Ctrl Pts',(13.1478804067087,-20.1100991868126,71.7286974247074));
#59703=CARTESIAN_POINT('Ctrl Pts',(12.9619002066534,-19.9164365783173,71.6191149045929));
#59704=CARTESIAN_POINT('Ctrl Pts',(12.7767862629449,-19.7750442233578,71.5174501763976));
#59705=CARTESIAN_POINT('Ctrl Pts',(12.5370551731176,-19.6359411990339,71.3942118174265));
#59706=CARTESIAN_POINT('Ctrl Pts',(12.275131801304,-19.5369293131258,71.2711059537325));
#59707=CARTESIAN_POINT('Ctrl Pts',(11.9573432269876,-19.4882523943241,71.1413575450164));
#59708=CARTESIAN_POINT('Ctrl Pts',(11.6013338289841,-19.4879656798897,71.011543399985));
#59709=CARTESIAN_POINT('Ctrl Pts',(11.1250974427879,-19.5943460899089,70.8696653569674));
#59710=CARTESIAN_POINT('Ctrl Pts',(10.6423938999603,-19.876197434027,70.7673342507931));
#59711=CARTESIAN_POINT('Ctrl Pts',(10.3759502542046,-20.1366682751392,70.7252948452286));
#59712=CARTESIAN_POINT('Ctrl Pts',(10.1892867726256,-20.3739939513888,70.6996355169175));
#59713=CARTESIAN_POINT('Ctrl Pts',(10.0257787789018,-20.637649843183,70.6803473347719));
#59714=CARTESIAN_POINT('Ctrl Pts',(9.8757916185907,-21.0449076219056,70.6663562428006));
#59715=CARTESIAN_POINT('Ctrl Pts',(9.84122986845921,-21.3520059990089,70.6636110875407));
#59716=CARTESIAN_POINT('Ctrl Pts',(9.84122986845921,-21.5,70.6636110875407));
#59717=CARTESIAN_POINT('Ctrl Pts',(9.74287700479826,-21.5,70.5125025877322));
#59718=CARTESIAN_POINT('Ctrl Pts',(9.74287700479826,-21.3437858030339,70.5125025877322));
#59719=CARTESIAN_POINT('Ctrl Pts',(9.77867795084425,-21.0196494588534,70.5144182338898));
#59720=CARTESIAN_POINT('Ctrl Pts',(9.93487527850697,-20.5875814819759,70.5252370307246));
#59721=CARTESIAN_POINT('Ctrl Pts',(10.1066531997307,-20.305521444769,70.5419005952258));
#59722=CARTESIAN_POINT('Ctrl Pts',(10.3040349212154,-20.0501861211832,70.5653346387674));
#59723=CARTESIAN_POINT('Ctrl Pts',(10.5875357806613,-19.7677773346453,70.6053394071194));
#59724=CARTESIAN_POINT('Ctrl Pts',(11.1091117678361,-19.4569229967783,70.7097325311002));
#59725=CARTESIAN_POINT('Ctrl Pts',(11.6310650689274,-19.3376578948939,70.8625951386498));
#59726=CARTESIAN_POINT('Ctrl Pts',(12.0216107241993,-19.338052834614,71.005036372742));
#59727=CARTESIAN_POINT('Ctrl Pts',(12.3693061289729,-19.3924814953289,71.1481752603989));
#59728=CARTESIAN_POINT('Ctrl Pts',(12.6535693601998,-19.5026800844597,71.2842239697829));
#59729=CARTESIAN_POINT('Ctrl Pts',(12.9112681237482,-19.656071853345,71.4199434952884));
#59730=CARTESIAN_POINT('Ctrl Pts',(13.108633737568,-19.8110230421895,71.5315418245281));
#59731=CARTESIAN_POINT('Ctrl Pts',(13.30479452339,-20.0214367560947,71.6512132027746));
#59732=CARTESIAN_POINT('Ctrl Pts',(13.4764722169006,-20.2695559196014,71.7628122981255));
#59733=CARTESIAN_POINT('Ctrl Pts',(13.6166712998014,-20.5540190040535,71.8591758531238));
#59734=CARTESIAN_POINT('Ctrl Pts',(13.7183983186692,-20.8609704899414,71.932093483098));
#59735=CARTESIAN_POINT('Ctrl Pts',(13.7985524061519,-21.2911597238678,71.9912918069344));
#59736=CARTESIAN_POINT('Ctrl Pts',(13.7979233224896,-21.6302708884948,71.9909065809688));
#59737=CARTESIAN_POINT('Ctrl Pts',(13.7535308851104,-21.9512225876456,71.9580350138515));
#59738=CARTESIAN_POINT('Ctrl Pts',(13.709674381118,-22.1641725337909,71.9258725275639));
#59739=CARTESIAN_POINT('Ctrl Pts',(13.6168015105668,-22.4461912796831,71.8592569555153));
#59740=CARTESIAN_POINT('Ctrl Pts',(13.4763850760173,-22.7304324210399,71.7627534820972));
#59741=CARTESIAN_POINT('Ctrl Pts',(13.3051919767247,-22.9780992092235,71.6514654851331));
#59742=CARTESIAN_POINT('Ctrl Pts',(13.1084649034627,-23.1892327479386,71.5314239215564));
#59743=CARTESIAN_POINT('Ctrl Pts',(12.8719512966863,-23.3748625900797,71.3976849620357));
#59744=CARTESIAN_POINT('Ctrl Pts',(12.6510577647346,-23.4940583870137,71.2838949455475));
#59745=CARTESIAN_POINT('Ctrl Pts',(12.4866718330575,-23.5575942766802,71.2055992342487));
#59746=CARTESIAN_POINT('Ctrl Pts',(12.4027779159087,-23.5839664204326,71.167268720936));
#59747=CARTESIAN_POINT('Ctrl Pts',(12.3543904463612,-23.5975235527391,71.1456250307213));
#59748=CARTESIAN_POINT('Ctrl Pts',(12.2208094014591,-23.6319919884316,71.0867018338967));
#59749=CARTESIAN_POINT('Ctrl Pts',(12.0578852179822,-23.6557172786385,71.0201457155622));
#59750=CARTESIAN_POINT('Ctrl Pts',(11.7658252370385,-23.664271882774,70.9111982308898));
#59751=CARTESIAN_POINT('Ctrl Pts',(11.5562073871596,-23.6406588378193,70.8422231900863));
#59752=CARTESIAN_POINT('Ctrl Pts',(11.3646737922248,-23.5926452515457,70.7868530255724));
#59753=CARTESIAN_POINT('Ctrl Pts',(11.2883532161314,-23.5711895983197,70.7654371551999));
#59754=CARTESIAN_POINT('Ctrl Pts',(11.1554284786727,-23.5274756480171,70.7298614280393));
#59755=CARTESIAN_POINT('Ctrl Pts',(10.8954109293732,-23.4174824644433,70.6667169758025));
#59756=CARTESIAN_POINT('Ctrl Pts',(10.5505406389766,-23.1948597886741,70.600128983041));
#59757=CARTESIAN_POINT('Ctrl Pts',(10.2764424102782,-22.9226724124575,70.5614144955755));
#59758=CARTESIAN_POINT('Ctrl Pts',(10.083942330172,-22.6596849246672,70.5396163501376));
#59759=CARTESIAN_POINT('Ctrl Pts',(9.92068473931345,-22.3731848943024,70.5242594183206));
#59760=CARTESIAN_POINT('Ctrl Pts',(9.77861943028971,-21.9803373691276,70.5144059476976));
#59761=CARTESIAN_POINT('Ctrl Pts',(9.74287700479826,-21.656214196966,70.5125025877322));
#59762=CARTESIAN_POINT('Ctrl Pts',(9.74287700479826,-21.5,70.5125025877322));
#59763=CARTESIAN_POINT('Origin',(9.31,-19.775,78.));
#59764=CARTESIAN_POINT('',(1.81,-25.3,78.));
#59765=CARTESIAN_POINT('Origin',(9.31,-25.3,78.));
#59766=CARTESIAN_POINT('',(1.81,-14.25,78.));
#59767=CARTESIAN_POINT('',(1.81,-19.775,78.));
#59768=CARTESIAN_POINT('Origin',(9.31,-14.25,78.));
#59769=CARTESIAN_POINT('',(4.82873245991394,-21.5,84.014003760738));
#59770=CARTESIAN_POINT('Ctrl Pts',(4.82873245991394,-21.5,84.014003760738));
#59771=CARTESIAN_POINT('Ctrl Pts',(4.82873245991394,-21.6562141969661,84.014003760738));
#59772=CARTESIAN_POINT('Ctrl Pts',(4.85736622748711,-21.9803502519472,84.0355447824565));
#59773=CARTESIAN_POINT('Ctrl Pts',(4.98401828163431,-22.4124109055271,84.1276650488678));
#59774=CARTESIAN_POINT('Ctrl Pts',(5.12625478749138,-22.6944732941622,84.2253058354118));
#59775=CARTESIAN_POINT('Ctrl Pts',(5.2926198619563,-22.9497986695551,84.3342442319345));
#59776=CARTESIAN_POINT('Ctrl Pts',(5.53493133383187,-23.2322336732833,84.4857324948551));
#59777=CARTESIAN_POINT('Ctrl Pts',(5.89665156355806,-23.4723187384843,84.6831785101655));
#59778=CARTESIAN_POINT('Ctrl Pts',(6.2753117530903,-23.6086799844817,84.8611083880992));
#59779=CARTESIAN_POINT('Ctrl Pts',(6.57408560510447,-23.662351077972,84.9862512166584));
#59780=CARTESIAN_POINT('Ctrl Pts',(6.89079758792843,-23.6619346851716,85.1014126433423));
#59781=CARTESIAN_POINT('Ctrl Pts',(7.14703055733959,-23.6230346405478,85.1827564818876));
#59782=CARTESIAN_POINT('Ctrl Pts',(7.45300707834779,-23.5382170209426,85.2689305062561));
#59783=CARTESIAN_POINT('Ctrl Pts',(7.75038779391833,-23.4057620043471,85.3390556557566));
#59784=CARTESIAN_POINT('Ctrl Pts',(8.06196599656662,-23.1891502055613,85.3968111581528));
#59785=CARTESIAN_POINT('Ctrl Pts',(8.28948884338796,-22.9784739218892,85.4312988805198));
#59786=CARTESIAN_POINT('Ctrl Pts',(8.47541979746267,-22.7514824404779,85.4540052246341));
#59787=CARTESIAN_POINT('Ctrl Pts',(8.59144124522549,-22.5645860879582,85.4656428345252));
#59788=CARTESIAN_POINT('Ctrl Pts',(8.74391346127118,-22.272332044321,85.4793401936152));
#59789=CARTESIAN_POINT('Ctrl Pts',(8.85381443839301,-21.9240224696184,85.4861466895026));
#59790=CARTESIAN_POINT('Ctrl Pts',(8.87901361505321,-21.5779256266326,85.487614474219));
#59791=CARTESIAN_POINT('Ctrl Pts',(8.87516743536897,-21.3694798611557,85.4873864938745));
#59792=CARTESIAN_POINT('Ctrl Pts',(8.85513326762087,-21.1553648060587,85.48622725368));
#59793=CARTESIAN_POINT('Ctrl Pts',(8.78657759480108,-20.8615791622571,85.4819283317405));
#59794=CARTESIAN_POINT('Ctrl Pts',(8.6617617762221,-20.5533339316959,85.4724237592255));
#59795=CARTESIAN_POINT('Ctrl Pts',(8.53517073786835,-20.3410662633443,85.4602233453799));
#59796=CARTESIAN_POINT('Ctrl Pts',(8.40767692089607,-20.1659139729294,85.4457557150761));
#59797=CARTESIAN_POINT('Ctrl Pts',(8.27089129566994,-20.0045077474062,85.4284509108725));
#59798=CARTESIAN_POINT('Ctrl Pts',(8.06181738257177,-19.8106817132535,85.3968159991057));
#59799=CARTESIAN_POINT('Ctrl Pts',(7.82802168890365,-19.6482675713107,85.3534138355257));
#59800=CARTESIAN_POINT('Ctrl Pts',(7.63726184737735,-19.5478095215932,85.3116066824435));
#59801=CARTESIAN_POINT('Ctrl Pts',(7.48927323429437,-19.4831548365047,85.2760681754352));
#59802=CARTESIAN_POINT('Ctrl Pts',(7.37608465013576,-19.4424658819364,85.2467130241579));
#59803=CARTESIAN_POINT('Ctrl Pts',(7.29030926384011,-19.4169940333725,85.2230170810003));
#59804=CARTESIAN_POINT('Ctrl Pts',(7.25209035941627,-19.406734446681,85.2121572627922));
#59805=CARTESIAN_POINT('Ctrl Pts',(7.2266071958566,-19.4001505834634,85.2048434726207));
#59806=CARTESIAN_POINT('Ctrl Pts',(7.05731504363103,-19.3586067795117,85.1556486945886));
#59807=CARTESIAN_POINT('Ctrl Pts',(6.83602917970007,-19.3336186512925,85.0828499150213));
#59808=CARTESIAN_POINT('Ctrl Pts',(6.54311667666213,-19.3463797210142,84.9723056198425));
#59809=CARTESIAN_POINT('Ctrl Pts',(6.38396293084926,-19.3722629250898,84.9064904925777));
#59810=CARTESIAN_POINT('Ctrl Pts',(6.27463875524686,-19.4001766884773,84.8583531527386));
#59811=CARTESIAN_POINT('Ctrl Pts',(6.2428188528774,-19.4088188503593,84.8441968000193));
#59812=CARTESIAN_POINT('Ctrl Pts',(6.21570312034965,-19.4167674428179,84.8319688066155));
#59813=CARTESIAN_POINT('Ctrl Pts',(6.16169834482935,-19.4335244855137,84.807359990206));
#59814=CARTESIAN_POINT('Ctrl Pts',(6.05042792170448,-19.472436531396,84.7554486067052));
#59815=CARTESIAN_POINT('Ctrl Pts',(5.84476190630921,-19.5673683139041,84.653489704449));
#59816=CARTESIAN_POINT('Ctrl Pts',(5.65739800951548,-19.6930263775506,84.5515530734112));
#59817=CARTESIAN_POINT('Ctrl Pts',(5.43315068978185,-19.8873972581003,84.4219190497216));
#59818=CARTESIAN_POINT('Ctrl Pts',(5.26897645452575,-20.0769606002621,84.319589452044));
#59819=CARTESIAN_POINT('Ctrl Pts',(5.10741908303976,-20.3403380172447,84.2124573333873));
#59820=CARTESIAN_POINT('Ctrl Pts',(4.97251341135122,-20.6267209881876,84.1193109715028));
#59821=CARTESIAN_POINT('Ctrl Pts',(4.85732795150402,-21.0196848429533,84.0355138144579));
#59822=CARTESIAN_POINT('Ctrl Pts',(4.82873245991394,-21.3437858030339,84.014003760738));
#59823=CARTESIAN_POINT('Ctrl Pts',(4.82873245991394,-21.5,84.014003760738));
#59824=CARTESIAN_POINT('',(16.6267263258151,-16.3,79.6478822388519));
#59825=CARTESIAN_POINT('Ctrl Pts',(16.6267263258151,-16.3,79.6478822388519));
#59826=CARTESIAN_POINT('Ctrl Pts',(16.6267263258151,-16.1627202519724,79.6478822388519));
#59827=CARTESIAN_POINT('Ctrl Pts',(16.6179955133542,-15.9782014756465,79.6876782461328));
#59828=CARTESIAN_POINT('Ctrl Pts',(16.5950312459286,-15.8037451346603,79.7828728219127));
#59829=CARTESIAN_POINT('Ctrl Pts',(16.586544255709,-15.7515481629588,79.8170540818662));
#59830=CARTESIAN_POINT('Ctrl Pts',(16.5813766158318,-15.7228477592171,79.837607390227));
#59831=CARTESIAN_POINT('Ctrl Pts',(16.5678845354643,-15.6528601133616,79.8907518590427));
#59832=CARTESIAN_POINT('Ctrl Pts',(16.548100587601,-15.5753837738119,79.9659216531079));
#59833=CARTESIAN_POINT('Ctrl Pts',(16.5162719674538,-15.4912042488478,80.0789622080761));
#59834=CARTESIAN_POINT('Ctrl Pts',(16.4893053796703,-15.438486627179,80.1703295926858));
#59835=CARTESIAN_POINT('Ctrl Pts',(16.4643631140139,-15.4034928690422,80.2509476732841));
#59836=CARTESIAN_POINT('Ctrl Pts',(16.4458365951828,-15.3843016285567,80.3086730273532));
#59837=CARTESIAN_POINT('Ctrl Pts',(16.4363274974597,-15.3760122112162,80.3377790265208));
#59838=CARTESIAN_POINT('Ctrl Pts',(16.4308398851589,-15.371663215768,80.3544280421398));
#59839=CARTESIAN_POINT('Ctrl Pts',(16.4058754210574,-15.353224391122,80.4297068102671));
#59840=CARTESIAN_POINT('Ctrl Pts',(16.3586107169648,-15.3376504708956,80.5654454852136));
#59841=CARTESIAN_POINT('Ctrl Pts',(16.308363242307,-15.3529640814669,80.6977276874573));
#59842=CARTESIAN_POINT('Ctrl Pts',(16.2807580438145,-15.37010041347,80.7673524199429));
#59843=CARTESIAN_POINT('Ctrl Pts',(16.2775147617408,-15.3721798545712,80.7755097810832));
#59844=CARTESIAN_POINT('Ctrl Pts',(16.2734481412606,-15.3748990742495,80.7856999038481));
#59845=CARTESIAN_POINT('Ctrl Pts',(16.2685609643578,-15.3783529418162,80.7978834589029));
#59846=CARTESIAN_POINT('Ctrl Pts',(16.2620326141532,-15.3832121080572,80.8140766685934));
#59847=CARTESIAN_POINT('Ctrl Pts',(16.2554916800538,-15.388450767397,80.8301796061662));
#59848=CARTESIAN_POINT('Ctrl Pts',(16.248947338163,-15.3940656126707,80.8461713540943));
#59849=CARTESIAN_POINT('Ctrl Pts',(16.2325860018634,-15.4087182634758,80.8859576775251));
#59850=CARTESIAN_POINT('Ctrl Pts',(16.2047961808524,-15.4384721428059,80.952041722185));
#59851=CARTESIAN_POINT('Ctrl Pts',(16.1666865284266,-15.4912543308356,81.0394472234925));
#59852=CARTESIAN_POINT('Ctrl Pts',(16.1185975434662,-15.5751968380705,81.1460824099368));
#59853=CARTESIAN_POINT('Ctrl Pts',(16.0669428124562,-15.6953850753735,81.2556190750553));
#59854=CARTESIAN_POINT('Ctrl Pts',(16.0200372266792,-15.8604273231654,81.3507157648354));
#59855=CARTESIAN_POINT('Ctrl Pts',(15.9959680144551,-15.996365623908,81.3982024054527));
#59856=CARTESIAN_POINT('Ctrl Pts',(15.9859992260481,-16.0782746472634,81.4177123723923));
#59857=CARTESIAN_POINT('Ctrl Pts',(15.981559283011,-16.1252411321897,81.4263653146201));
#59858=CARTESIAN_POINT('Ctrl Pts',(15.9725425009045,-16.2435059768007,81.4438943965471));
#59859=CARTESIAN_POINT('Ctrl Pts',(15.9726062552113,-16.3565449674897,81.443748920257));
#59860=CARTESIAN_POINT('Ctrl Pts',(15.9816103595508,-16.4745965934211,81.4262469365913));
#59861=CARTESIAN_POINT('Ctrl Pts',(15.9860578245946,-16.5216040414588,81.4175766075504));
#59862=CARTESIAN_POINT('Ctrl Pts',(15.9931529411453,-16.5800659147356,81.4036970257625));
#59863=CARTESIAN_POINT('Ctrl Pts',(16.0022521358187,-16.6373793785181,81.3857696123251));
#59864=CARTESIAN_POINT('Ctrl Pts',(16.0106538593799,-16.6821981103206,81.3691011936988));
#59865=CARTESIAN_POINT('Ctrl Pts',(16.0334936810962,-16.7925239444982,81.3235736952026));
#59866=CARTESIAN_POINT('Ctrl Pts',(16.0732729417727,-16.9216470840919,81.2426097135714));
#59867=CARTESIAN_POINT('Ctrl Pts',(16.1302272700693,-17.0466007917327,81.1205411519808));
#59868=CARTESIAN_POINT('Ctrl Pts',(16.1791754703243,-17.1289822618776,81.0115059847778));
#59869=CARTESIAN_POINT('Ctrl Pts',(16.2223085872669,-17.1816622921672,80.9108472236554));
#59870=CARTESIAN_POINT('Ctrl Pts',(16.2529286652786,-17.2096866928451,80.8365863008715));
#59871=CARTESIAN_POINT('Ctrl Pts',(16.2703393347549,-17.2229799642533,80.7935103025339));
#59872=CARTESIAN_POINT('Ctrl Pts',(16.3311939963963,-17.263076777122,80.640871035239));
#59873=CARTESIAN_POINT('Ctrl Pts',(16.3879482597749,-17.2633110844262,80.4849293868592));
#59874=CARTESIAN_POINT('Ctrl Pts',(16.4430881666924,-17.2186801784522,80.3172431103551));
#59875=CARTESIAN_POINT('Ctrl Pts',(16.4642217393025,-17.1966318363056,80.251361487145));
#59876=CARTESIAN_POINT('Ctrl Pts',(16.4991469954625,-17.1481299251104,80.1385791791468));
#59877=CARTESIAN_POINT('Ctrl Pts',(16.5417979890631,-17.0491114348861,79.9898247024023));
#59878=CARTESIAN_POINT('Ctrl Pts',(16.5787193153288,-16.9047265894586,79.8495489824192));
#59879=CARTESIAN_POINT('Ctrl Pts',(16.6070569699324,-16.7195440420054,79.7337450825527));
#59880=CARTESIAN_POINT('Ctrl Pts',(16.6232895344097,-16.5114662207145,79.6631181782204));
#59881=CARTESIAN_POINT('Ctrl Pts',(16.6267263258151,-16.3686398740138,79.647882238852));
#59882=CARTESIAN_POINT('Ctrl Pts',(16.6267263258151,-16.3,79.647882238852));
#59883=CARTESIAN_POINT('Origin',(9.31513030214989,-21.5,77.9859046106882));
#59884=CARTESIAN_POINT('',(5.00120579598144,-21.5,83.9614679362901));
#59885=CARTESIAN_POINT('',(7.42634813437021,-21.5,77.2984441226036));
#59886=CARTESIAN_POINT('Ctrl Pts',(5.00120579598144,-21.5,83.9614679362901));
#59887=CARTESIAN_POINT('Ctrl Pts',(5.00120579598144,-21.3520059990089,83.9614679362901));
#59888=CARTESIAN_POINT('Ctrl Pts',(5.02938710354273,-21.0449379529334,83.9815481249973));
#59889=CARTESIAN_POINT('Ctrl Pts',(5.14210001521926,-20.6745440882475,84.0595031650574));
#59890=CARTESIAN_POINT('Ctrl Pts',(5.27274890176333,-20.4064934480325,84.1457116731447));
#59891=CARTESIAN_POINT('Ctrl Pts',(5.42805833516398,-20.1613379356766,84.2445019203697));
#59892=CARTESIAN_POINT('Ctrl Pts',(5.5842076611768,-19.9865699045241,84.3383374923964));
#59893=CARTESIAN_POINT('Ctrl Pts',(5.79518871998536,-19.8086662168602,84.4566186593402));
#59894=CARTESIAN_POINT('Ctrl Pts',(5.97008028592641,-19.6944825986058,84.5492829143672));
#59895=CARTESIAN_POINT('Ctrl Pts',(6.16024874649474,-19.6088242840925,84.6416704339889));
#59896=CARTESIAN_POINT('Ctrl Pts',(6.26265561097925,-19.5738308190456,84.6886756114093));
#59897=CARTESIAN_POINT('Ctrl Pts',(6.31228285326648,-19.5587773020503,84.7109583986528));
#59898=CARTESIAN_POINT('Ctrl Pts',(6.33718439395397,-19.5516405475664,84.7220307194513));
#59899=CARTESIAN_POINT('Ctrl Pts',(6.36638310919858,-19.5438854025941,84.7348502432122));
#59900=CARTESIAN_POINT('Ctrl Pts',(6.46664380786896,-19.5188490700099,84.7784451622438));
#59901=CARTESIAN_POINT('Ctrl Pts',(6.61214355835411,-19.4956974788605,84.8381010128625));
#59902=CARTESIAN_POINT('Ctrl Pts',(6.87934184713117,-19.4843021730789,84.9386886521805));
#59903=CARTESIAN_POINT('Ctrl Pts',(7.08098376058415,-19.5065990278365,85.0055173198125));
#59904=CARTESIAN_POINT('Ctrl Pts',(7.23572536065315,-19.5438603297829,85.0512669854069));
#59905=CARTESIAN_POINT('Ctrl Pts',(7.25902594561429,-19.5497685575946,85.0580779380141));
#59906=CARTESIAN_POINT('Ctrl Pts',(7.29398062082609,-19.5589776728157,85.068202640782));
#59907=CARTESIAN_POINT('Ctrl Pts',(7.37249143930395,-19.5818620333112,85.0903671757502));
#59908=CARTESIAN_POINT('Ctrl Pts',(7.47629543310783,-19.6184900161799,85.1180421488052));
#59909=CARTESIAN_POINT('Ctrl Pts',(7.61240028365782,-19.6768804536723,85.1519024555482));
#59910=CARTESIAN_POINT('Ctrl Pts',(7.7884588882969,-19.7679209606644,85.1922855511176));
#59911=CARTESIAN_POINT('Ctrl Pts',(8.00571902094384,-19.9161198082099,85.2354092037281));
#59912=CARTESIAN_POINT('Ctrl Pts',(8.20165416446568,-20.0945202553182,85.2681402867983));
#59913=CARTESIAN_POINT('Ctrl Pts',(8.33072651652134,-20.2441651242008,85.2867918154456));
#59914=CARTESIAN_POINT('Ctrl Pts',(8.45148795656648,-20.4072154069382,85.3028209480783));
#59915=CARTESIAN_POINT('Ctrl Pts',(8.57200758743931,-20.6057239697199,85.3169691524854));
#59916=CARTESIAN_POINT('Ctrl Pts',(8.69159825227611,-20.8958285905613,85.3288534467772));
#59917=CARTESIAN_POINT('Ctrl Pts',(8.75757356805284,-21.1735479434414,85.3346262878536));
#59918=CARTESIAN_POINT('Ctrl Pts',(8.77688460061852,-21.3763469753939,85.336233820364));
#59919=CARTESIAN_POINT('Ctrl Pts',(8.78059087654672,-21.5738186910076,85.3365468413902));
#59920=CARTESIAN_POINT('Ctrl Pts',(8.75630061671194,-21.9017339681359,85.334517176155));
#59921=CARTESIAN_POINT('Ctrl Pts',(8.65051985500575,-22.2305671395078,85.3253318026369));
#59922=CARTESIAN_POINT('Ctrl Pts',(8.50506066967912,-22.5045527127309,85.3091069381655));
#59923=CARTESIAN_POINT('Ctrl Pts',(8.39473328732379,-22.6791889660986,85.2957679284494));
#59924=CARTESIAN_POINT('Ctrl Pts',(8.21907518119456,-22.8898206522999,85.2710792257392));
#59925=CARTESIAN_POINT('Ctrl Pts',(8.00586508617554,-23.0837282560587,85.2354108414265));
#59926=CARTESIAN_POINT('Ctrl Pts',(7.71630377271468,-23.2813748438679,85.1780083266107));
#59927=CARTESIAN_POINT('Ctrl Pts',(7.44278857103648,-23.4008177940264,85.1110366251592));
#59928=CARTESIAN_POINT('Ctrl Pts',(7.16292149566871,-23.476956232333,85.0306247350017));
#59929=CARTESIAN_POINT('Ctrl Pts',(6.92920042935146,-23.5117274127833,84.9556727639564));
#59930=CARTESIAN_POINT('Ctrl Pts',(6.64052521451068,-23.5121075528597,84.8507009698725));
#59931=CARTESIAN_POINT('Ctrl Pts',(6.36728513118301,-23.4641122791779,84.7373259615023));
#59932=CARTESIAN_POINT('Ctrl Pts',(6.01870899323939,-23.3415395005,84.5762647242888));
#59933=CARTESIAN_POINT('Ctrl Pts',(5.68113207878283,-23.1237730049189,84.396893955329));
#59934=CARTESIAN_POINT('Ctrl Pts',(5.45052492150888,-22.8633215721594,84.2579345062791));
#59935=CARTESIAN_POINT('Ctrl Pts',(5.29094963212753,-22.6259977123551,84.1575892563859));
#59936=CARTESIAN_POINT('Ctrl Pts',(5.15335516091919,-22.362344512459,84.0672755210376));
#59937=CARTESIAN_POINT('Ctrl Pts',(5.02942559621785,-21.9550903286244,83.9815767221747));
#59938=CARTESIAN_POINT('Ctrl Pts',(5.00120579598144,-21.6479940009911,83.9614679362901));
#59939=CARTESIAN_POINT('Ctrl Pts',(5.00120579598144,-21.5,83.9614679362901));
#59940=CARTESIAN_POINT('',(8.46456668098594,-23.4399831912377,78.7854630291158));
#59941=CARTESIAN_POINT('',(9.16725530571964,-23.439990633261,76.8549480800671));
#59942=CARTESIAN_POINT('',(8.82100921955859,-23.44,77.8060592445016));
#59943=CARTESIAN_POINT('',(10.1553645548646,-23.43992588449,77.2145815988743));
#59944=CARTESIAN_POINT('Ctrl Pts',(10.1553531683805,-23.4399183977911,77.2145896236657));
#59945=CARTESIAN_POINT('Ctrl Pts',(10.0879810015635,-23.4637967282797,77.1412715498725));
#59946=CARTESIAN_POINT('Ctrl Pts',(9.9717328772446,-23.4927472120551,77.0438930991871));
#59947=CARTESIAN_POINT('Ctrl Pts',(9.76844966013923,-23.5119591404095,76.9341462709327));
#59948=CARTESIAN_POINT('Ctrl Pts',(9.58984999260555,-23.5101434522743,76.872532168987));
#59949=CARTESIAN_POINT('Ctrl Pts',(9.3788902833647,-23.4855876966743,76.8415124408269));
#59950=CARTESIAN_POINT('Ctrl Pts',(9.2427353924026,-23.4580865891214,76.8456230088964));
#59951=CARTESIAN_POINT('Ctrl Pts',(9.17328487982263,-23.4414541894188,76.854157385364));
#59952=CARTESIAN_POINT('Ctrl Pts',(9.16725530571964,-23.439990633261,76.8549480800671));
#59953=CARTESIAN_POINT('',(9.45274488900745,-23.4399725752062,79.1450870611007));
#59954=CARTESIAN_POINT('',(9.80925138474118,-23.44,78.1657499768748));
#59955=CARTESIAN_POINT('Ctrl Pts',(8.46456668098594,-23.4399831912377,78.7854630291158));
#59956=CARTESIAN_POINT('Ctrl Pts',(8.48862373486699,-23.4485471463589,78.8117034392736));
#59957=CARTESIAN_POINT('Ctrl Pts',(8.55980178672779,-23.4709295638718,78.8823074031271));
#59958=CARTESIAN_POINT('Ctrl Pts',(8.69364486134355,-23.4983842652002,78.9832904164185));
#59959=CARTESIAN_POINT('Ctrl Pts',(8.86630044007771,-23.5123967187664,79.0720196330274));
#59960=CARTESIAN_POINT('Ctrl Pts',(9.04620851329942,-23.5082837204292,79.1299209668847));
#59961=CARTESIAN_POINT('Ctrl Pts',(9.24114419357868,-23.4856018928221,79.1585650126785));
#59962=CARTESIAN_POINT('Ctrl Pts',(9.3772214843187,-23.4580769550451,79.1543912360021));
#59963=CARTESIAN_POINT('Ctrl Pts',(9.44668059476406,-23.4414315376984,79.1458387644055));
#59964=CARTESIAN_POINT('Ctrl Pts',(9.45273622862353,-23.4399606993813,79.1450431018916));
#59965=CARTESIAN_POINT('Ctrl Pts',(4.82873245991394,-21.5,84.014003760738));
#59966=CARTESIAN_POINT('Ctrl Pts',(4.82873245991394,-21.3437858030339,84.014003760738));
#59967=CARTESIAN_POINT('Ctrl Pts',(4.85732795150402,-21.0196848429533,84.0355138144579));
#59968=CARTESIAN_POINT('Ctrl Pts',(4.97251341135122,-20.6267209881876,84.1193109715028));
#59969=CARTESIAN_POINT('Ctrl Pts',(5.10741908303976,-20.3403380172447,84.2124573333873));
#59970=CARTESIAN_POINT('Ctrl Pts',(5.26897645452575,-20.0769606002621,84.319589452044));
#59971=CARTESIAN_POINT('Ctrl Pts',(5.43315068978185,-19.8873972581003,84.4219190497216));
#59972=CARTESIAN_POINT('Ctrl Pts',(5.65739800951548,-19.6930263775506,84.5515530734112));
#59973=CARTESIAN_POINT('Ctrl Pts',(5.84476190630921,-19.5673683139041,84.653489704449));
#59974=CARTESIAN_POINT('Ctrl Pts',(6.05042792170448,-19.472436531396,84.7554486067052));
#59975=CARTESIAN_POINT('Ctrl Pts',(6.16169834482935,-19.4335244855137,84.807359990206));
#59976=CARTESIAN_POINT('Ctrl Pts',(6.21570312034965,-19.4167674428179,84.8319688066155));
#59977=CARTESIAN_POINT('Ctrl Pts',(6.2428188528774,-19.4088188503593,84.8441968000193));
#59978=CARTESIAN_POINT('Ctrl Pts',(6.27463875524686,-19.4001766884773,84.8583531527386));
#59979=CARTESIAN_POINT('Ctrl Pts',(6.38396293084926,-19.3722629250898,84.9064904925777));
#59980=CARTESIAN_POINT('Ctrl Pts',(6.54311667666213,-19.3463797210142,84.9723056198425));
#59981=CARTESIAN_POINT('Ctrl Pts',(6.83602917970007,-19.3336186512925,85.0828499150213));
#59982=CARTESIAN_POINT('Ctrl Pts',(7.05731504363103,-19.3586067795117,85.1556486945886));
#59983=CARTESIAN_POINT('Ctrl Pts',(7.2266071958566,-19.4001505834634,85.2048434726207));
#59984=CARTESIAN_POINT('Ctrl Pts',(7.25209035941627,-19.406734446681,85.2121572627922));
#59985=CARTESIAN_POINT('Ctrl Pts',(7.29030926384011,-19.4169940333725,85.2230170810003));
#59986=CARTESIAN_POINT('Ctrl Pts',(7.37608465013576,-19.4424658819364,85.2467130241579));
#59987=CARTESIAN_POINT('Ctrl Pts',(7.48927323429437,-19.4831548365047,85.2760681754352));
#59988=CARTESIAN_POINT('Ctrl Pts',(7.63726184737735,-19.5478095215932,85.3116066824435));
#59989=CARTESIAN_POINT('Ctrl Pts',(7.82802168890365,-19.6482675713107,85.3534138355257));
#59990=CARTESIAN_POINT('Ctrl Pts',(8.06181738257177,-19.8106817132535,85.3968159991057));
#59991=CARTESIAN_POINT('Ctrl Pts',(8.27089129566994,-20.0045077474062,85.4284509108725));
#59992=CARTESIAN_POINT('Ctrl Pts',(8.40767692089607,-20.1659139729294,85.4457557150761));
#59993=CARTESIAN_POINT('Ctrl Pts',(8.53517073786835,-20.3410662633443,85.4602233453799));
#59994=CARTESIAN_POINT('Ctrl Pts',(8.6617617762221,-20.5533339316959,85.4724237592255));
#59995=CARTESIAN_POINT('Ctrl Pts',(8.78657759480108,-20.8615791622571,85.4819283317405));
#59996=CARTESIAN_POINT('Ctrl Pts',(8.85513326762087,-21.1553648060587,85.48622725368));
#59997=CARTESIAN_POINT('Ctrl Pts',(8.87516743536897,-21.3694798611557,85.4873864938745));
#59998=CARTESIAN_POINT('Ctrl Pts',(8.87901361505321,-21.5779256266326,85.487614474219));
#59999=CARTESIAN_POINT('Ctrl Pts',(8.85381443839301,-21.9240224696184,85.4861466895026));
#60000=CARTESIAN_POINT('Ctrl Pts',(8.74391346127118,-22.272332044321,85.4793401936152));
#60001=CARTESIAN_POINT('Ctrl Pts',(8.59144124522549,-22.5645860879582,85.4656428345252));
#60002=CARTESIAN_POINT('Ctrl Pts',(8.47541979746267,-22.7514824404779,85.4540052246341));
#60003=CARTESIAN_POINT('Ctrl Pts',(8.28948884338796,-22.9784739218892,85.4312988805198));
#60004=CARTESIAN_POINT('Ctrl Pts',(8.06196599656662,-23.1891502055613,85.3968111581528));
#60005=CARTESIAN_POINT('Ctrl Pts',(7.75038779391833,-23.4057620043471,85.3390556557566));
#60006=CARTESIAN_POINT('Ctrl Pts',(7.45300707834779,-23.5382170209426,85.2689305062561));
#60007=CARTESIAN_POINT('Ctrl Pts',(7.14703055733959,-23.6230346405478,85.1827564818876));
#60008=CARTESIAN_POINT('Ctrl Pts',(6.89079758792843,-23.6619346851716,85.1014126433423));
#60009=CARTESIAN_POINT('Ctrl Pts',(6.57408560510447,-23.662351077972,84.9862512166584));
#60010=CARTESIAN_POINT('Ctrl Pts',(6.2753117530903,-23.6086799844817,84.8611083880992));
#60011=CARTESIAN_POINT('Ctrl Pts',(5.89665156355806,-23.4723187384843,84.6831785101655));
#60012=CARTESIAN_POINT('Ctrl Pts',(5.53493133383187,-23.2322336732833,84.4857324948551));
#60013=CARTESIAN_POINT('Ctrl Pts',(5.2926198619563,-22.9497986695551,84.3342442319345));
#60014=CARTESIAN_POINT('Ctrl Pts',(5.12625478749138,-22.6944732941622,84.2253058354118));
#60015=CARTESIAN_POINT('Ctrl Pts',(4.98401828163431,-22.4124109055271,84.1276650488678));
#60016=CARTESIAN_POINT('Ctrl Pts',(4.85736622748711,-21.9803502519472,84.0355447824565));
#60017=CARTESIAN_POINT('Ctrl Pts',(4.82873245991394,-21.6562141969661,84.014003760738));
#60018=CARTESIAN_POINT('Ctrl Pts',(4.82873245991394,-21.5,84.014003760738));
#60019=CARTESIAN_POINT('Ctrl Pts',(4.88622357193644,-21.5,83.9964918192554));
#60020=CARTESIAN_POINT('Ctrl Pts',(4.88622357193644,-21.3465258683589,83.9964918192554));
#60021=CARTESIAN_POINT('Ctrl Pts',(4.91468100218359,-21.02810254628,84.0175252513044));
#60022=CARTESIAN_POINT('Ctrl Pts',(5.02904227930723,-20.6426620215409,84.099375036021));
#60023=CARTESIAN_POINT('Ctrl Pts',(5.16252902261428,-20.3623898275073,84.1902087799731));
#60024=CARTESIAN_POINT('Ctrl Pts',(5.32200374807183,-20.1050863787336,84.2945602748192));
#60025=CARTESIAN_POINT('Ctrl Pts',(5.48350301358017,-19.9204548069083,84.3940585306133));
#60026=CARTESIAN_POINT('Ctrl Pts',(5.70332824633877,-19.7315729906538,84.5199082687209));
#60027=CARTESIAN_POINT('Ctrl Pts',(5.88653469951494,-19.609739742138,84.6187541077551));
#60028=CARTESIAN_POINT('Ctrl Pts',(6.08703486330123,-19.5178991156282,84.7175225491331));
#60029=CARTESIAN_POINT('Ctrl Pts',(6.19535076687932,-19.4802932633577,84.7677985306071));
#60030=CARTESIAN_POINT('Ctrl Pts',(6.24789636465526,-19.464104062562,84.7916320039613));
#60031=CARTESIAN_POINT('Ctrl Pts',(6.27427403323625,-19.4564260827617,84.8034747731633));
#60032=CARTESIAN_POINT('Ctrl Pts',(6.3052202065641,-19.4480795931829,84.8171855162298));
#60033=CARTESIAN_POINT('Ctrl Pts',(6.41152322318916,-19.4211249733965,84.8638087157997));
#60034=CARTESIAN_POINT('Ctrl Pts',(6.56612563722612,-19.396152306963,84.9275707508492));
#60035=CARTESIAN_POINT('Ctrl Pts',(6.85046673551044,-19.383846491888,85.034796160741));
#60036=CARTESIAN_POINT('Ctrl Pts',(7.06520461594874,-19.4079375289533,85.1056049029966));
#60037=CARTESIAN_POINT('Ctrl Pts',(7.22964658412212,-19.4480538322366,85.1536513102161));
#60038=CARTESIAN_POINT('Ctrl Pts',(7.25440222148228,-19.4544124836522,85.1607974878662));
#60039=CARTESIAN_POINT('Ctrl Pts',(7.29153304950211,-19.4643219131869,85.1714122675942));
#60040=CARTESIAN_POINT('Ctrl Pts',(7.37488691319182,-19.488931265728,85.1945977413554));
#60041=CARTESIAN_POINT('Ctrl Pts',(7.48494730056552,-19.5282665630631,85.2233928332252));
#60042=CARTESIAN_POINT('Ctrl Pts',(7.62897465947084,-19.5908331656196,85.258371940145));
#60043=CARTESIAN_POINT('Ctrl Pts',(7.8148340887014,-19.6881520344286,85.2997044073897));
#60044=CARTESIAN_POINT('Ctrl Pts',(8.04311792869579,-19.8458277449056,85.3430137339799));
#60045=CARTESIAN_POINT('Ctrl Pts',(8.24781225193518,-20.0345119167102,85.3750140361811));
#60046=CARTESIAN_POINT('Ctrl Pts',(8.38202678610449,-20.1919976900199,85.3927677485326));
#60047=CARTESIAN_POINT('Ctrl Pts',(8.50727647743439,-20.3631159778756,85.4077558796127));
#60048=CARTESIAN_POINT('Ctrl Pts',(8.6318437132945,-20.5707972777039,85.4206055569788));
#60049=CARTESIAN_POINT('Ctrl Pts',(8.75491781395942,-20.8729956383585,85.4309033700861));
#60050=CARTESIAN_POINT('Ctrl Pts',(8.82261336776486,-21.161425851853,85.4356935984045));
#60051=CARTESIAN_POINT('Ctrl Pts',(8.84240649045215,-21.3717688992351,85.437002269371));
#60052=CARTESIAN_POINT('Ctrl Pts',(8.84620603555104,-21.5765566480909,85.4372585966094));
#60053=CARTESIAN_POINT('Ctrl Pts',(8.82130983116599,-21.9165929691243,85.4356035183868));
#60054=CARTESIAN_POINT('Ctrl Pts',(8.7127822591827,-22.2584104093833,85.4280040632891));
#60055=CARTESIAN_POINT('Ctrl Pts',(8.56264772004336,-22.5445749628824,85.4134642024053));
#60056=CARTESIAN_POINT('Ctrl Pts',(8.44852429408304,-22.7273846156848,85.4012594592392));
#60057=CARTESIAN_POINT('Ctrl Pts',(8.26601762265683,-22.9489228320261,85.3778923289262));
#60058=CARTESIAN_POINT('Ctrl Pts',(8.04326569310293,-23.1540095557271,85.3430110525773));
#60059=CARTESIAN_POINT('Ctrl Pts',(7.73902645351712,-23.3642996175207,85.285373212708));
#60060=CARTESIAN_POINT('Ctrl Pts',(7.44960090924402,-23.4924172786372,85.2162992125571));
#60061=CARTESIAN_POINT('Ctrl Pts',(7.15232753678263,-23.5743418378095,85.1320458995923));
#60062=CARTESIAN_POINT('Ctrl Pts',(6.90359853506944,-23.6118655943755,85.052832683547));
#60063=CARTESIAN_POINT('Ctrl Pts',(6.59623214157321,-23.6122699029346,84.9410678010631));
#60064=CARTESIAN_POINT('Ctrl Pts',(6.30596954578787,-23.5604907493805,84.8198475792336));
#60065=CARTESIAN_POINT('Ctrl Pts',(5.93733737345184,-23.4287256591562,84.6475405815399));
#60066=CARTESIAN_POINT('Ctrl Pts',(5.58366491548219,-23.1960801171618,84.4561196483464));
#60067=CARTESIAN_POINT('Ctrl Pts',(5.34525488180716,-22.9209729704232,84.308807656716));
#60068=CARTESIAN_POINT('Ctrl Pts',(5.18115306903677,-22.6716481002265,84.2027336424032));
#60069=CARTESIAN_POINT('Ctrl Pts',(5.0404639080626,-22.3957221078377,84.1075352062577));
#60070=CARTESIAN_POINT('Ctrl Pts',(4.91471935039736,-21.9719302775063,84.0175554290292));
#60071=CARTESIAN_POINT('Ctrl Pts',(4.88622357193644,-21.6534741316411,83.9964918192554));
#60072=CARTESIAN_POINT('Ctrl Pts',(4.88622357193644,-21.5,83.9964918192554));
#60073=CARTESIAN_POINT('Ctrl Pts',(4.94371468395894,-21.5,83.9789798777728));
#60074=CARTESIAN_POINT('Ctrl Pts',(4.94371468395894,-21.3492659336839,83.9789798777728));
#60075=CARTESIAN_POINT('Ctrl Pts',(4.97203405286316,-21.0365202496067,83.9995366881508));
#60076=CARTESIAN_POINT('Ctrl Pts',(5.08557114726325,-20.6586030548942,84.0794391005392));
#60077=CARTESIAN_POINT('Ctrl Pts',(5.2176389621888,-20.3844416377699,84.1679602265589));
#60078=CARTESIAN_POINT('Ctrl Pts',(5.3750310416179,-20.1332121572051,84.2695310975945));
#60079=CARTESIAN_POINT('Ctrl Pts',(5.53385533737848,-19.9535123557162,84.3661980115048));
#60080=CARTESIAN_POINT('Ctrl Pts',(5.74925848316206,-19.770119603757,84.4882634640305));
#60081=CARTESIAN_POINT('Ctrl Pts',(5.92830749272068,-19.6521111703719,84.5840185110611));
#60082=CARTESIAN_POINT('Ctrl Pts',(6.12364180489798,-19.5633616998603,84.6795964915611));
#60083=CARTESIAN_POINT('Ctrl Pts',(6.22900318892928,-19.5270620412017,84.7282370710082));
#60084=CARTESIAN_POINT('Ctrl Pts',(6.28008960896087,-19.5114406823062,84.7512952013071));
#60085=CARTESIAN_POINT('Ctrl Pts',(6.30572921359511,-19.5040333151641,84.7627527463073));
#60086=CARTESIAN_POINT('Ctrl Pts',(6.33580165788134,-19.4959824978885,84.776017879721));
#60087=CARTESIAN_POINT('Ctrl Pts',(6.43908351552906,-19.4699870217032,84.8211269390218));
#60088=CARTESIAN_POINT('Ctrl Pts',(6.58913459779012,-19.4459248929117,84.8828358818558));
#60089=CARTESIAN_POINT('Ctrl Pts',(6.8649042913208,-19.4340743324834,84.9867424064607));
#60090=CARTESIAN_POINT('Ctrl Pts',(7.07309418826644,-19.4572682783949,85.0555611114046));
#60091=CARTESIAN_POINT('Ctrl Pts',(7.23268597238763,-19.4959570810097,85.1024591478115));
#60092=CARTESIAN_POINT('Ctrl Pts',(7.25671408354828,-19.5020905206234,85.1094377129401));
#60093=CARTESIAN_POINT('Ctrl Pts',(7.2927568351641,-19.5116497930013,85.1198074541881));
#60094=CARTESIAN_POINT('Ctrl Pts',(7.37368917624788,-19.5353966495196,85.1424824585528));
#60095=CARTESIAN_POINT('Ctrl Pts',(7.48062136683667,-19.5733782896215,85.1707174910152));
#60096=CARTESIAN_POINT('Ctrl Pts',(7.62068747156432,-19.6338568096459,85.2051371978466));
#60097=CARTESIAN_POINT('Ctrl Pts',(7.80164648849915,-19.7280364975465,85.2459949792536));
#60098=CARTESIAN_POINT('Ctrl Pts',(8.02441847481981,-19.8809737765578,85.289211468854));
#60099=CARTESIAN_POINT('Ctrl Pts',(8.22473320820043,-20.0645160860142,85.3215771614897));
#60100=CARTESIAN_POINT('Ctrl Pts',(8.35637665131292,-20.2180814071103,85.3397797819891));
#60101=CARTESIAN_POINT('Ctrl Pts',(8.47938221700044,-20.3851656924069,85.3552884138455));
#60102=CARTESIAN_POINT('Ctrl Pts',(8.60192565036691,-20.5882606237119,85.3687873547321));
#60103=CARTESIAN_POINT('Ctrl Pts',(8.72325803311777,-20.8844121144599,85.3798784084316));
#60104=CARTESIAN_POINT('Ctrl Pts',(8.79009346790885,-21.1674868976472,85.385159943129));
#60105=CARTESIAN_POINT('Ctrl Pts',(8.80964554553534,-21.3740579373145,85.3866180448675));
#60106=CARTESIAN_POINT('Ctrl Pts',(8.81339845604888,-21.5751876695492,85.3869027189998));
#60107=CARTESIAN_POINT('Ctrl Pts',(8.78880522393897,-21.9091634686301,85.3850603472709));
#60108=CARTESIAN_POINT('Ctrl Pts',(8.68165105709423,-22.2444887744455,85.376667932963));
#60109=CARTESIAN_POINT('Ctrl Pts',(8.53385419486124,-22.5245638378067,85.3612855702854));
#60110=CARTESIAN_POINT('Ctrl Pts',(8.42162879070342,-22.7032867908917,85.3485136938443));
#60111=CARTESIAN_POINT('Ctrl Pts',(8.2425464019257,-22.919371742163,85.3244857773327));
#60112=CARTESIAN_POINT('Ctrl Pts',(8.02456538963924,-23.1188689058929,85.2892109470019));
#60113=CARTESIAN_POINT('Ctrl Pts',(7.7276651131159,-23.3228372306943,85.2316907696594));
#60114=CARTESIAN_POINT('Ctrl Pts',(7.44619474014025,-23.4466175363318,85.1636679188582));
#60115=CARTESIAN_POINT('Ctrl Pts',(7.15762451622567,-23.5256490350712,85.081335317297));
#60116=CARTESIAN_POINT('Ctrl Pts',(6.91639948221045,-23.5617965035794,85.0042527237517));
#60117=CARTESIAN_POINT('Ctrl Pts',(6.61837867804194,-23.5621887278972,84.8958843854678));
#60118=CARTESIAN_POINT('Ctrl Pts',(6.33662733848544,-23.5123015142792,84.7785867703679));
#60119=CARTESIAN_POINT('Ctrl Pts',(5.97802318334561,-23.3851325798281,84.6119026529143));
#60120=CARTESIAN_POINT('Ctrl Pts',(5.63239849713251,-23.1599265610404,84.4265068018377));
#60121=CARTESIAN_POINT('Ctrl Pts',(5.39788990165802,-22.8921472712913,84.2833710814976));
#60122=CARTESIAN_POINT('Ctrl Pts',(5.23605135058215,-22.6488229062908,84.1801614493946));
#60123=CARTESIAN_POINT('Ctrl Pts',(5.0969095344909,-22.3790333101484,84.0874053636477));
#60124=CARTESIAN_POINT('Ctrl Pts',(4.9720724733076,-21.9635103030653,83.999566075602));
#60125=CARTESIAN_POINT('Ctrl Pts',(4.94371468395894,-21.6507340663161,83.9789798777728));
#60126=CARTESIAN_POINT('Ctrl Pts',(4.94371468395894,-21.5,83.9789798777728));
#60127=CARTESIAN_POINT('Ctrl Pts',(5.00120579598144,-21.5,83.9614679362901));
#60128=CARTESIAN_POINT('Ctrl Pts',(5.00120579598144,-21.3520059990089,83.9614679362901));
#60129=CARTESIAN_POINT('Ctrl Pts',(5.02938710354273,-21.0449379529334,83.9815481249973));
#60130=CARTESIAN_POINT('Ctrl Pts',(5.14210001521926,-20.6745440882475,84.0595031650574));
#60131=CARTESIAN_POINT('Ctrl Pts',(5.27274890176333,-20.4064934480325,84.1457116731447));
#60132=CARTESIAN_POINT('Ctrl Pts',(5.42805833516398,-20.1613379356766,84.2445019203697));
#60133=CARTESIAN_POINT('Ctrl Pts',(5.5842076611768,-19.9865699045241,84.3383374923964));
#60134=CARTESIAN_POINT('Ctrl Pts',(5.79518871998536,-19.8086662168602,84.4566186593402));
#60135=CARTESIAN_POINT('Ctrl Pts',(5.97008028592641,-19.6944825986058,84.5492829143672));
#60136=CARTESIAN_POINT('Ctrl Pts',(6.16024874649474,-19.6088242840925,84.6416704339889));
#60137=CARTESIAN_POINT('Ctrl Pts',(6.26265561097925,-19.5738308190456,84.6886756114093));
#60138=CARTESIAN_POINT('Ctrl Pts',(6.31228285326648,-19.5587773020503,84.7109583986528));
#60139=CARTESIAN_POINT('Ctrl Pts',(6.33718439395397,-19.5516405475664,84.7220307194513));
#60140=CARTESIAN_POINT('Ctrl Pts',(6.36638310919858,-19.5438854025941,84.7348502432122));
#60141=CARTESIAN_POINT('Ctrl Pts',(6.46664380786896,-19.5188490700099,84.7784451622438));
#60142=CARTESIAN_POINT('Ctrl Pts',(6.61214355835411,-19.4956974788605,84.8381010128625));
#60143=CARTESIAN_POINT('Ctrl Pts',(6.87934184713117,-19.4843021730789,84.9386886521805));
#60144=CARTESIAN_POINT('Ctrl Pts',(7.08098376058415,-19.5065990278365,85.0055173198125));
#60145=CARTESIAN_POINT('Ctrl Pts',(7.23572536065315,-19.5438603297829,85.0512669854069));
#60146=CARTESIAN_POINT('Ctrl Pts',(7.25902594561429,-19.5497685575946,85.0580779380141));
#60147=CARTESIAN_POINT('Ctrl Pts',(7.29398062082609,-19.5589776728157,85.068202640782));
#60148=CARTESIAN_POINT('Ctrl Pts',(7.37249143930395,-19.5818620333112,85.0903671757502));
#60149=CARTESIAN_POINT('Ctrl Pts',(7.47629543310783,-19.6184900161799,85.1180421488052));
#60150=CARTESIAN_POINT('Ctrl Pts',(7.61240028365782,-19.6768804536723,85.1519024555482));
#60151=CARTESIAN_POINT('Ctrl Pts',(7.7884588882969,-19.7679209606644,85.1922855511176));
#60152=CARTESIAN_POINT('Ctrl Pts',(8.00571902094384,-19.9161198082099,85.2354092037281));
#60153=CARTESIAN_POINT('Ctrl Pts',(8.20165416446568,-20.0945202553182,85.2681402867983));
#60154=CARTESIAN_POINT('Ctrl Pts',(8.33072651652134,-20.2441651242008,85.2867918154456));
#60155=CARTESIAN_POINT('Ctrl Pts',(8.45148795656648,-20.4072154069382,85.3028209480783));
#60156=CARTESIAN_POINT('Ctrl Pts',(8.57200758743931,-20.6057239697199,85.3169691524854));
#60157=CARTESIAN_POINT('Ctrl Pts',(8.69159825227611,-20.8958285905613,85.3288534467772));
#60158=CARTESIAN_POINT('Ctrl Pts',(8.75757356805284,-21.1735479434414,85.3346262878536));
#60159=CARTESIAN_POINT('Ctrl Pts',(8.77688460061852,-21.3763469753939,85.336233820364));
#60160=CARTESIAN_POINT('Ctrl Pts',(8.78059087654672,-21.5738186910076,85.3365468413902));
#60161=CARTESIAN_POINT('Ctrl Pts',(8.75630061671194,-21.9017339681359,85.334517176155));
#60162=CARTESIAN_POINT('Ctrl Pts',(8.65051985500575,-22.2305671395078,85.3253318026369));
#60163=CARTESIAN_POINT('Ctrl Pts',(8.50506066967912,-22.5045527127309,85.3091069381655));
#60164=CARTESIAN_POINT('Ctrl Pts',(8.39473328732379,-22.6791889660986,85.2957679284494));
#60165=CARTESIAN_POINT('Ctrl Pts',(8.21907518119456,-22.8898206522999,85.2710792257392));
#60166=CARTESIAN_POINT('Ctrl Pts',(8.00586508617554,-23.0837282560587,85.2354108414265));
#60167=CARTESIAN_POINT('Ctrl Pts',(7.71630377271468,-23.2813748438679,85.1780083266107));
#60168=CARTESIAN_POINT('Ctrl Pts',(7.44278857103648,-23.4008177940264,85.1110366251592));
#60169=CARTESIAN_POINT('Ctrl Pts',(7.16292149566871,-23.476956232333,85.0306247350017));
#60170=CARTESIAN_POINT('Ctrl Pts',(6.92920042935146,-23.5117274127833,84.9556727639564));
#60171=CARTESIAN_POINT('Ctrl Pts',(6.64052521451068,-23.5121075528597,84.8507009698725));
#60172=CARTESIAN_POINT('Ctrl Pts',(6.36728513118301,-23.4641122791779,84.7373259615023));
#60173=CARTESIAN_POINT('Ctrl Pts',(6.01870899323939,-23.3415395005,84.5762647242888));
#60174=CARTESIAN_POINT('Ctrl Pts',(5.68113207878283,-23.1237730049189,84.396893955329));
#60175=CARTESIAN_POINT('Ctrl Pts',(5.45052492150888,-22.8633215721594,84.2579345062791));
#60176=CARTESIAN_POINT('Ctrl Pts',(5.29094963212753,-22.6259977123551,84.1575892563859));
#60177=CARTESIAN_POINT('Ctrl Pts',(5.15335516091919,-22.362344512459,84.0672755210376));
#60178=CARTESIAN_POINT('Ctrl Pts',(5.02942559621785,-21.9550903286244,83.9815767221747));
#60179=CARTESIAN_POINT('Ctrl Pts',(5.00120579598144,-21.6479940009911,83.9614679362901));
#60180=CARTESIAN_POINT('Ctrl Pts',(5.00120579598144,-21.5,83.9614679362901));
#60181=CARTESIAN_POINT('',(4.82873245991394,-21.5,84.014003760738));
#60182=CARTESIAN_POINT('Origin',(9.31,-25.425,78.));
#60183=CARTESIAN_POINT('',(8.155,-25.5,78.));
#60184=CARTESIAN_POINT('Origin',(9.31,-25.5,78.));
#60185=CARTESIAN_POINT('',(8.305,-25.35,78.));
#60186=CARTESIAN_POINT('',(8.23,-25.425,78.));
#60187=CARTESIAN_POINT('Origin',(9.31,-25.35,78.));
#60188=CARTESIAN_POINT('Origin',(9.31,-24.485,78.));
#60189=CARTESIAN_POINT('',(10.0375846303818,-23.44,78.6932860921958));
#60190=CARTESIAN_POINT('',(8.30700212696576,-23.44,78.0634055730105));
#60191=CARTESIAN_POINT('Ctrl Pts',(10.0375846303818,-23.44,78.6932860921958));
#60192=CARTESIAN_POINT('Ctrl Pts',(9.96378821732871,-23.4632503226554,78.7707333921188));
#60193=CARTESIAN_POINT('Ctrl Pts',(9.78849047425474,-23.5225924173496,78.9050100514895));
#60194=CARTESIAN_POINT('Ctrl Pts',(9.51299812381197,-23.5976720228355,78.9966426113753));
#60195=CARTESIAN_POINT('Ctrl Pts',(9.27165366179481,-23.6401744298665,79.0099541241551));
#60196=CARTESIAN_POINT('Ctrl Pts',(9.08912965205693,-23.6586188959259,78.9859235830548));
#60197=CARTESIAN_POINT('Ctrl Pts',(8.92062369891718,-23.6619658680752,78.93222291379));
#60198=CARTESIAN_POINT('Ctrl Pts',(8.75994339020282,-23.6505635245521,78.8477059319911));
#60199=CARTESIAN_POINT('Ctrl Pts',(8.61580639791841,-23.6244291357707,78.7342228481503));
#60200=CARTESIAN_POINT('Ctrl Pts',(8.53710751827929,-23.5995950380918,78.6449366444775));
#60201=CARTESIAN_POINT('Ctrl Pts',(8.4893081082794,-23.5810512812345,78.5804189420813));
#60202=CARTESIAN_POINT('Ctrl Pts',(8.47679119967003,-23.5757772780198,78.5622829233047));
#60203=CARTESIAN_POINT('Ctrl Pts',(8.36906164076755,-23.5268334295508,78.3949081991338));
#60204=CARTESIAN_POINT('Ctrl Pts',(8.31739801874628,-23.4758129863659,78.2278557443297));
#60205=CARTESIAN_POINT('Ctrl Pts',(8.30700212696576,-23.44,78.0634055730105));
#60206=CARTESIAN_POINT('',(10.3129978730329,-23.4400000000023,77.9365944269688));
#60207=CARTESIAN_POINT('Origin',(9.31,-23.44,78.));
#60208=CARTESIAN_POINT('',(8.58241536963251,-23.4400000000023,77.3067139077891));
#60209=CARTESIAN_POINT('Ctrl Pts',(8.58241536961817,-23.44,77.3067139078042));
#60210=CARTESIAN_POINT('Ctrl Pts',(8.65618600625714,-23.4632422015298,77.2292936595168));
#60211=CARTESIAN_POINT('Ctrl Pts',(8.83158910154321,-23.522637422146,77.0950063597563));
#60212=CARTESIAN_POINT('Ctrl Pts',(9.10686435836405,-23.5977025591498,77.003294081653));
#60213=CARTESIAN_POINT('Ctrl Pts',(9.34839642462173,-23.6401800947028,76.9900977598095));
#60214=CARTESIAN_POINT('Ctrl Pts',(9.54592789251119,-23.6601491700001,77.0161150091369));
#60215=CARTESIAN_POINT('Ctrl Pts',(9.71319142839158,-23.6616254923616,77.0735905656994));
#60216=CARTESIAN_POINT('Ctrl Pts',(9.92566013575099,-23.644055915951,77.1912681046098));
#60217=CARTESIAN_POINT('Ctrl Pts',(10.0483680006109,-23.6129990647924,77.3084577996669));
#60218=CARTESIAN_POINT('Ctrl Pts',(10.1306989862535,-23.5810249250644,77.4196554703819));
#60219=CARTESIAN_POINT('Ctrl Pts',(10.1432239502022,-23.5757515322204,77.4377948245863));
#60220=CARTESIAN_POINT('Ctrl Pts',(10.2509072559687,-23.5268295608697,77.6050981709781));
#60221=CARTESIAN_POINT('Ctrl Pts',(10.3026077290777,-23.4757931855883,77.7722351791483));
#60222=CARTESIAN_POINT('Ctrl Pts',(10.3129978730342,-23.44,77.9365944269895));
#60223=CARTESIAN_POINT('',(8.305,-23.44,78.));
#60224=CARTESIAN_POINT('Origin',(9.31,-23.44,78.));
#60225=CARTESIAN_POINT('',(8.305,-24.485,78.));
#60226=CARTESIAN_POINT('Origin',(9.31,-23.44,78.));
#60227=CARTESIAN_POINT('Origin',(9.31,-25.5,78.));
#60228=CARTESIAN_POINT('',(2.01,-25.5,78.));
#60229=CARTESIAN_POINT('Origin',(9.31,-25.5,78.));
#60230=CARTESIAN_POINT('Ctrl Pts',(10.100212007486,-23.2297865267127,78.8219759032923));
#60231=CARTESIAN_POINT('Ctrl Pts',(10.0103245365164,-23.2613499461505,78.912999905046));
#60232=CARTESIAN_POINT('Ctrl Pts',(9.80443306533852,-23.339235126355,79.0610556336041));
#60233=CARTESIAN_POINT('Ctrl Pts',(9.50086601864425,-23.4330668442817,79.1505987981109));
#60234=CARTESIAN_POINT('Ctrl Pts',(9.24114419357868,-23.4856018928221,79.1585650126785));
#60235=CARTESIAN_POINT('Ctrl Pts',(9.04620851329942,-23.5082837204292,79.1299209668847));
#60236=CARTESIAN_POINT('Ctrl Pts',(8.86630044007771,-23.5123967187664,79.0720196330274));
#60237=CARTESIAN_POINT('Ctrl Pts',(8.69364486134355,-23.4983842652002,78.9832904164185));
#60238=CARTESIAN_POINT('Ctrl Pts',(8.53662363166247,-23.4661751204574,78.8648197598721));
#60239=CARTESIAN_POINT('Ctrl Pts',(8.4489747625146,-23.4353586041831,78.7708091230029));
#60240=CARTESIAN_POINT('Ctrl Pts',(8.39503262461223,-23.4122040782005,78.7021958553138));
#60241=CARTESIAN_POINT('Ctrl Pts',(8.38081350063257,-23.4055972563583,78.6828313686353));
#60242=CARTESIAN_POINT('Ctrl Pts',(8.2578365866536,-23.3442373462283,78.5034801846723));
#60243=CARTESIAN_POINT('Ctrl Pts',(8.19224688382286,-23.2784043599677,78.3181334130021));
#60244=CARTESIAN_POINT('Ctrl Pts',(8.17630655668227,-23.2297865267127,78.1217315856572));
#60245=CARTESIAN_POINT('Ctrl Pts',(10.0793362151179,-23.2998576844751,78.7790792995935));
#60246=CARTESIAN_POINT('Ctrl Pts',(9.99485230101193,-23.3286228262624,78.8655473612077));
#60247=CARTESIAN_POINT('Ctrl Pts',(9.79910201738819,-23.4003640892565,79.009055802932));
#60248=CARTESIAN_POINT('Ctrl Pts',(9.50491384035135,-23.4879249343831,79.0992633727804));
#60249=CARTESIAN_POINT('Ctrl Pts',(9.25130749167517,-23.5371227532837,79.1090171864575));
#60250=CARTESIAN_POINT('Ctrl Pts',(9.06051438646356,-23.5583916441821,79.0819108022503));
#60251=CARTESIAN_POINT('Ctrl Pts',(8.88441470298779,-23.5622512059598,79.0254124040774));
#60252=CARTESIAN_POINT('Ctrl Pts',(8.71574308357439,-23.5491044557046,78.938087008499));
#60253=CARTESIAN_POINT('Ctrl Pts',(8.56302183467341,-23.5189230023405,78.8212783528971));
#60254=CARTESIAN_POINT('Ctrl Pts',(8.47834776994348,-23.4900971027019,78.7288410132963));
#60255=CARTESIAN_POINT('Ctrl Pts',(8.42645705160579,-23.4684807083556,78.6615934910345));
#60256=CARTESIAN_POINT('Ctrl Pts',(8.41280930323009,-23.462321544408,78.6426422389549));
#60257=CARTESIAN_POINT('Ctrl Pts',(8.29488073666906,-23.4050771273758,78.4672608815071));
#60258=CARTESIAN_POINT('Ctrl Pts',(8.23391095961167,-23.3441519573982,78.2879642490827));
#60259=CARTESIAN_POINT('Ctrl Pts',(8.21987174677676,-23.2998576844751,78.1022895814417));
#60260=CARTESIAN_POINT('Ctrl Pts',(10.0584604227499,-23.3699288422376,78.7361826958946));
#60261=CARTESIAN_POINT('Ctrl Pts',(9.97926045283321,-23.3959774425435,78.8181859359572));
#60262=CARTESIAN_POINT('Ctrl Pts',(9.79382152220507,-23.4614634544481,78.9570098821616));
#60263=CARTESIAN_POINT('Ctrl Pts',(9.50895030210486,-23.5428139327341,79.0479780367058));
#60264=CARTESIAN_POINT('Ctrl Pts',(9.26149036369832,-23.5886535694049,79.0595019503761));
#60265=CARTESIAN_POINT('Ctrl Pts',(9.07482377889279,-23.608510972173,79.0339337476891));
#60266=CARTESIAN_POINT('Ctrl Pts',(8.9025094360071,-23.6121113808818,78.97883014274));
#60267=CARTESIAN_POINT('Ctrl Pts',(8.73784516797198,-23.5998433340478,78.8929093399106));
#60268=CARTESIAN_POINT('Ctrl Pts',(8.58940819490746,-23.5716812538877,78.7777642551252));
#60269=CARTESIAN_POINT('Ctrl Pts',(8.50773451085042,-23.5448565395729,78.6869047541841));
#60270=CARTESIAN_POINT('Ctrl Pts',(8.45788368128585,-23.5247746510794,78.6210213063607));
#60271=CARTESIAN_POINT('Ctrl Pts',(8.44479539707251,-23.5190529899701,78.602472052985));
#60272=CARTESIAN_POINT('Ctrl Pts',(8.3320174907521,-23.4659936484033,78.431127502299));
#60273=CARTESIAN_POINT('Ctrl Pts',(8.27573394295747,-23.4100653889354,78.2580249082491));
#60274=CARTESIAN_POINT('Ctrl Pts',(8.26343693687126,-23.3699288422376,78.0828475772261));
#60275=CARTESIAN_POINT('Ctrl Pts',(10.0375846303818,-23.44,78.6932860921958));
#60276=CARTESIAN_POINT('Ctrl Pts',(9.96378821732871,-23.4632503226554,78.7707333921188));
#60277=CARTESIAN_POINT('Ctrl Pts',(9.78849047425474,-23.5225924173496,78.9050100514895));
#60278=CARTESIAN_POINT('Ctrl Pts',(9.51299812381197,-23.5976720228355,78.9966426113753));
#60279=CARTESIAN_POINT('Ctrl Pts',(9.27165366179481,-23.6401744298665,79.0099541241551));
#60280=CARTESIAN_POINT('Ctrl Pts',(9.08912965205693,-23.6586188959259,78.9859235830548));
#60281=CARTESIAN_POINT('Ctrl Pts',(8.92062369891718,-23.6619658680752,78.93222291379));
#60282=CARTESIAN_POINT('Ctrl Pts',(8.75994339020282,-23.6505635245521,78.8477059319911));
#60283=CARTESIAN_POINT('Ctrl Pts',(8.61580639791841,-23.6244291357707,78.7342228481503));
#60284=CARTESIAN_POINT('Ctrl Pts',(8.53710751827929,-23.5995950380918,78.6449366444775));
#60285=CARTESIAN_POINT('Ctrl Pts',(8.4893081082794,-23.5810512812345,78.5804189420813));
#60286=CARTESIAN_POINT('Ctrl Pts',(8.47679119967003,-23.5757772780198,78.5622829233047));
#60287=CARTESIAN_POINT('Ctrl Pts',(8.36906164076755,-23.5268334295508,78.3949081991338));
#60288=CARTESIAN_POINT('Ctrl Pts',(8.31739801874628,-23.4758129863659,78.2278557443297));
#60289=CARTESIAN_POINT('Ctrl Pts',(8.30700212696576,-23.44,78.0634055730105));
#60290=CARTESIAN_POINT('Ctrl Pts',(10.0375846303818,-23.44,78.6932860921958));
#60291=CARTESIAN_POINT('Ctrl Pts',(9.9599378066044,-23.44,78.7997428949848));
#60292=CARTESIAN_POINT('Ctrl Pts',(9.86722691076642,-23.44,78.8961653627146));
#60293=CARTESIAN_POINT('Ctrl Pts',(9.66852004688849,-23.44,79.0475540438521));
#60294=CARTESIAN_POINT('Ctrl Pts',(9.56417005974731,-23.44,79.106184738785));
#60295=CARTESIAN_POINT('Ctrl Pts',(9.45276488839657,-23.44,79.1451885759221));
#60296=CARTESIAN_POINT('Ctrl Pts',(8.46452272321397,-23.44,78.7854978435489));
#60297=CARTESIAN_POINT('Ctrl Pts',(8.42330536322784,-23.44,78.716092159532));
#60298=CARTESIAN_POINT('Ctrl Pts',(8.39052202042233,-23.44,78.6417586933716));
#60299=CARTESIAN_POINT('Ctrl Pts',(8.31364989985943,-23.44,78.4045407779282));
#60300=CARTESIAN_POINT('Ctrl Pts',(8.29551551211911,-23.44,78.2321594268118));
#60301=CARTESIAN_POINT('Ctrl Pts',(8.30700212696576,-23.44,78.0634055730105));
#60302=CARTESIAN_POINT('Ctrl Pts',(8.519787992514,-23.2297865267127,77.1780240967077));
#60303=CARTESIAN_POINT('Ctrl Pts',(8.60964406660961,-23.2613389213359,77.0870318888077));
#60304=CARTESIAN_POINT('Ctrl Pts',(8.81560969574407,-23.339249297738,76.9390093127447));
#60305=CARTESIAN_POINT('Ctrl Pts',(9.11896640120719,-23.4330872349703,76.8493596419297));
#60306=CARTESIAN_POINT('Ctrl Pts',(9.3788902833647,-23.4855876966743,76.8415124408269));
#60307=CARTESIAN_POINT('Ctrl Pts',(9.58984999260555,-23.5101434522743,76.872532168987));
#60308=CARTESIAN_POINT('Ctrl Pts',(9.76844966013923,-23.5119591404095,76.9341462709327));
#60309=CARTESIAN_POINT('Ctrl Pts',(9.99707390435989,-23.4903522775185,77.0575739991169));
#60310=CARTESIAN_POINT('Ctrl Pts',(10.1320938555494,-23.4520581358879,77.1796744771316));
#60311=CARTESIAN_POINT('Ctrl Pts',(10.2250132495704,-23.412138947756,77.2979250401662));
#60312=CARTESIAN_POINT('Ctrl Pts',(10.2392416738491,-23.4055315301041,77.3172947002189));
#60313=CARTESIAN_POINT('Ctrl Pts',(10.3621589089987,-23.3442025877036,77.496565902309));
#60314=CARTESIAN_POINT('Ctrl Pts',(10.427761929485,-23.2783774794697,77.681975176348));
#60315=CARTESIAN_POINT('Ctrl Pts',(10.4436934433177,-23.2297865267127,77.8782684143427));
#60316=CARTESIAN_POINT('Ctrl Pts',(8.54066378488206,-23.2998576844752,77.2209207004065));
#60317=CARTESIAN_POINT('Ctrl Pts',(8.62510929439727,-23.3286069304059,77.1344916746785));
#60318=CARTESIAN_POINT('Ctrl Pts',(8.8209342962108,-23.4003746742759,76.9910095890714));
#60319=CARTESIAN_POINT('Ctrl Pts',(9.11491770383446,-23.4879441141189,76.9006932924059));
#60320=CARTESIAN_POINT('Ctrl Pts',(9.36872278502232,-23.5371069494853,76.8910608603316));
#60321=CARTESIAN_POINT('Ctrl Pts',(9.57520010070161,-23.5601348424691,76.9204112874013));
#60322=CARTESIAN_POINT('Ctrl Pts',(9.75002742645247,-23.56183762232,76.9806466551884));
#60323=CARTESIAN_POINT('Ctrl Pts',(9.97326596229238,-23.5415767678213,77.1021600329057));
#60324=CARTESIAN_POINT('Ctrl Pts',(10.1042121603643,-23.5056801367365,77.222624707157));
#60325=CARTESIAN_POINT('Ctrl Pts',(10.1935880244434,-23.4684159698535,77.3385282257988));
#60326=CARTESIAN_POINT('Ctrl Pts',(10.2072463553255,-23.462255399493,77.3574841605641));
#60327=CARTESIAN_POINT('Ctrl Pts',(10.3251091704039,-23.4050474225909,77.5327786005297));
#60328=CARTESIAN_POINT('Ctrl Pts',(10.3861102406279,-23.3441130561887,77.7121608586934));
#60329=CARTESIAN_POINT('Ctrl Pts',(10.4001282532232,-23.2998576844752,77.8977104185583));
#60330=CARTESIAN_POINT('Ctrl Pts',(8.56153957725011,-23.3699288422376,77.2638173041054));
#60331=CARTESIAN_POINT('Ctrl Pts',(8.64072077846948,-23.3959741924597,77.1818338736461));
#60332=CARTESIAN_POINT('Ctrl Pts',(8.82626450107649,-23.4615120456081,77.0430060834296));
#60333=CARTESIAN_POINT('Ctrl Pts',(9.11091305573679,-23.5428456800012,76.9519604311767));
#60334=CARTESIAN_POINT('Ctrl Pts',(9.35856392296411,-23.5886608418917,76.9405493403047));
#60335=CARTESIAN_POINT('Ctrl Pts',(9.56057778441512,-23.6101577798053,76.9682358907225));
#60336=CARTESIAN_POINT('Ctrl Pts',(9.73161366207835,-23.611747010451,77.0270901814438));
#60337=CARTESIAN_POINT('Ctrl Pts',(9.9494680778185,-23.5928314256482,77.146682070821));
#60338=CARTESIAN_POINT('Ctrl Pts',(10.0762496957961,-23.5593770639438,77.2655075696414));
#60339=CARTESIAN_POINT('Ctrl Pts',(10.1621242113804,-23.5247479029669,77.3790522847493));
#60340=CARTESIAN_POINT('Ctrl Pts',(10.1752192687258,-23.5190276628316,77.3976053642411));
#60341=CARTESIAN_POINT('Ctrl Pts',(10.2879569945636,-23.4659847259824,77.5688854727573));
#60342=CARTESIAN_POINT('Ctrl Pts',(10.3442594179347,-23.4100576088693,77.742049496803));
#60343=CARTESIAN_POINT('Ctrl Pts',(10.3565630631287,-23.3699288422376,77.9171524227739));
#60344=CARTESIAN_POINT('Ctrl Pts',(8.58241536961817,-23.44,77.3067139078042));
#60345=CARTESIAN_POINT('Ctrl Pts',(8.65618600625714,-23.4632422015298,77.2292936595168));
#60346=CARTESIAN_POINT('Ctrl Pts',(8.83158910154321,-23.522637422146,77.0950063597563));
#60347=CARTESIAN_POINT('Ctrl Pts',(9.10686435836405,-23.5977025591498,77.003294081653));
#60348=CARTESIAN_POINT('Ctrl Pts',(9.34839642462173,-23.6401800947028,76.9900977598095));
#60349=CARTESIAN_POINT('Ctrl Pts',(9.54592789251119,-23.6601491700001,77.0161150091369));
#60350=CARTESIAN_POINT('Ctrl Pts',(9.71319142839158,-23.6616254923616,77.0735905656994));
#60351=CARTESIAN_POINT('Ctrl Pts',(9.92566013575099,-23.644055915951,77.1912681046098));
#60352=CARTESIAN_POINT('Ctrl Pts',(10.0483680006109,-23.6129990647924,77.3084577996669));
#60353=CARTESIAN_POINT('Ctrl Pts',(10.1306989862535,-23.5810249250644,77.4196554703819));
#60354=CARTESIAN_POINT('Ctrl Pts',(10.1432239502022,-23.5757515322204,77.4377948245863));
#60355=CARTESIAN_POINT('Ctrl Pts',(10.2509072559687,-23.5268295608697,77.6050981709781));
#60356=CARTESIAN_POINT('Ctrl Pts',(10.3026077290777,-23.4757931855883,77.7722351791483));
#60357=CARTESIAN_POINT('Ctrl Pts',(10.3129978730342,-23.44,77.9365944269895));
#60358=CARTESIAN_POINT('Ctrl Pts',(8.58241536961817,-23.44,77.3067139078042));
#60359=CARTESIAN_POINT('Ctrl Pts',(8.66006016612818,-23.44,77.2002598844773));
#60360=CARTESIAN_POINT('Ctrl Pts',(8.75276823603309,-23.44,77.1038396887893));
#60361=CARTESIAN_POINT('Ctrl Pts',(8.95147388732374,-23.44,76.9524493606504));
#60362=CARTESIAN_POINT('Ctrl Pts',(9.05582670211928,-23.44,76.8938163949113));
#60363=CARTESIAN_POINT('Ctrl Pts',(9.16723511160343,-23.44,76.8548114240778));
#60364=CARTESIAN_POINT('Ctrl Pts',(10.155477276786,-23.44,77.2145021564511));
#60365=CARTESIAN_POINT('Ctrl Pts',(10.1966868174929,-23.44,77.283894673627));
#60366=CARTESIAN_POINT('Ctrl Pts',(10.229465540476,-23.44,77.3582131109841));
#60367=CARTESIAN_POINT('Ctrl Pts',(10.3063468190756,-23.44,77.5954278309571));
#60368=CARTESIAN_POINT('Ctrl Pts',(10.3244855296182,-23.44,77.7678252686633));
#60369=CARTESIAN_POINT('Ctrl Pts',(10.3129978730342,-23.44,77.9365944269895));
#60370=CARTESIAN_POINT('Ctrl Pts',(12.1440294707702,-15.3457361617732,78.9916063779574));
#60371=CARTESIAN_POINT('Ctrl Pts',(12.0821287866527,-15.3383729044183,79.1685196844361));
#60372=CARTESIAN_POINT('Ctrl Pts',(11.9811196883727,-15.4003238547929,79.3825863055803));
#60373=CARTESIAN_POINT('Ctrl Pts',(11.8251071448527,-15.616984349081,79.6451820555524));
#60374=CARTESIAN_POINT('Ctrl Pts',(11.6852150750259,-15.9157775367878,79.8401596355449));
#60375=CARTESIAN_POINT('Ctrl Pts',(11.6322385355776,-16.4531466810754,79.9023659741719));
#60376=CARTESIAN_POINT('Ctrl Pts',(11.7419583042977,-16.8055520460372,79.7657541392426));
#60377=CARTESIAN_POINT('Ctrl Pts',(11.822863335852,-16.9636835154004,79.6436043679924));
#60378=CARTESIAN_POINT('Ctrl Pts',(11.8340060584782,-16.9839356481672,79.626485701499));
#60379=CARTESIAN_POINT('Ctrl Pts',(11.8910343120941,-17.0804741647385,79.5365456795022));
#60380=CARTESIAN_POINT('Ctrl Pts',(11.9963709991369,-17.2117774433501,79.3562680459212));
#60381=CARTESIAN_POINT('Ctrl Pts',(12.0925286612292,-17.2551291983681,79.1341301729733));
#60382=CARTESIAN_POINT('Ctrl Pts',(12.1731938226851,-17.2549658653676,78.9122669584772));
#60383=CARTESIAN_POINT('Ctrl Pts',(12.228036692318,-17.218306148821,78.7260201971924));
#60384=CARTESIAN_POINT('Ctrl Pts',(12.2717094191553,-17.0934753320961,78.5017481928062));
#60385=CARTESIAN_POINT('Ctrl Pts',(12.2987015121157,-16.9349741098207,78.3119581382534));
#60386=CARTESIAN_POINT('Ctrl Pts',(12.3081423262004,-16.7295975635937,78.172212569198));
#60387=CARTESIAN_POINT('Ctrl Pts',(12.3111010412262,-16.492435283584,78.0968890708661));
#60388=CARTESIAN_POINT('Ctrl Pts',(12.3115831055068,-16.2454177966105,78.0700185886829));
#60389=CARTESIAN_POINT('Ctrl Pts',(12.3106379014819,-15.9361493339683,78.1306696064297));
#60390=CARTESIAN_POINT('Ctrl Pts',(12.2972420283652,-15.6231316758572,78.3377707078825));
#60391=CARTESIAN_POINT('Ctrl Pts',(12.2499737983051,-15.4084011027765,78.6408069135594));
#60392=CARTESIAN_POINT('Ctrl Pts',(12.1846480803193,-15.3505678575739,78.8755176364136));
#60393=CARTESIAN_POINT('Ctrl Pts',(12.1440294707702,-15.3457361617732,78.9916063779574));
#60394=CARTESIAN_POINT('Ctrl Pts',(12.1905411751434,-15.395718781424,79.0100646834078));
#60395=CARTESIAN_POINT('Ctrl Pts',(12.1307865477481,-15.3884188195122,79.1802503183488));
#60396=CARTESIAN_POINT('Ctrl Pts',(12.0347735529135,-15.4494252933908,79.3861988883646));
#60397=CARTESIAN_POINT('Ctrl Pts',(11.8885687474473,-15.6581438008607,79.636587449847));
#60398=CARTESIAN_POINT('Ctrl Pts',(11.7598527815262,-15.9428103951435,79.8196635436855));
#60399=CARTESIAN_POINT('Ctrl Pts',(11.7123017216896,-16.4419422338359,79.8765562283324));
#60400=CARTESIAN_POINT('Ctrl Pts',(11.8116717647762,-16.7724433312399,79.7503244727558));
#60401=CARTESIAN_POINT('Ctrl Pts',(11.8868691413704,-16.9237865974938,79.6346407897848));
#60402=CARTESIAN_POINT('Ctrl Pts',(11.8971829796672,-16.9430695195421,79.618457434879));
#60403=CARTESIAN_POINT('Ctrl Pts',(11.9502752858818,-17.0355212070356,79.5331286750323));
#60404=CARTESIAN_POINT('Ctrl Pts',(12.0491364656578,-17.1626660611137,79.3609572273587));
#60405=CARTESIAN_POINT('Ctrl Pts',(12.1410059087477,-17.2051327276356,79.1471173412086));
#60406=CARTESIAN_POINT('Ctrl Pts',(12.2185735988939,-17.2049790741984,78.9337592374503));
#60407=CARTESIAN_POINT('Ctrl Pts',(12.2718391220554,-17.1690378747736,78.7548462589905));
#60408=CARTESIAN_POINT('Ctrl Pts',(12.3149022681015,-17.0481569211274,78.5414316970799));
#60409=CARTESIAN_POINT('Ctrl Pts',(12.3419162375973,-16.89588396213,78.3621822312909));
#60410=CARTESIAN_POINT('Ctrl Pts',(12.3519442672886,-16.7012080271386,78.2321915109205));
#60411=CARTESIAN_POINT('Ctrl Pts',(12.3553529574687,-16.4792730984203,78.1627644017751));
#60412=CARTESIAN_POINT('Ctrl Pts',(12.3560377852108,-16.2491700223592,78.1381695110903));
#60413=CARTESIAN_POINT('Ctrl Pts',(12.3546266916132,-15.9610344808616,78.1936295942804));
#60414=CARTESIAN_POINT('Ctrl Pts',(12.3403320117296,-15.6644959222293,78.3860774975201));
#60415=CARTESIAN_POINT('Ctrl Pts',(12.2932391850083,-15.4570233754469,78.673215845813));
#60416=CARTESIAN_POINT('Ctrl Pts',(12.2296649765981,-15.4004233493121,78.8984274812488));
#60417=CARTESIAN_POINT('Ctrl Pts',(12.1905411751434,-15.395718781424,79.0100646834078));
#60418=CARTESIAN_POINT('Ctrl Pts',(12.2370528795166,-15.4457014010748,79.0285229888583));
#60419=CARTESIAN_POINT('Ctrl Pts',(12.1798257226226,-15.4387970155116,79.1916890394376));
#60420=CARTESIAN_POINT('Ctrl Pts',(12.0884081621552,-15.4985468621786,79.3898292947456));
#60421=CARTESIAN_POINT('Ctrl Pts',(11.9522340660948,-15.6994288658102,79.6278251275205));
#60422=CARTESIAN_POINT('Ctrl Pts',(11.834568849452,-15.9701317113529,79.7991100429138));
#60423=CARTESIAN_POINT('Ctrl Pts',(11.7920587468212,-16.4301848099057,79.8510263063962));
#60424=CARTESIAN_POINT('Ctrl Pts',(11.8815772239625,-16.7400260169906,79.7347243019166));
#60425=CARTESIAN_POINT('Ctrl Pts',(11.9506563012613,-16.883501785339,79.6258869212831));
#60426=CARTESIAN_POINT('Ctrl Pts',(11.9602409595347,-16.9020175268376,79.6105578504383));
#60427=CARTESIAN_POINT('Ctrl Pts',(12.0094076680351,-16.9904823469893,79.5297823783282));
#60428=CARTESIAN_POINT('Ctrl Pts',(12.1018520459692,-17.1134311038727,79.3657191698453));
#60429=CARTESIAN_POINT('Ctrl Pts',(12.1894185541784,-17.1550573199279,79.1601685949679));
#60430=CARTESIAN_POINT('Ctrl Pts',(12.2639231573512,-17.1548908469061,78.9552998254218));
#60431=CARTESIAN_POINT('Ctrl Pts',(12.3155809210026,-17.1197507947583,78.783714952818));
#60432=CARTESIAN_POINT('Ctrl Pts',(12.3580545728541,-17.0027799265832,78.5811277203043));
#60433=CARTESIAN_POINT('Ctrl Pts',(12.3850999349634,-16.8567601611705,78.412439808554));
#60434=CARTESIAN_POINT('Ctrl Pts',(12.395719201828,-16.6728435871762,78.2921907493411));
#60435=CARTESIAN_POINT('Ctrl Pts',(12.3995908338668,-16.4661177374306,78.2286929082959));
#60436=CARTESIAN_POINT('Ctrl Pts',(12.4004721034329,-16.2529370512118,78.2063226605274));
#60437=CARTESIAN_POINT('Ctrl Pts',(12.3986099640282,-15.9858739114076,78.2566551537243));
#60438=CARTESIAN_POINT('Ctrl Pts',(12.3834130133868,-15.7059406852543,78.4344048281252));
#60439=CARTESIAN_POINT('Ctrl Pts',(12.3364987711348,-15.5056308812999,78.7056068063562));
#60440=CARTESIAN_POINT('Ctrl Pts',(12.2746913544106,-15.4503175838733,78.921418150445));
#60441=CARTESIAN_POINT('Ctrl Pts',(12.2370528795166,-15.4457014010748,79.0285229888583));
#60442=CARTESIAN_POINT('Ctrl Pts',(12.2835645838897,-15.4956840207256,79.0469812943087));
#60443=CARTESIAN_POINT('Ctrl Pts',(12.228483483718,-15.4888429306054,79.2034196733504));
#60444=CARTESIAN_POINT('Ctrl Pts',(12.1420620266961,-15.5476483007766,79.3934418775299));
#60445=CARTESIAN_POINT('Ctrl Pts',(12.0156956686893,-15.7405883175899,79.6192305218151));
#60446=CARTESIAN_POINT('Ctrl Pts',(11.9092065559523,-15.9971645697086,79.7786139510543));
#60447=CARTESIAN_POINT('Ctrl Pts',(11.8721219329333,-16.4189803626662,79.8252165605567));
#60448=CARTESIAN_POINT('Ctrl Pts',(11.951290684441,-16.7069173021933,79.7192946354299));
#60449=CARTESIAN_POINT('Ctrl Pts',(12.0146621067797,-16.8436048674325,79.6169233430755));
#60450=CARTESIAN_POINT('Ctrl Pts',(12.0234178807236,-16.8611513982124,79.6025295838183));
#60451=CARTESIAN_POINT('Ctrl Pts',(12.0686486418228,-16.9455293892864,79.5263653738583));
#60452=CARTESIAN_POINT('Ctrl Pts',(12.1546175124901,-17.0643197216363,79.3704083512828));
#60453=CARTESIAN_POINT('Ctrl Pts',(12.2378958016969,-17.1050608491954,79.1731557632031));
#60454=CARTESIAN_POINT('Ctrl Pts',(12.3093029335599,-17.1049040557369,78.9767921043949));
#60455=CARTESIAN_POINT('Ctrl Pts',(12.35938335074,-17.0704825207109,78.8125410146161));
#60456=CARTESIAN_POINT('Ctrl Pts',(12.4012474218003,-16.9574615156145,78.620811224578));
#60457=CARTESIAN_POINT('Ctrl Pts',(12.4283146604451,-16.8176700134799,78.4626639015916));
#60458=CARTESIAN_POINT('Ctrl Pts',(12.4395211429162,-16.6444540507211,78.3521696910637));
#60459=CARTESIAN_POINT('Ctrl Pts',(12.4438427501093,-16.4529555522669,78.2945682392049));
#60460=CARTESIAN_POINT('Ctrl Pts',(12.444926783137,-16.2566892769605,78.2744735829348));
#60461=CARTESIAN_POINT('Ctrl Pts',(12.4425987541595,-16.010759058301,78.319615141575));
#60462=CARTESIAN_POINT('Ctrl Pts',(12.4265029967512,-15.7473049316263,78.4827116177628));
#60463=CARTESIAN_POINT('Ctrl Pts',(12.379764157838,-15.5542531539703,78.7380157386097));
#60464=CARTESIAN_POINT('Ctrl Pts',(12.3197082506894,-15.5001730756115,78.9443279952801));
#60465=CARTESIAN_POINT('Ctrl Pts',(12.2835645838897,-15.4956840207256,79.0469812943087));
#60466=CARTESIAN_POINT('',(12.1440294707702,-15.3457361617732,78.9916063779574));
#60467=CARTESIAN_POINT('',(12.2835645838897,-15.4956840207256,79.0469812943087));
#60468=CARTESIAN_POINT('',(12.1440294707702,-15.3457361617732,78.9916063779574));
#60469=CARTESIAN_POINT('',(12.4444120815709,-16.3000163632569,78.2841628434877));
#60470=CARTESIAN_POINT('Ctrl Pts',(12.2835645838897,-15.4956840207256,79.0469812943087));
#60471=CARTESIAN_POINT('Ctrl Pts',(12.228483483718,-15.4888429306054,79.2034196733504));
#60472=CARTESIAN_POINT('Ctrl Pts',(12.1420620266961,-15.5476483007766,79.3934418775299));
#60473=CARTESIAN_POINT('Ctrl Pts',(12.0156956686893,-15.7405883175899,79.6192305218151));
#60474=CARTESIAN_POINT('Ctrl Pts',(11.9092065559523,-15.9971645697086,79.7786139510543));
#60475=CARTESIAN_POINT('Ctrl Pts',(11.8721219329333,-16.4189803626662,79.8252165605567));
#60476=CARTESIAN_POINT('Ctrl Pts',(11.951290684441,-16.7069173021933,79.7192946354299));
#60477=CARTESIAN_POINT('Ctrl Pts',(12.0146621067797,-16.8436048674325,79.6169233430755));
#60478=CARTESIAN_POINT('Ctrl Pts',(12.0234178807236,-16.8611513982124,79.6025295838183));
#60479=CARTESIAN_POINT('Ctrl Pts',(12.0686486418228,-16.9455293892864,79.5263653738583));
#60480=CARTESIAN_POINT('Ctrl Pts',(12.1546175124901,-17.0643197216363,79.3704083512828));
#60481=CARTESIAN_POINT('Ctrl Pts',(12.2378958016969,-17.1050608491954,79.1731557632031));
#60482=CARTESIAN_POINT('Ctrl Pts',(12.3093029335599,-17.1049040557369,78.9767921043949));
#60483=CARTESIAN_POINT('Ctrl Pts',(12.35938335074,-17.0704825207109,78.8125410146161));
#60484=CARTESIAN_POINT('Ctrl Pts',(12.4012474218003,-16.9574615156145,78.620811224578));
#60485=CARTESIAN_POINT('Ctrl Pts',(12.4283146604451,-16.8176700134799,78.4626639015916));
#60486=CARTESIAN_POINT('Ctrl Pts',(12.4395211429162,-16.6444540507211,78.3521696910637));
#60487=CARTESIAN_POINT('Ctrl Pts',(12.4438427501093,-16.4529555522669,78.2945682392049));
#60488=CARTESIAN_POINT('Ctrl Pts',(12.4443952514524,-16.3529241160095,78.2843265544088));
#60489=CARTESIAN_POINT('Ctrl Pts',(12.4444118401433,-16.3019162824862,78.2841619672088));
#60490=CARTESIAN_POINT('Ctrl Pts',(12.4444120815709,-16.3000163632569,78.2841628434877));
#60491=CARTESIAN_POINT('Ctrl Pts',(12.4444120815709,-16.3000163632569,78.2841628434877));
#60492=CARTESIAN_POINT('Ctrl Pts',(12.4444243208177,-16.2036993661096,78.2842072667228));
#60493=CARTESIAN_POINT('Ctrl Pts',(12.442494968104,-16.0090602960789,78.3206667938524));
#60494=CARTESIAN_POINT('Ctrl Pts',(12.4265029967512,-15.7473049316263,78.4827116177628));
#60495=CARTESIAN_POINT('Ctrl Pts',(12.379764157838,-15.5542531539703,78.7380157386097));
#60496=CARTESIAN_POINT('Ctrl Pts',(12.3197082506894,-15.5001730756115,78.9443279952801));
#60497=CARTESIAN_POINT('Ctrl Pts',(12.2835645838897,-15.4956840207256,79.0469812943087));
#60498=CARTESIAN_POINT('',(12.2711805139213,-17.0828938614663,78.4968565980093));
#60499=CARTESIAN_POINT('Ctrl Pts',(12.1440294707702,-15.3457361617732,78.9916063779574));
#60500=CARTESIAN_POINT('Ctrl Pts',(12.1846480803193,-15.3505678575739,78.8755176364136));
#60501=CARTESIAN_POINT('Ctrl Pts',(12.2499737983051,-15.4084011027765,78.6408069135594));
#60502=CARTESIAN_POINT('Ctrl Pts',(12.2972420283652,-15.6231316758572,78.3377707078825));
#60503=CARTESIAN_POINT('Ctrl Pts',(12.3106379014819,-15.9361493339683,78.1306696064297));
#60504=CARTESIAN_POINT('Ctrl Pts',(12.3115831055068,-16.2454177966105,78.0700185886829));
#60505=CARTESIAN_POINT('Ctrl Pts',(12.3111010412262,-16.492435283584,78.0968890708661));
#60506=CARTESIAN_POINT('Ctrl Pts',(12.3081423262004,-16.7295975635937,78.172212569198));
#60507=CARTESIAN_POINT('Ctrl Pts',(12.2988420797468,-16.9319161855434,78.3098774168852));
#60508=CARTESIAN_POINT('Ctrl Pts',(12.2792560441049,-17.0491162087367,78.4486637689));
#60509=CARTESIAN_POINT('Ctrl Pts',(12.2711805139213,-17.0828938614663,78.4968565980093));
#60510=CARTESIAN_POINT('',(11.8979359134617,-17.0829544530057,79.5224663406848));
#60511=CARTESIAN_POINT('Ctrl Pts',(12.2711805139213,-17.0828938614663,78.4968565980093));
#60512=CARTESIAN_POINT('Ctrl Pts',(12.2706690975431,-17.0850329711507,78.4999086084107));
#60513=CARTESIAN_POINT('Ctrl Pts',(12.2614414961737,-17.1228243859493,78.5544769284436));
#60514=CARTESIAN_POINT('Ctrl Pts',(12.228036692318,-17.218306148821,78.7260201971924));
#60515=CARTESIAN_POINT('Ctrl Pts',(12.1731938226851,-17.2549658653676,78.9122669584772));
#60516=CARTESIAN_POINT('Ctrl Pts',(12.0925286612292,-17.2551291983681,79.1341301729733));
#60517=CARTESIAN_POINT('Ctrl Pts',(12.0139885788277,-17.2197201593246,79.3155689316349));
#60518=CARTESIAN_POINT('Ctrl Pts',(11.929324830863,-17.1256354200658,79.4690811831062));
#60519=CARTESIAN_POINT('Ctrl Pts',(11.8979359134617,-17.0829544530057,79.5224663406848));
#60520=CARTESIAN_POINT('Ctrl Pts',(11.8979359134617,-17.0829544530057,79.5224663406848));
#60521=CARTESIAN_POINT('Ctrl Pts',(11.8797818085212,-17.0582694743852,79.5533421985731));
#60522=CARTESIAN_POINT('Ctrl Pts',(11.862111845529,-17.0315136611155,79.5821596885964));
#60523=CARTESIAN_POINT('Ctrl Pts',(11.8340060584782,-16.9839356481672,79.626485701499));
#60524=CARTESIAN_POINT('Ctrl Pts',(11.822863335852,-16.9636835154004,79.6436043679924));
#60525=CARTESIAN_POINT('Ctrl Pts',(11.7419583042977,-16.8055520460372,79.7657541392426));
#60526=CARTESIAN_POINT('Ctrl Pts',(11.6322385355776,-16.4531466810754,79.9023659741719));
#60527=CARTESIAN_POINT('Ctrl Pts',(11.6852150750259,-15.9157775367878,79.8401596355449));
#60528=CARTESIAN_POINT('Ctrl Pts',(11.8251071448527,-15.616984349081,79.6451820555524));
#60529=CARTESIAN_POINT('Ctrl Pts',(11.9811196883727,-15.4003238547929,79.3825863055803));
#60530=CARTESIAN_POINT('Ctrl Pts',(12.0821287866527,-15.3383729044183,79.1685196844361));
#60531=CARTESIAN_POINT('Ctrl Pts',(12.1440294707702,-15.3457361617732,78.9916063779574));
#60532=CARTESIAN_POINT('Origin',(14.2351639486941,-16.3,79.7926130762057));
#60533=CARTESIAN_POINT('',(16.4513530905785,-16.3,79.7425768505124));
#60534=CARTESIAN_POINT('Ctrl Pts',(16.4513530905785,-16.3,79.7425768505124));
#60535=CARTESIAN_POINT('Ctrl Pts',(16.4513530905785,-16.3589692886209,79.7425768505124));
#60536=CARTESIAN_POINT('Ctrl Pts',(16.4480480854555,-16.4816735726619,79.7558601913112));
#60537=CARTESIAN_POINT('Ctrl Pts',(16.4325736298389,-16.6594622572905,79.8171984098592));
#60538=CARTESIAN_POINT('Ctrl Pts',(16.4062748363779,-16.8159706118973,79.9166929639477));
#60539=CARTESIAN_POINT('Ctrl Pts',(16.3729890665525,-16.9364358562187,80.0357782635816));
#60540=CARTESIAN_POINT('Ctrl Pts',(16.3356911646629,-17.0179798530874,80.1605114661715));
#60541=CARTESIAN_POINT('Ctrl Pts',(16.3058473255403,-17.0575804523145,80.254295100986));
#60542=CARTESIAN_POINT('Ctrl Pts',(16.2879525013642,-17.0755371418863,80.308927696043));
#60543=CARTESIAN_POINT('Ctrl Pts',(16.2415372469172,-17.1117868061966,80.447753029014));
#60544=CARTESIAN_POINT('Ctrl Pts',(16.1948063223941,-17.1115730952314,80.576147720836));
#60545=CARTESIAN_POINT('Ctrl Pts',(16.1449618162535,-17.0790101292845,80.7029348679748));
#60546=CARTESIAN_POINT('Ctrl Pts',(16.1307085706017,-17.0681960618883,80.7387696350713));
#60547=CARTESIAN_POINT('Ctrl Pts',(16.1056532177054,-17.0453545991598,80.800704934583));
#60548=CARTESIAN_POINT('Ctrl Pts',(16.0703540029782,-17.0022330082117,80.8851607398882));
#60549=CARTESIAN_POINT('Ctrl Pts',(16.0301839042296,-16.9342077983924,80.9775549085599));
#60550=CARTESIAN_POINT('Ctrl Pts',(15.9832611827489,-16.8301442655337,81.0820269634397));
#60551=CARTESIAN_POINT('Ctrl Pts',(15.9502407645414,-16.7212601418262,81.1524384808638));
#60552=CARTESIAN_POINT('Ctrl Pts',(15.9312021587559,-16.6273889065201,81.1923360286486));
#60553=CARTESIAN_POINT('Ctrl Pts',(15.9241925939478,-16.5891969664984,81.2069681165303));
#60554=CARTESIAN_POINT('Ctrl Pts',(15.9165903821184,-16.5402506433046,81.2227467611148));
#60555=CARTESIAN_POINT('Ctrl Pts',(15.91065385941,-16.4902046723651,81.2349960729889));
#60556=CARTESIAN_POINT('Ctrl Pts',(15.9069299685908,-16.4499097222704,81.2426581791741));
#60557=CARTESIAN_POINT('Ctrl Pts',(15.8993860003837,-16.3486391820234,81.2581428999399));
#60558=CARTESIAN_POINT('Ctrl Pts',(15.8993339911057,-16.2514057238454,81.2582653088229));
#60559=CARTESIAN_POINT('Ctrl Pts',(15.9068883109817,-16.1499522168206,81.2427575723468));
#60560=CARTESIAN_POINT('Ctrl Pts',(15.9106060634705,-16.1096920097338,81.2351100583515));
#60561=CARTESIAN_POINT('Ctrl Pts',(15.9189462667354,-16.039575969747,81.2178946689264));
#60562=CARTESIAN_POINT('Ctrl Pts',(15.9390487495246,-15.9236171521494,81.176123768719));
#60563=CARTESIAN_POINT('Ctrl Pts',(15.9780188589416,-15.7841245162218,81.093298797813));
#60564=CARTESIAN_POINT('Ctrl Pts',(16.0206262002669,-15.6838578074055,80.9992772183258));
#60565=CARTESIAN_POINT('Ctrl Pts',(16.0601083842914,-15.614453165806,80.9088149092774));
#60566=CARTESIAN_POINT('Ctrl Pts',(16.0913245109124,-15.5711026393277,80.8352208082551));
#60567=CARTESIAN_POINT('Ctrl Pts',(16.1140619626514,-15.5467976611288,80.7799456784944));
#60568=CARTESIAN_POINT('Ctrl Pts',(16.1274512959284,-15.5348564441079,80.7467731693007));
#60569=CARTESIAN_POINT('Ctrl Pts',(16.1328072862571,-15.5302830340556,80.7334485354894));
#60570=CARTESIAN_POINT('Ctrl Pts',(16.1381613217313,-15.5260194401552,80.7200442157294));
#60571=CARTESIAN_POINT('Ctrl Pts',(16.1435063115107,-15.5220675070163,80.7065768755647));
#60572=CARTESIAN_POINT('Ctrl Pts',(16.1475083522864,-15.5192597790203,80.6964500598804));
#60573=CARTESIAN_POINT('Ctrl Pts',(16.1508391816247,-15.5170502299053,80.6879848666869));
#60574=CARTESIAN_POINT('Ctrl Pts',(16.15349609922,-15.5153610551317,80.6812109984591));
#60575=CARTESIAN_POINT('Ctrl Pts',(16.1761138473566,-15.5014438248939,80.6234102411006));
#60576=CARTESIAN_POINT('Ctrl Pts',(16.2173799719997,-15.4890669000081,80.5140466644355));
#60577=CARTESIAN_POINT('Ctrl Pts',(16.256671069509,-15.5016526498119,80.4020055506128));
#60578=CARTESIAN_POINT('Ctrl Pts',(16.2776453806387,-15.5166287131285,80.339710128914));
#60579=CARTESIAN_POINT('Ctrl Pts',(16.2822621877799,-15.5201625714385,80.3259280683213));
#60580=CARTESIAN_POINT('Ctrl Pts',(16.2902787106003,-15.5269026562889,80.3018213429743));
#60581=CARTESIAN_POINT('Ctrl Pts',(16.3059640273659,-15.5425274630872,80.253955052204));
#60582=CARTESIAN_POINT('Ctrl Pts',(16.3272838914141,-15.5711106544873,80.1869069342357));
#60583=CARTESIAN_POINT('Ctrl Pts',(16.3506559088329,-15.6144081339517,80.1105373437524));
#60584=CARTESIAN_POINT('Ctrl Pts',(16.3786675677716,-15.6840040800632,80.0154883579624));
#60585=CARTESIAN_POINT('Ctrl Pts',(16.3965034681242,-15.7486486439767,79.9516745085037));
#60586=CARTESIAN_POINT('Ctrl Pts',(16.4088407689086,-15.8075043665704,79.9062850349126));
#60587=CARTESIAN_POINT('Ctrl Pts',(16.413584292267,-15.8316774627009,79.8887037060206));
#60588=CARTESIAN_POINT('Ctrl Pts',(16.4214143032745,-15.8757440839149,79.8594045459933));
#60589=CARTESIAN_POINT('Ctrl Pts',(16.4428541971365,-16.0236308749458,79.7774158873755));
#60590=CARTESIAN_POINT('Ctrl Pts',(16.4513530905785,-16.1820614227582,79.7425768505124));
#60591=CARTESIAN_POINT('Ctrl Pts',(16.4513530905785,-16.3,79.7425768505124));
#60592=CARTESIAN_POINT('',(14.5104901640713,-16.3,79.036160516473));
#60593=CARTESIAN_POINT('Origin',(9.31,-16.425,78.));
#60594=CARTESIAN_POINT('',(6.3075,-18.7,78.));
#60595=CARTESIAN_POINT('Origin',(9.31,-18.7,78.));
#60596=CARTESIAN_POINT('',(6.3075,-14.15,78.));
#60597=CARTESIAN_POINT('',(6.3075,-16.425,78.));
#60598=CARTESIAN_POINT('Origin',(9.31,-14.15,78.));
#60599=CARTESIAN_POINT('Ctrl Pts',(16.6267263258151,-16.3,79.647882238852));
#60600=CARTESIAN_POINT('Ctrl Pts',(16.6267263258151,-16.3686398740138,79.647882238852));
#60601=CARTESIAN_POINT('Ctrl Pts',(16.6232895344097,-16.5114662207145,79.6631181782204));
#60602=CARTESIAN_POINT('Ctrl Pts',(16.6070569699324,-16.7195440420054,79.7337450825527));
#60603=CARTESIAN_POINT('Ctrl Pts',(16.5787193153288,-16.9047265894586,79.8495489824192));
#60604=CARTESIAN_POINT('Ctrl Pts',(16.5417979890631,-17.0491114348861,79.9898247024023));
#60605=CARTESIAN_POINT('Ctrl Pts',(16.4991469954625,-17.1481299251104,80.1385791791468));
#60606=CARTESIAN_POINT('Ctrl Pts',(16.4642217393025,-17.1966318363056,80.251361487145));
#60607=CARTESIAN_POINT('Ctrl Pts',(16.4430881666924,-17.2186801784522,80.3172431103551));
#60608=CARTESIAN_POINT('Ctrl Pts',(16.3879482597749,-17.2633110844262,80.4849293868592));
#60609=CARTESIAN_POINT('Ctrl Pts',(16.3311939963963,-17.263076777122,80.640871035239));
#60610=CARTESIAN_POINT('Ctrl Pts',(16.2703393347549,-17.2229799642533,80.7935103025339));
#60611=CARTESIAN_POINT('Ctrl Pts',(16.2529286652786,-17.2096866928451,80.8365863008715));
#60612=CARTESIAN_POINT('Ctrl Pts',(16.2223085872669,-17.1816622921672,80.9108472236554));
#60613=CARTESIAN_POINT('Ctrl Pts',(16.1791754703243,-17.1289822618776,81.0115059847778));
#60614=CARTESIAN_POINT('Ctrl Pts',(16.1302272700693,-17.0466007917327,81.1205411519808));
#60615=CARTESIAN_POINT('Ctrl Pts',(16.0732729417727,-16.9216470840919,81.2426097135714));
#60616=CARTESIAN_POINT('Ctrl Pts',(16.0334936810962,-16.7925239444982,81.3235736952026));
#60617=CARTESIAN_POINT('Ctrl Pts',(16.0106538593799,-16.6821981103206,81.3691011936988));
#60618=CARTESIAN_POINT('Ctrl Pts',(16.0022521358187,-16.6373793785181,81.3857696123251));
#60619=CARTESIAN_POINT('Ctrl Pts',(15.9931529411453,-16.5800659147356,81.4036970257625));
#60620=CARTESIAN_POINT('Ctrl Pts',(15.9860578245946,-16.5216040414588,81.4175766075504));
#60621=CARTESIAN_POINT('Ctrl Pts',(15.9816103595508,-16.4745965934211,81.4262469365913));
#60622=CARTESIAN_POINT('Ctrl Pts',(15.9726062552113,-16.3565449674897,81.443748920257));
#60623=CARTESIAN_POINT('Ctrl Pts',(15.9725425009045,-16.2435059768007,81.4438943965471));
#60624=CARTESIAN_POINT('Ctrl Pts',(15.981559283011,-16.1252411321897,81.4263653146201));
#60625=CARTESIAN_POINT('Ctrl Pts',(15.9859992260481,-16.0782746472634,81.4177123723923));
#60626=CARTESIAN_POINT('Ctrl Pts',(15.9959680144551,-15.996365623908,81.3982024054527));
#60627=CARTESIAN_POINT('Ctrl Pts',(16.0200372266792,-15.8604273231654,81.3507157648354));
#60628=CARTESIAN_POINT('Ctrl Pts',(16.0669428124562,-15.6953850753735,81.2556190750553));
#60629=CARTESIAN_POINT('Ctrl Pts',(16.1185975434662,-15.5751968380705,81.1460824099368));
#60630=CARTESIAN_POINT('Ctrl Pts',(16.1666865284266,-15.4912543308356,81.0394472234925));
#60631=CARTESIAN_POINT('Ctrl Pts',(16.2047961808524,-15.4384721428059,80.952041722185));
#60632=CARTESIAN_POINT('Ctrl Pts',(16.2325860018634,-15.4087182634758,80.8859576775251));
#60633=CARTESIAN_POINT('Ctrl Pts',(16.248947338163,-15.3940656126707,80.8461713540943));
#60634=CARTESIAN_POINT('Ctrl Pts',(16.2554916800538,-15.388450767397,80.8301796061662));
#60635=CARTESIAN_POINT('Ctrl Pts',(16.2620326141532,-15.3832121080572,80.8140766685934));
#60636=CARTESIAN_POINT('Ctrl Pts',(16.2685609643578,-15.3783529418162,80.7978834589029));
#60637=CARTESIAN_POINT('Ctrl Pts',(16.2734481412606,-15.3748990742495,80.7856999038481));
#60638=CARTESIAN_POINT('Ctrl Pts',(16.2775147617408,-15.3721798545712,80.7755097810832));
#60639=CARTESIAN_POINT('Ctrl Pts',(16.2807580438145,-15.37010041347,80.7673524199429));
#60640=CARTESIAN_POINT('Ctrl Pts',(16.308363242307,-15.3529640814669,80.6977276874573));
#60641=CARTESIAN_POINT('Ctrl Pts',(16.3586107169648,-15.3376504708956,80.5654454852136));
#60642=CARTESIAN_POINT('Ctrl Pts',(16.4058754210574,-15.353224391122,80.4297068102671));
#60643=CARTESIAN_POINT('Ctrl Pts',(16.4308398851589,-15.371663215768,80.3544280421398));
#60644=CARTESIAN_POINT('Ctrl Pts',(16.4363274974597,-15.3760122112162,80.3377790265208));
#60645=CARTESIAN_POINT('Ctrl Pts',(16.4458365951828,-15.3843016285567,80.3086730273532));
#60646=CARTESIAN_POINT('Ctrl Pts',(16.4643631140139,-15.4034928690422,80.2509476732841));
#60647=CARTESIAN_POINT('Ctrl Pts',(16.4893053796703,-15.438486627179,80.1703295926858));
#60648=CARTESIAN_POINT('Ctrl Pts',(16.5162719674538,-15.4912042488478,80.0789622080761));
#60649=CARTESIAN_POINT('Ctrl Pts',(16.548100587601,-15.5753837738119,79.9659216531079));
#60650=CARTESIAN_POINT('Ctrl Pts',(16.5678845354643,-15.6528601133616,79.8907518590427));
#60651=CARTESIAN_POINT('Ctrl Pts',(16.5813766158318,-15.7228477592171,79.837607390227));
#60652=CARTESIAN_POINT('Ctrl Pts',(16.586544255709,-15.7515481629588,79.8170540818662));
#60653=CARTESIAN_POINT('Ctrl Pts',(16.5950312459286,-15.8037451346603,79.7828728219127));
#60654=CARTESIAN_POINT('Ctrl Pts',(16.6179955133542,-15.9782014756465,79.6876782461328));
#60655=CARTESIAN_POINT('Ctrl Pts',(16.6267263258151,-16.1627202519724,79.6478822388519));
#60656=CARTESIAN_POINT('Ctrl Pts',(16.6267263258151,-16.3,79.6478822388519));
#60657=CARTESIAN_POINT('Ctrl Pts',(16.5682685807363,-16.3,79.6794471094054));
#60658=CARTESIAN_POINT('Ctrl Pts',(16.5682685807363,-16.3654163455495,79.6794471094054));
#60659=CARTESIAN_POINT('Ctrl Pts',(16.5648757180916,-16.5015353380303,79.694032182584));
#60660=CARTESIAN_POINT('Ctrl Pts',(16.5488958565679,-16.6995167804338,79.7615628583216));
#60661=CARTESIAN_POINT('Ctrl Pts',(16.5212378223452,-16.8751412636049,79.8719303095954));
#60662=CARTESIAN_POINT('Ctrl Pts',(16.4855283482262,-17.0115529086637,80.0051425561287));
#60663=CARTESIAN_POINT('Ctrl Pts',(16.4446617185293,-17.1047465677694,80.1458899414884));
#60664=CARTESIAN_POINT('Ctrl Pts',(16.4114302680484,-17.1502813749753,80.2523393584253));
#60665=CARTESIAN_POINT('Ctrl Pts',(16.3913762782497,-17.1709658329303,80.3144713055844));
#60666=CARTESIAN_POINT('Ctrl Pts',(16.3391445888223,-17.212802991683,80.4725372675774));
#60667=CARTESIAN_POINT('Ctrl Pts',(16.2857314383956,-17.2125755498251,80.6192965971047));
#60668=CARTESIAN_POINT('Ctrl Pts',(16.2285468285878,-17.1749900192637,80.7633184910142));
#60669=CARTESIAN_POINT('Ctrl Pts',(16.2121886337196,-17.1625231491928,80.8039807456047));
#60670=CARTESIAN_POINT('Ctrl Pts',(16.1834234640797,-17.136226394498,80.8741331272979));
#60671=CARTESIAN_POINT('Ctrl Pts',(16.1429016478756,-17.0867325106556,80.9693909031479));
#60672=CARTESIAN_POINT('Ctrl Pts',(16.0968794814561,-17.0091364606193,81.0728790708405));
#60673=CARTESIAN_POINT('Ctrl Pts',(16.0432690220981,-16.8911461445725,81.1890821301941));
#60674=CARTESIAN_POINT('Ctrl Pts',(16.0057427089113,-16.7687693436075,81.2665286237563));
#60675=CARTESIAN_POINT('Ctrl Pts',(15.9841699591719,-16.6639283757204,81.3101794720153));
#60676=CARTESIAN_POINT('Ctrl Pts',(15.9762322885284,-16.6213185745115,81.3261691137268));
#60677=CARTESIAN_POINT('Ctrl Pts',(15.9676320881363,-16.5667941575919,81.3433802708799));
#60678=CARTESIAN_POINT('Ctrl Pts',(15.9609231695331,-16.5111375850943,81.3567164293632));
#60679=CARTESIAN_POINT('Ctrl Pts',(15.9567168958975,-16.4663676363709,81.3650506841189));
#60680=CARTESIAN_POINT('Ctrl Pts',(15.9481995036021,-16.3539097056676,81.3818802468179));
#60681=CARTESIAN_POINT('Ctrl Pts',(15.9481396643049,-16.2461392258156,81.3820180339724));
#60682=CARTESIAN_POINT('Ctrl Pts',(15.9566689590012,-16.1334781604,81.3651627338623));
#60683=CARTESIAN_POINT('Ctrl Pts',(15.9608681718556,-16.0887471014202,81.3568449343787));
#60684=CARTESIAN_POINT('Ctrl Pts',(15.9702940985485,-16.010769072521,81.3380998266106));
#60685=CARTESIAN_POINT('Ctrl Pts',(15.9930410676277,-15.8814905994934,81.2925184327966));
#60686=CARTESIAN_POINT('Ctrl Pts',(16.037301494618,-15.7249648889896,81.2015123159746));
#60687=CARTESIAN_POINT('Ctrl Pts',(16.0859404290664,-15.6114171611822,81.0971473460665));
#60688=CARTESIAN_POINT('Ctrl Pts',(16.1311604803816,-15.5323206091591,80.9959031187542));
#60689=CARTESIAN_POINT('Ctrl Pts',(16.1669722908724,-15.4826823083131,80.9131014175417));
#60690=CARTESIAN_POINT('Ctrl Pts',(16.1930779887927,-15.4547447293601,80.8506203445149));
#60691=CARTESIAN_POINT('Ctrl Pts',(16.2084486574181,-15.4409958898165,80.8130386258298));
#60692=CARTESIAN_POINT('Ctrl Pts',(16.2145968821216,-15.4357281896166,80.7979359159407));
#60693=CARTESIAN_POINT('Ctrl Pts',(16.2207421833459,-15.4308145520899,80.7827325176388));
#60694=CARTESIAN_POINT('Ctrl Pts',(16.2268760800755,-15.4262577968829,80.7674479311235));
#60695=CARTESIAN_POINT('Ctrl Pts',(16.2314682116025,-15.4230193091731,80.7559499558589));
#60696=CARTESIAN_POINT('Ctrl Pts',(16.2352895683688,-15.4204699796826,80.7463348096178));
#60697=CARTESIAN_POINT('Ctrl Pts',(16.2383373956163,-15.4185206273572,80.7386386127816));
#60698=CARTESIAN_POINT('Ctrl Pts',(16.2642801106568,-15.4024573292759,80.6729552053384));
#60699=CARTESIAN_POINT('Ctrl Pts',(16.3115338019764,-15.3881226139331,80.5483125449542));
#60700=CARTESIAN_POINT('Ctrl Pts',(16.3561406372079,-15.402700477352,80.420473057049));
#60701=CARTESIAN_POINT('Ctrl Pts',(16.3797750503189,-15.4199850482215,80.3495220710645));
#60702=CARTESIAN_POINT('Ctrl Pts',(16.3849723942331,-15.4240623312903,80.333828707121));
#60703=CARTESIAN_POINT('Ctrl Pts',(16.3939839669887,-15.4318353044674,80.3063891325602));
#60704=CARTESIAN_POINT('Ctrl Pts',(16.4115634184646,-15.4498377337239,80.2519501329241));
#60705=CARTESIAN_POINT('Ctrl Pts',(16.4352982169183,-15.4826946362818,80.1758553732025));
#60706=CARTESIAN_POINT('Ctrl Pts',(16.4610666145802,-15.5322722105491,80.0894872533015));
#60707=CARTESIAN_POINT('Ctrl Pts',(16.4916229143245,-15.6115905425624,79.9824438880594));
#60708=CARTESIAN_POINT('Ctrl Pts',(16.5107575130176,-15.6847896235666,79.911059408863));
#60709=CARTESIAN_POINT('Ctrl Pts',(16.5238646668574,-15.7510666283349,79.8604999384555));
#60710=CARTESIAN_POINT('Ctrl Pts',(16.5288909345617,-15.7782579295395,79.8409372899176));
#60711=CARTESIAN_POINT('Ctrl Pts',(16.5371589317105,-15.8277447844118,79.8083833966062));
#60712=CARTESIAN_POINT('Ctrl Pts',(16.559615074615,-15.9933446087463,79.7175907932137));
#60713=CARTESIAN_POINT('Ctrl Pts',(16.5682685807363,-16.169167308901,79.6794471094054));
#60714=CARTESIAN_POINT('Ctrl Pts',(16.5682685807363,-16.3,79.6794471094054));
#60715=CARTESIAN_POINT('Ctrl Pts',(16.5098108356574,-16.3,79.7110119799589));
#60716=CARTESIAN_POINT('Ctrl Pts',(16.5098108356574,-16.3621928170852,79.7110119799589));
#60717=CARTESIAN_POINT('Ctrl Pts',(16.5064619017735,-16.4916044553461,79.7249461869476));
#60718=CARTESIAN_POINT('Ctrl Pts',(16.4907347432034,-16.6794895188621,79.7893806340904));
#60719=CARTESIAN_POINT('Ctrl Pts',(16.4637563293615,-16.8455559377511,79.8943116367715));
#60720=CARTESIAN_POINT('Ctrl Pts',(16.4292587073893,-16.9739943824412,80.0204604098552));
#60721=CARTESIAN_POINT('Ctrl Pts',(16.3901764415961,-17.0613632104284,80.15320070383));
#60722=CARTESIAN_POINT('Ctrl Pts',(16.3586387967944,-17.1039309136449,80.2533172297057));
#60723=CARTESIAN_POINT('Ctrl Pts',(16.3396643898069,-17.1232514874083,80.3116995008137));
#60724=CARTESIAN_POINT('Ctrl Pts',(16.2903409178698,-17.1622948989398,80.4601451482957));
#60725=CARTESIAN_POINT('Ctrl Pts',(16.2402688803948,-17.1620743225282,80.5977221589703));
#60726=CARTESIAN_POINT('Ctrl Pts',(16.1867543224206,-17.1270000742741,80.7331266794945));
#60727=CARTESIAN_POINT('Ctrl Pts',(16.1714486021607,-17.1153596055406,80.771375190338));
#60728=CARTESIAN_POINT('Ctrl Pts',(16.1445383408925,-17.0907904968289,80.8374190309404));
#60729=CARTESIAN_POINT('Ctrl Pts',(16.1066278254269,-17.0444827594336,80.9272758215181));
#60730=CARTESIAN_POINT('Ctrl Pts',(16.0635316928428,-16.9716721295058,81.0252169897002));
#60731=CARTESIAN_POINT('Ctrl Pts',(16.0132651024235,-16.8606452050531,81.1355545468169));
#60732=CARTESIAN_POINT('Ctrl Pts',(15.9779917367264,-16.7450147427169,81.20948355231));
#60733=CARTESIAN_POINT('Ctrl Pts',(15.9576860589639,-16.6456586411203,81.2512577503319));
#60734=CARTESIAN_POINT('Ctrl Pts',(15.9502124412381,-16.605257770505,81.2665686151285));
#60735=CARTESIAN_POINT('Ctrl Pts',(15.9421112351274,-16.5535224004483,81.2830635159973));
#60736=CARTESIAN_POINT('Ctrl Pts',(15.9357885144715,-16.5006711287297,81.295856251176));
#60737=CARTESIAN_POINT('Ctrl Pts',(15.9318234322441,-16.4581386793206,81.3038544316465));
#60738=CARTESIAN_POINT('Ctrl Pts',(15.9237927519929,-16.3512744438455,81.3200115733789));
#60739=CARTESIAN_POINT('Ctrl Pts',(15.9237368277053,-16.2487724748305,81.3201416713976));
#60740=CARTESIAN_POINT('Ctrl Pts',(15.9317786349915,-16.1417151886103,81.3039601531045));
#60741=CARTESIAN_POINT('Ctrl Pts',(15.935737117663,-16.099219555577,81.2959774963651));
#60742=CARTESIAN_POINT('Ctrl Pts',(15.9446201826419,-16.025172521134,81.2779972477685));
#60743=CARTESIAN_POINT('Ctrl Pts',(15.9660449085761,-15.9025538758214,81.2343211007578));
#60744=CARTESIAN_POINT('Ctrl Pts',(16.0076601767798,-15.7545447026057,81.1474055568938));
#60745=CARTESIAN_POINT('Ctrl Pts',(16.0532833146667,-15.6476374842939,81.0482122821961));
#60746=CARTESIAN_POINT('Ctrl Pts',(16.0956344323365,-15.5733868874825,80.9523590140158));
#60747=CARTESIAN_POINT('Ctrl Pts',(16.1291484008924,-15.5268924738204,80.8741611128984));
#60748=CARTESIAN_POINT('Ctrl Pts',(16.153569975722,-15.5007711952445,80.8152830115046));
#60749=CARTESIAN_POINT('Ctrl Pts',(16.1679499766733,-15.4879261669622,80.7799058975652));
#60750=CARTESIAN_POINT('Ctrl Pts',(16.1737020841893,-15.4830056118361,80.765692225715));
#60751=CARTESIAN_POINT('Ctrl Pts',(16.1794517525386,-15.4784169961225,80.7513883666841));
#60752=CARTESIAN_POINT('Ctrl Pts',(16.1851911957931,-15.4741626519496,80.7370124033441));
#60753=CARTESIAN_POINT('Ctrl Pts',(16.1894882819445,-15.4711395440967,80.7262000078696));
#60754=CARTESIAN_POINT('Ctrl Pts',(16.1930643749967,-15.468760104794,80.7171598381523));
#60755=CARTESIAN_POINT('Ctrl Pts',(16.1959167474182,-15.4669408412445,80.7099248056204));
#60756=CARTESIAN_POINT('Ctrl Pts',(16.2201969790067,-15.4519505770849,80.6481827232194));
#60757=CARTESIAN_POINT('Ctrl Pts',(16.2644568869881,-15.4385947569706,80.5311796046948));
#60758=CARTESIAN_POINT('Ctrl Pts',(16.3064058533584,-15.4521765635819,80.411239303831));
#60759=CARTESIAN_POINT('Ctrl Pts',(16.3287102154788,-15.468306880675,80.3446160999893));
#60760=CARTESIAN_POINT('Ctrl Pts',(16.3336172910065,-15.4721124513644,80.3298783877211));
#60761=CARTESIAN_POINT('Ctrl Pts',(16.3421313387945,-15.4793689803781,80.3041052377673));
#60762=CARTESIAN_POINT('Ctrl Pts',(16.3587637229153,-15.4961825984056,80.2529525925641));
#60763=CARTESIAN_POINT('Ctrl Pts',(16.3812910541662,-15.5269026453845,80.1813811537191));
#60764=CARTESIAN_POINT('Ctrl Pts',(16.4058612617066,-15.5733401722504,80.100012298527));
#60765=CARTESIAN_POINT('Ctrl Pts',(16.4351452410481,-15.6477973113128,79.9989661230109));
#60766=CARTESIAN_POINT('Ctrl Pts',(16.4536304905709,-15.7167191337717,79.9313669586834));
#60767=CARTESIAN_POINT('Ctrl Pts',(16.466352717883,-15.7792854974526,79.8833924866841));
#60768=CARTESIAN_POINT('Ctrl Pts',(16.4712376134143,-15.8049676961202,79.8648204979691));
#60769=CARTESIAN_POINT('Ctrl Pts',(16.4792866174925,-15.8517444341634,79.8338939712997));
#60770=CARTESIAN_POINT('Ctrl Pts',(16.5012346358758,-16.0084877418461,79.7475033402946));
#60771=CARTESIAN_POINT('Ctrl Pts',(16.5098108356574,-16.1756143658296,79.7110119799589));
#60772=CARTESIAN_POINT('Ctrl Pts',(16.5098108356574,-16.3,79.7110119799589));
#60773=CARTESIAN_POINT('Ctrl Pts',(16.4513530905785,-16.3,79.7425768505124));
#60774=CARTESIAN_POINT('Ctrl Pts',(16.4513530905785,-16.3589692886209,79.7425768505124));
#60775=CARTESIAN_POINT('Ctrl Pts',(16.4480480854555,-16.4816735726619,79.7558601913112));
#60776=CARTESIAN_POINT('Ctrl Pts',(16.4325736298389,-16.6594622572905,79.8171984098592));
#60777=CARTESIAN_POINT('Ctrl Pts',(16.4062748363779,-16.8159706118973,79.9166929639477));
#60778=CARTESIAN_POINT('Ctrl Pts',(16.3729890665525,-16.9364358562187,80.0357782635816));
#60779=CARTESIAN_POINT('Ctrl Pts',(16.3356911646629,-17.0179798530874,80.1605114661715));
#60780=CARTESIAN_POINT('Ctrl Pts',(16.3058473255403,-17.0575804523145,80.254295100986));
#60781=CARTESIAN_POINT('Ctrl Pts',(16.2879525013642,-17.0755371418863,80.308927696043));
#60782=CARTESIAN_POINT('Ctrl Pts',(16.2415372469172,-17.1117868061966,80.447753029014));
#60783=CARTESIAN_POINT('Ctrl Pts',(16.1948063223941,-17.1115730952314,80.576147720836));
#60784=CARTESIAN_POINT('Ctrl Pts',(16.1449618162535,-17.0790101292845,80.7029348679748));
#60785=CARTESIAN_POINT('Ctrl Pts',(16.1307085706017,-17.0681960618883,80.7387696350713));
#60786=CARTESIAN_POINT('Ctrl Pts',(16.1056532177054,-17.0453545991598,80.800704934583));
#60787=CARTESIAN_POINT('Ctrl Pts',(16.0703540029782,-17.0022330082117,80.8851607398882));
#60788=CARTESIAN_POINT('Ctrl Pts',(16.0301839042296,-16.9342077983924,80.9775549085599));
#60789=CARTESIAN_POINT('Ctrl Pts',(15.9832611827489,-16.8301442655337,81.0820269634397));
#60790=CARTESIAN_POINT('Ctrl Pts',(15.9502407645414,-16.7212601418262,81.1524384808638));
#60791=CARTESIAN_POINT('Ctrl Pts',(15.9312021587559,-16.6273889065201,81.1923360286486));
#60792=CARTESIAN_POINT('Ctrl Pts',(15.9241925939478,-16.5891969664984,81.2069681165303));
#60793=CARTESIAN_POINT('Ctrl Pts',(15.9165903821184,-16.5402506433046,81.2227467611148));
#60794=CARTESIAN_POINT('Ctrl Pts',(15.91065385941,-16.4902046723651,81.2349960729889));
#60795=CARTESIAN_POINT('Ctrl Pts',(15.9069299685908,-16.4499097222704,81.2426581791741));
#60796=CARTESIAN_POINT('Ctrl Pts',(15.8993860003837,-16.3486391820234,81.2581428999399));
#60797=CARTESIAN_POINT('Ctrl Pts',(15.8993339911057,-16.2514057238454,81.2582653088229));
#60798=CARTESIAN_POINT('Ctrl Pts',(15.9068883109817,-16.1499522168206,81.2427575723468));
#60799=CARTESIAN_POINT('Ctrl Pts',(15.9106060634705,-16.1096920097338,81.2351100583515));
#60800=CARTESIAN_POINT('Ctrl Pts',(15.9189462667354,-16.039575969747,81.2178946689264));
#60801=CARTESIAN_POINT('Ctrl Pts',(15.9390487495246,-15.9236171521494,81.176123768719));
#60802=CARTESIAN_POINT('Ctrl Pts',(15.9780188589416,-15.7841245162218,81.093298797813));
#60803=CARTESIAN_POINT('Ctrl Pts',(16.0206262002669,-15.6838578074055,80.9992772183258));
#60804=CARTESIAN_POINT('Ctrl Pts',(16.0601083842914,-15.614453165806,80.9088149092774));
#60805=CARTESIAN_POINT('Ctrl Pts',(16.0913245109124,-15.5711026393277,80.8352208082551));
#60806=CARTESIAN_POINT('Ctrl Pts',(16.1140619626514,-15.5467976611288,80.7799456784944));
#60807=CARTESIAN_POINT('Ctrl Pts',(16.1274512959284,-15.5348564441079,80.7467731693007));
#60808=CARTESIAN_POINT('Ctrl Pts',(16.1328072862571,-15.5302830340556,80.7334485354894));
#60809=CARTESIAN_POINT('Ctrl Pts',(16.1381613217313,-15.5260194401552,80.7200442157294));
#60810=CARTESIAN_POINT('Ctrl Pts',(16.1435063115107,-15.5220675070163,80.7065768755647));
#60811=CARTESIAN_POINT('Ctrl Pts',(16.1475083522864,-15.5192597790203,80.6964500598804));
#60812=CARTESIAN_POINT('Ctrl Pts',(16.1508391816247,-15.5170502299053,80.6879848666869));
#60813=CARTESIAN_POINT('Ctrl Pts',(16.15349609922,-15.5153610551317,80.6812109984591));
#60814=CARTESIAN_POINT('Ctrl Pts',(16.1761138473566,-15.5014438248939,80.6234102411006));
#60815=CARTESIAN_POINT('Ctrl Pts',(16.2173799719997,-15.4890669000081,80.5140466644355));
#60816=CARTESIAN_POINT('Ctrl Pts',(16.256671069509,-15.5016526498119,80.4020055506128));
#60817=CARTESIAN_POINT('Ctrl Pts',(16.2776453806387,-15.5166287131285,80.339710128914));
#60818=CARTESIAN_POINT('Ctrl Pts',(16.2822621877799,-15.5201625714385,80.3259280683213));
#60819=CARTESIAN_POINT('Ctrl Pts',(16.2902787106003,-15.5269026562889,80.3018213429743));
#60820=CARTESIAN_POINT('Ctrl Pts',(16.3059640273659,-15.5425274630872,80.253955052204));
#60821=CARTESIAN_POINT('Ctrl Pts',(16.3272838914141,-15.5711106544873,80.1869069342357));
#60822=CARTESIAN_POINT('Ctrl Pts',(16.3506559088329,-15.6144081339517,80.1105373437524));
#60823=CARTESIAN_POINT('Ctrl Pts',(16.3786675677716,-15.6840040800632,80.0154883579624));
#60824=CARTESIAN_POINT('Ctrl Pts',(16.3965034681242,-15.7486486439767,79.9516745085037));
#60825=CARTESIAN_POINT('Ctrl Pts',(16.4088407689086,-15.8075043665704,79.9062850349126));
#60826=CARTESIAN_POINT('Ctrl Pts',(16.413584292267,-15.8316774627009,79.8887037060206));
#60827=CARTESIAN_POINT('Ctrl Pts',(16.4214143032745,-15.8757440839149,79.8594045459933));
#60828=CARTESIAN_POINT('Ctrl Pts',(16.4428541971365,-16.0236308749458,79.7774158873755));
#60829=CARTESIAN_POINT('Ctrl Pts',(16.4513530905785,-16.1820614227582,79.7425768505124));
#60830=CARTESIAN_POINT('Ctrl Pts',(16.4513530905785,-16.3,79.7425768505124));
#60831=CARTESIAN_POINT('',(16.6267263258151,-16.3,79.647882238852));
#60832=CARTESIAN_POINT('Origin',(10.315,-23.44,78.));
#60833=CARTESIAN_POINT('Origin',(10.315,-23.44,78.));
#60834=CARTESIAN_POINT('Origin',(12.3125,-18.7,78.));
#60835=CARTESIAN_POINT('Origin',(9.31,-14.1,78.));
#60836=CARTESIAN_POINT('',(6.2075,-14.05,78.));
#60837=CARTESIAN_POINT('',(6.2575,-14.1,78.));
#60838=CARTESIAN_POINT('Origin',(9.31,-14.05,78.));
#60839=CARTESIAN_POINT('Origin',(16.61,-14.05,78.));
#60840=CARTESIAN_POINT('',(2.01,-14.05,78.));
#60841=CARTESIAN_POINT('Origin',(9.31,-14.05,78.));
#60842=CARTESIAN_POINT('Origin',(9.31,-14.15,78.));
#60843=CARTESIAN_POINT('',(1.91,-14.15,78.));
#60844=CARTESIAN_POINT('Origin',(9.31,-25.4,78.));
#60845=CARTESIAN_POINT('',(1.91,-25.4,78.));
#60846=CARTESIAN_POINT('',(0.,0.,0.));
#60847=CARTESIAN_POINT('Origin',(4.42952305344106,-2.25,78.7389695278488));
#60848=CARTESIAN_POINT('',(4.42952305344106,4.42047694655894,78.7389695278488));
#60849=CARTESIAN_POINT('',(4.5,4.35,78.8396210385982));
#60850=CARTESIAN_POINT('',(1.84616051607008,7.00383948392992,75.04954546941));
#60851=CARTESIAN_POINT('',(4.5,-4.35,78.8396210385982));
#60852=CARTESIAN_POINT('',(4.5,-2.25,78.8396210385982));
#60853=CARTESIAN_POINT('',(4.42952305344105,-4.42047694655895,78.7389695278488));
#60854=CARTESIAN_POINT('',(1.2891756037128,-7.56082439628721,74.2540885770415));
#60855=CARTESIAN_POINT('',(4.35904610688211,-4.35,78.6383180170993));
#60856=CARTESIAN_POINT('',(2.71496575386869,-2.70591964698626,76.2903279380192));
#60857=CARTESIAN_POINT('',(4.35904610688211,4.35,78.6383180170993));
#60858=CARTESIAN_POINT('',(4.35904610688211,-2.25,78.6383180170993));
#60859=CARTESIAN_POINT('',(2.90546581342326,2.89641970654102,76.5623902183564));
#60860=CARTESIAN_POINT('Origin',(0.709236498419204,4.425,77.3897092918157));
#60861=CARTESIAN_POINT('',(3.15,4.35,78.1982612223388));
#60862=CARTESIAN_POINT('',(0.734888009168629,4.35,77.3192323452568));
#60863=CARTESIAN_POINT('',(3.,4.5,78.3032923530703));
#60864=CARTESIAN_POINT('',(4.07348426223018,3.42651573776982,77.5516305805072));
#60865=CARTESIAN_POINT('',(4.35,4.5,78.7946521693296));
#60866=CARTESIAN_POINT('',(0.683584987669779,4.5,77.4601862383747));
#60867=CARTESIAN_POINT('',(6.57988693089012,2.27011306910988,77.2332685309651));
#60868=CARTESIAN_POINT('Origin',(3.15,0.,78.1982612223388));
#60869=CARTESIAN_POINT('',(3.15,-4.35,78.1982612223388));
#60870=CARTESIAN_POINT('',(-3.23871198784907,-4.35,75.8729602234621));
#60871=CARTESIAN_POINT('',(3.15,0.,78.1982612223388));
#60872=CARTESIAN_POINT('Origin',(-3.26436349859849,-4.425,75.943437170021));
#60873=CARTESIAN_POINT('',(4.35,-4.5,78.7946521693296));
#60874=CARTESIAN_POINT('',(5.98539619974414,-2.86460380025586,77.6495354223095));
#60875=CARTESIAN_POINT('',(3.,-4.5,78.3032923530702));
#60876=CARTESIAN_POINT('',(-3.29001500934791,-4.5,76.01391411658));
#60877=CARTESIAN_POINT('',(3.,-4.5,78.3032923530702));
#60878=CARTESIAN_POINT('Origin',(4.42952305344106,-2.25,95.7035698572336));
#60879=CARTESIAN_POINT('',(4.42952305344105,4.42047694655895,95.7035698572336));
#60880=CARTESIAN_POINT('',(4.5,4.35,95.8042213679831));
#60881=CARTESIAN_POINT('',(-1.1526413191047,10.0026413191047,87.7314129352752));
#60882=CARTESIAN_POINT('',(4.5,-4.35,95.8042213679831));
#60883=CARTESIAN_POINT('',(4.5,-2.25,95.8042213679831));
#60884=CARTESIAN_POINT('',(4.42952305344106,-4.42047694655894,95.7035698572336));
#60885=CARTESIAN_POINT('',(-1.70962623146198,-10.559626231462,86.9359560429067));
#60886=CARTESIAN_POINT('',(4.35904610688212,-4.35,95.6029183464842));
#60887=CARTESIAN_POINT('',(2.2021404371328,-2.19309433025049,92.5225378135008));
#60888=CARTESIAN_POINT('',(4.35904610688211,4.35,95.6029183464842));
#60889=CARTESIAN_POINT('',(4.35904610688211,-2.25,95.6029183464842));
#60890=CARTESIAN_POINT('',(2.39264049668742,2.38359438980513,92.794600093838));
#60891=CARTESIAN_POINT('Origin',(-2.01692222533399,4.425,93.3620689918693));
#60892=CARTESIAN_POINT('',(3.15,4.35,95.1628615517237));
#60893=CARTESIAN_POINT('',(-1.99127071458457,4.35,93.2915920453104));
#60894=CARTESIAN_POINT('',(3.,4.5,95.2678926824551));
#60895=CARTESIAN_POINT('',(4.85812886689736,2.64187113310263,93.9668168428886));
#60896=CARTESIAN_POINT('',(4.35,4.5,95.7592524987145));
#60897=CARTESIAN_POINT('',(-2.04257373608342,4.5,93.4325459384283));
#60898=CARTESIAN_POINT('',(8.55703704573063,0.292962954269369,92.8134534457666));
#60899=CARTESIAN_POINT('Origin',(3.15,0.,95.1628615517237));
#60900=CARTESIAN_POINT('',(3.15,-4.35,95.1628615517237));
#60901=CARTESIAN_POINT('',(-5.96487071160227,-4.35,91.8453199235157));
#60902=CARTESIAN_POINT('',(3.15,0.,95.1628615517237));
#60903=CARTESIAN_POINT('Origin',(-5.99052222235169,-4.425,91.9157968700746));
#60904=CARTESIAN_POINT('',(4.35,-4.5,95.7592524987145));
#60905=CARTESIAN_POINT('',(7.96254631458501,-0.887453685414986,93.2297203371105));
#60906=CARTESIAN_POINT('',(3.,-4.5,95.2678926824551));
#60907=CARTESIAN_POINT('',(-6.01617373310111,-4.5,91.9862738166335));
#60908=CARTESIAN_POINT('',(3.,-4.5,95.2678926824551));
#60909=CARTESIAN_POINT('Origin',(4.42952305344106,-2.25,112.668170186619));
#60910=CARTESIAN_POINT('',(4.42952305344106,4.42047694655894,112.668170186619));
#60911=CARTESIAN_POINT('',(4.5,4.35,112.768821697368));
#60912=CARTESIAN_POINT('',(-4.15144315427948,13.0014431542795,100.41328040114));
#60913=CARTESIAN_POINT('',(4.5,-4.35,112.768821697368));
#60914=CARTESIAN_POINT('',(4.5,-2.25,112.768821697368));
#60915=CARTESIAN_POINT('',(4.42952305344106,-4.42047694655895,112.668170186619));
#60916=CARTESIAN_POINT('',(-4.70842806663676,-13.5584280666368,99.6178235087719));
#60917=CARTESIAN_POINT('',(4.35904610688211,-4.35,112.567518675869));
#60918=CARTESIAN_POINT('',(1.68931512039689,-1.68026901351456,108.754747688982));
#60919=CARTESIAN_POINT('',(4.35904610688211,4.35,112.567518675869));
#60920=CARTESIAN_POINT('',(4.35904610688211,-2.25,112.567518675869));
#60921=CARTESIAN_POINT('',(1.87981517995153,1.87076907306921,109.02680996932));
#60922=CARTESIAN_POINT('Origin',(3.15,0.,112.127461881109));
#60923=CARTESIAN_POINT('',(3.15,-4.35,112.127461881109));
#60924=CARTESIAN_POINT('',(-8.69102943535563,-4.35,107.817679623569));
#60925=CARTESIAN_POINT('',(3.15,4.35,112.127461881109));
#60926=CARTESIAN_POINT('',(3.15,0.,112.127461881109));
#60927=CARTESIAN_POINT('',(-4.71742943833795,4.35,109.263951745364));
#60928=CARTESIAN_POINT('Origin',(-8.71668094610505,-4.425,107.888156570128));
#60929=CARTESIAN_POINT('',(4.35,-4.5,112.723852828099));
#60930=CARTESIAN_POINT('',(9.93969642942553,1.08969642942552,108.809905251912));
#60931=CARTESIAN_POINT('',(3.,-4.5,112.23249301184));
#60932=CARTESIAN_POINT('',(-8.74233245685448,-4.5,107.958633516687));
#60933=CARTESIAN_POINT('',(3.,-4.5,112.23249301184));
#60934=CARTESIAN_POINT('Origin',(4.425,-4.425,59.4601776313845));
#60935=CARTESIAN_POINT('',(4.5,-4.35,112.974535212325));
#60936=CARTESIAN_POINT('',(4.5,-4.35,59.4601776313845));
#60937=CARTESIAN_POINT('',(4.42952305344105,-4.42047694655896,113.075186723075));
#60938=CARTESIAN_POINT('',(14.1744814719277,5.32448147192768,99.1579437819278));
#60939=CARTESIAN_POINT('',(4.35,-4.5,113.019504081594));
#60940=CARTESIAN_POINT('',(-2.40533103406217,-11.2553310340622,108.289370368442));
#60941=CARTESIAN_POINT('',(4.35,-4.5,59.4601776313845));
#60942=CARTESIAN_POINT('Origin',(4.42952305344106,-2.25,118.32303696308));
#60943=CARTESIAN_POINT('',(4.42952305344106,4.42047694655894,118.32303696308));
#60944=CARTESIAN_POINT('',(4.5,4.35,118.42368847383));
#60945=CARTESIAN_POINT('',(-5.1510437660044,14.0010437660044,104.640569556429));
#60946=CARTESIAN_POINT('',(4.5,-4.35,118.42368847383));
#60947=CARTESIAN_POINT('',(4.5,-2.25,118.42368847383));
#60948=CARTESIAN_POINT('',(4.42952305344105,-4.42047694655895,118.32303696308));
#60949=CARTESIAN_POINT('',(-5.70802867836169,-14.5580286783617,103.845112664061));
#60950=CARTESIAN_POINT('',(4.35904610688211,-4.35,118.222385452331));
#60951=CARTESIAN_POINT('',(1.51837334815156,-1.50932724126927,114.165484314143));
#60952=CARTESIAN_POINT('',(4.35904610688211,4.35,118.222385452331));
#60953=CARTESIAN_POINT('',(4.35904610688211,-2.25,118.222385452331));
#60954=CARTESIAN_POINT('',(1.70887340770616,1.69982730082414,114.43754659448));
#60955=CARTESIAN_POINT('Origin',(-5.6518005236718,4.425,114.658548591941));
#60956=CARTESIAN_POINT('',(3.15,4.35,117.78232865757));
#60957=CARTESIAN_POINT('',(-5.62614901292237,4.35,114.588071645382));
#60958=CARTESIAN_POINT('',(3.,4.5,117.887359788302));
#60959=CARTESIAN_POINT('',(5.90432167312078,1.5956783268792,115.853731859396));
#60960=CARTESIAN_POINT('',(4.35,4.5,118.378719604561));
#60961=CARTESIAN_POINT('',(-5.67745203442123,4.5,114.7290255385));
#60962=CARTESIAN_POINT('',(11.1932371988523,-2.34323719885225,113.587033332167));
#60963=CARTESIAN_POINT('Origin',(3.15,0.,117.78232865757));
#60964=CARTESIAN_POINT('',(3.15,-4.35,117.78232865757));
#60965=CARTESIAN_POINT('',(-9.59974900994005,-4.35,113.141799523587));
#60966=CARTESIAN_POINT('',(3.15,0.,117.78232865757));
#60967=CARTESIAN_POINT('Origin',(-9.62540052068947,-4.425,113.212276470146));
#60968=CARTESIAN_POINT('',(4.35,-4.5,118.378719604561));
#60969=CARTESIAN_POINT('',(10.5987464677057,1.74874646770573,114.003300223512));
#60970=CARTESIAN_POINT('',(3.,-4.5,117.887359788302));
#60971=CARTESIAN_POINT('',(-9.6510520314389,-4.5,113.282753416705));
#60972=CARTESIAN_POINT('',(3.,-4.5,117.887359788302));
#60973=CARTESIAN_POINT('Origin',(4.42952305344106,-2.25,99.4734810415414));
#60974=CARTESIAN_POINT('',(4.42952305344106,4.42047694655894,99.4734810415414));
#60975=CARTESIAN_POINT('',(4.5,4.35,99.5741325522908));
#60976=CARTESIAN_POINT('',(-1.81904172692132,10.6690417269213,90.5496057054675));
#60977=CARTESIAN_POINT('',(4.5,-4.35,99.5741325522908));
#60978=CARTESIAN_POINT('',(4.5,-2.25,99.5741325522908));
#60979=CARTESIAN_POINT('',(4.42952305344106,-4.42047694655894,99.4734810415414));
#60980=CARTESIAN_POINT('',(-2.3760266392786,-11.2260266392786,89.754148813099));
#60981=CARTESIAN_POINT('',(4.35904610688212,-4.35,99.372829530792));
#60982=CARTESIAN_POINT('',(2.08817925563595,-2.07913314875362,96.1296955636079));
#60983=CARTESIAN_POINT('',(4.35904610688211,4.35,99.372829530792));
#60984=CARTESIAN_POINT('',(4.35904610688211,-2.25,99.372829530792));
#60985=CARTESIAN_POINT('',(2.27867931519057,2.26963320830827,96.4017578439451));
#60986=CARTESIAN_POINT('Origin',(4.5,-4.5,59.4601776313845));
#60987=CARTESIAN_POINT('',(4.5,4.35,99.7798460672483));
#60988=CARTESIAN_POINT('',(4.5,4.35,59.4601776313845));
#60989=CARTESIAN_POINT('',(4.5,-4.35,99.7798460672483));
#60990=CARTESIAN_POINT('',(4.5,-2.25,99.7798460672483));
#60991=CARTESIAN_POINT('',(4.5,-4.35,59.4601776313845));
#60992=CARTESIAN_POINT('Origin',(4.425,4.425,59.4601776313845));
#60993=CARTESIAN_POINT('',(4.35,4.5,99.5291636830223));
#60994=CARTESIAN_POINT('',(8.99640373791744,-0.146403737917441,96.2757167601669));
#60995=CARTESIAN_POINT('',(4.35,4.5,99.8248149365169));
#60996=CARTESIAN_POINT('',(4.35,4.5,59.4601776313845));
#60997=CARTESIAN_POINT('',(4.42952305344105,4.42047694655895,99.8804975779977));
#60998=CARTESIAN_POINT('',(-0.273056880261707,9.12305688026171,96.5877156593865));
#60999=CARTESIAN_POINT('',(12.3990649569269,-3.54906495692689,88.4988121938873));
#61000=CARTESIAN_POINT('Origin',(-2.62273527505693,4.425,96.9114822585479));
#61001=CARTESIAN_POINT('',(3.15,4.35,98.9327727360315));
#61002=CARTESIAN_POINT('',(-2.5970837643075,4.35,96.841005311989));
#61003=CARTESIAN_POINT('',(3.,4.5,99.0378038667629));
#61004=CARTESIAN_POINT('',(3.15,4.35,98.9327727360315));
#61005=CARTESIAN_POINT('',(-2.64838678580635,4.5,96.9819592051068));
#61006=CARTESIAN_POINT('Origin',(4.42952305344106,-2.25,97.9955419858439));
#61007=CARTESIAN_POINT('',(4.42952305344105,-4.42047694655895,97.9955419858439));
#61008=CARTESIAN_POINT('',(4.5,-4.35,97.8948904750944));
#61009=CARTESIAN_POINT('',(11.5088798406612,2.65887984066121,87.8851727011587));
#61010=CARTESIAN_POINT('',(4.5,4.35,97.8948904750944));
#61011=CARTESIAN_POINT('',(4.5,-2.25,97.8948904750944));
#61012=CARTESIAN_POINT('',(4.42952305344105,4.42047694655894,97.9955419858439));
#61013=CARTESIAN_POINT('',(12.0658647530185,-3.2158647530185,87.0897158087902));
#61014=CARTESIAN_POINT('',(4.35904610688211,4.35,98.0961934965933));
#61015=CARTESIAN_POINT('',(4.78481711861775,4.77577101173567,97.4881294748544));
#61016=CARTESIAN_POINT('',(4.35904610688211,-4.35,98.0961934965933));
#61017=CARTESIAN_POINT('',(4.35904610688211,-2.25,98.0961934965933));
#61018=CARTESIAN_POINT('',(4.59431705906312,-4.58527095218102,97.7601917551917));
#61019=CARTESIAN_POINT('Origin',(10.699792324063,4.425,95.7085372775677));
#61020=CARTESIAN_POINT('',(4.35,4.5,97.939859344363));
#61021=CARTESIAN_POINT('',(-0.0533735341695696,8.90337353416957,94.8565840021845));
#61022=CARTESIAN_POINT('',(3.,4.5,98.4312191606224));
#61023=CARTESIAN_POINT('',(10.6741408133136,4.5,95.6380603310088));
#61024=CARTESIAN_POINT('',(3.15,4.35,98.5362502913538));
#61025=CARTESIAN_POINT('',(3.15,4.35,98.5362502913538));
#61026=CARTESIAN_POINT('',(10.7254438348125,4.35,95.7790142241267));
#61027=CARTESIAN_POINT('Origin',(4.425,4.425,59.4601776313845));
#61028=CARTESIAN_POINT('',(4.5,4.35,97.689176960137));
#61029=CARTESIAN_POINT('',(4.5,4.35,59.4601776313845));
#61030=CARTESIAN_POINT('',(4.42952305344105,4.42047694655894,97.5885254493875));
#61031=CARTESIAN_POINT('',(-1.48584152301308,10.3358415230131,89.1405093203705));
#61032=CARTESIAN_POINT('',(4.35,4.5,97.6442080908684));
#61033=CARTESIAN_POINT('',(8.77672039182401,0.0732796081759872,94.5445851029668));
#61034=CARTESIAN_POINT('',(4.35,4.5,59.4601776313845));
#61035=CARTESIAN_POINT('Origin',(4.5,-4.5,59.4601776313845));
#61036=CARTESIAN_POINT('',(4.5,-4.35,97.689176960137));
#61037=CARTESIAN_POINT('',(4.5,-4.35,59.4601776313845));
#61038=CARTESIAN_POINT('',(4.5,-2.25,97.689176960137));
#61039=CARTESIAN_POINT('Origin',(4.42952305344106,-2.25,97.5885254493875));
#61040=CARTESIAN_POINT('',(4.42952305344106,-4.42047694655894,97.5885254493875));
#61041=CARTESIAN_POINT('',(-2.04282643537031,-10.8928264353703,88.3450524280019));
#61042=CARTESIAN_POINT('',(4.35904610688211,-4.35,97.4878739386381));
#61043=CARTESIAN_POINT('',(2.14515984638464,-2.13611373950202,94.3261166885544));
#61044=CARTESIAN_POINT('',(4.35904610688212,4.35,97.4878739386381));
#61045=CARTESIAN_POINT('',(4.35904610688212,-2.25,97.4878739386381));
#61046=CARTESIAN_POINT('',(2.33565990593919,2.3266137990566,94.5981789688915));
#61047=CARTESIAN_POINT('Origin',(-2.31982875019547,4.425,95.1367756252086));
#61048=CARTESIAN_POINT('',(3.15,4.35,97.0478171438776));
#61049=CARTESIAN_POINT('',(-2.29417723944604,4.35,95.0662986786497));
#61050=CARTESIAN_POINT('',(3.,4.5,97.152848274609));
#61051=CARTESIAN_POINT('',(3.15,4.35,97.0478171438776));
#61052=CARTESIAN_POINT('',(-2.34548026094489,4.5,95.2072525717676));
#61053=CARTESIAN_POINT('Origin',(4.42952305344106,-2.25,96.11058639369));
#61054=CARTESIAN_POINT('',(4.42952305344106,-4.42047694655894,96.11058639369));
#61055=CARTESIAN_POINT('',(4.5,-4.35,96.0099348829406));
#61056=CARTESIAN_POINT('',(11.1756796367529,2.3256796367529,86.4760763160626));
#61057=CARTESIAN_POINT('',(4.5,4.35,96.0099348829406));
#61058=CARTESIAN_POINT('',(4.5,-2.25,96.0099348829406));
#61059=CARTESIAN_POINT('',(4.42952305344105,4.42047694655895,96.11058639369));
#61060=CARTESIAN_POINT('',(11.7326645491102,-2.88266454911019,85.680619423694));
#61061=CARTESIAN_POINT('',(4.35904610688211,4.35,96.2112379044394));
#61062=CARTESIAN_POINT('',(4.72783652786931,4.71879042098724,95.6845505998009));
#61063=CARTESIAN_POINT('',(4.35904610688211,-4.35,96.2112379044394));
#61064=CARTESIAN_POINT('',(4.35904610688211,-2.25,96.2112379044394));
#61065=CARTESIAN_POINT('',(4.53733646831466,-4.52829036143257,95.9566128801382));
#61066=CARTESIAN_POINT('Origin',(4.55,0.,96.1417363712273));
#61067=CARTESIAN_POINT('',(3.15,4.35,96.6512946992));
#61068=CARTESIAN_POINT('',(10.422537309951,4.35,94.0043075907874));
#61069=CARTESIAN_POINT('',(3.15,-4.35,96.6512946992));
#61070=CARTESIAN_POINT('',(3.15,0.,96.6512946992));
#61071=CARTESIAN_POINT('',(6.44893731293329,-4.35,95.4505797125821));
#61072=CARTESIAN_POINT('Origin',(10.3968857992016,4.425,93.9338306442285));
#61073=CARTESIAN_POINT('',(4.35,4.5,96.0549037522091));
#61074=CARTESIAN_POINT('',(0.16630981192384,8.68369018807616,93.1254523449844));
#61075=CARTESIAN_POINT('',(3.,4.5,96.5462635684685));
#61076=CARTESIAN_POINT('',(10.3712342884521,4.5,93.8633536976695));
#61077=CARTESIAN_POINT('',(3.15,4.35,96.6512946992));
#61078=CARTESIAN_POINT('Origin',(4.425,4.425,59.4601776313845));
#61079=CARTESIAN_POINT('',(4.35,4.5,59.4601776313845));
#61080=CARTESIAN_POINT('',(4.5,4.35,59.4601776313845));
#61081=CARTESIAN_POINT('Origin',(4.42952305344105,-2.25,82.5088807121565));
#61082=CARTESIAN_POINT('',(4.42952305344105,4.42047694655895,82.5088807121565));
#61083=CARTESIAN_POINT('',(4.5,4.35,82.6095322229059));
#61084=CARTESIAN_POINT('',(1.17976010825354,7.67023989174646,77.8677382396028));
#61085=CARTESIAN_POINT('',(4.5,-4.35,82.6095322229059));
#61086=CARTESIAN_POINT('',(4.5,-2.25,82.6095322229059));
#61087=CARTESIAN_POINT('',(4.42952305344105,-4.42047694655895,82.5088807121565));
#61088=CARTESIAN_POINT('',(0.622775195896197,-8.2272248041038,77.0722813472343));
#61089=CARTESIAN_POINT('',(4.35904610688211,-4.35,82.4082292014071));
#61090=CARTESIAN_POINT('',(2.60100457237156,-2.59195846548954,79.8974856881262));
#61091=CARTESIAN_POINT('',(4.35904610688211,4.35,82.4082292014071));
#61092=CARTESIAN_POINT('',(4.35904610688211,-2.25,82.4082292014071));
#61093=CARTESIAN_POINT('',(2.79150463192627,2.78245852504406,80.1695479684634));
#61094=CARTESIAN_POINT('Origin',(4.5,-4.5,59.4601776313845));
#61095=CARTESIAN_POINT('',(4.5,4.35,82.8152457378634));
#61096=CARTESIAN_POINT('',(4.5,4.35,59.4601776313845));
#61097=CARTESIAN_POINT('',(4.5,-4.35,82.8152457378634));
#61098=CARTESIAN_POINT('',(4.5,-2.25,82.8152457378634));
#61099=CARTESIAN_POINT('',(4.5,-4.35,59.4601776313845));
#61100=CARTESIAN_POINT('Origin',(4.425,4.425,59.4601776313845));
#61101=CARTESIAN_POINT('',(4.35,4.5,82.5645633536374));
#61102=CARTESIAN_POINT('',(7.0192536230765,1.8307463769235,80.695531845366));
#61103=CARTESIAN_POINT('',(4.35,4.5,82.860214607132));
#61104=CARTESIAN_POINT('',(4.35,4.5,59.4601776313845));
#61105=CARTESIAN_POINT('',(4.42952305344106,4.42047694655894,82.9158972486129));
#61106=CARTESIAN_POINT('',(1.70409323457756,7.14590676542244,81.0075307445832));
#61107=CARTESIAN_POINT('',(9.40026312175203,-0.550263121752025,75.8169447280211));
#61108=CARTESIAN_POINT('Origin',(0.103423448696272,4.425,80.9391225584943));
#61109=CARTESIAN_POINT('',(3.15,4.35,81.9681724066466));
#61110=CARTESIAN_POINT('',(0.129074959445692,4.35,80.8686456119354));
#61111=CARTESIAN_POINT('',(3.,4.5,82.073203537378));
#61112=CARTESIAN_POINT('',(3.15,4.35,81.9681724066466));
#61113=CARTESIAN_POINT('',(0.0777719379468511,4.5,81.0095995050532));
#61114=CARTESIAN_POINT('Origin',(4.42952305344106,-2.25,81.030941656459));
#61115=CARTESIAN_POINT('',(4.42952305344105,-4.42047694655895,81.030941656459));
#61116=CARTESIAN_POINT('',(4.5,-4.35,80.9302901457095));
#61117=CARTESIAN_POINT('',(8.51007800548643,-0.339921994513569,75.2033052352935));
#61118=CARTESIAN_POINT('',(4.5,4.35,80.9302901457095));
#61119=CARTESIAN_POINT('',(4.5,-2.25,80.9302901457095));
#61120=CARTESIAN_POINT('',(4.42952305344106,4.42047694655894,81.030941656459));
#61121=CARTESIAN_POINT('',(9.06706291784371,-0.217062917843715,74.4078483429249));
#61122=CARTESIAN_POINT('',(4.35904610688211,4.35,81.1315931672084));
#61123=CARTESIAN_POINT('',(4.2719918018819,4.26294569499977,81.2559195993728));
#61124=CARTESIAN_POINT('',(4.35904610688212,-4.35,81.1315931672084));
#61125=CARTESIAN_POINT('',(4.35904610688211,-2.25,81.1315931672084));
#61126=CARTESIAN_POINT('',(4.08149174232726,-4.07244563544511,81.52798187971));
#61127=CARTESIAN_POINT('Origin',(7.97363360030984,4.425,79.7361775775141));
#61128=CARTESIAN_POINT('',(4.35,4.5,80.9752590149781));
#61129=CARTESIAN_POINT('',(1.92377658067096,6.92622341932904,79.2763990873831));
#61130=CARTESIAN_POINT('',(3.,4.5,81.4666188312375));
#61131=CARTESIAN_POINT('',(7.94798208956041,4.5,79.6657006309552));
#61132=CARTESIAN_POINT('',(3.15,4.35,81.5716499619689));
#61133=CARTESIAN_POINT('',(3.15,4.35,81.5716499619689));
#61134=CARTESIAN_POINT('',(7.99928511105926,4.35,79.8066545240731));
#61135=CARTESIAN_POINT('Origin',(4.425,4.425,59.4601776313845));
#61136=CARTESIAN_POINT('',(4.5,4.35,80.7245766307521));
#61137=CARTESIAN_POINT('',(4.5,4.35,59.4601776313845));
#61138=CARTESIAN_POINT('',(4.42952305344105,4.42047694655894,80.6239251200027));
#61139=CARTESIAN_POINT('',(1.51296031216177,7.33703968783823,76.4586418545061));
#61140=CARTESIAN_POINT('',(4.35,4.5,80.6796077614835));
#61141=CARTESIAN_POINT('',(6.7995702769835,2.0504297230165,78.9644001881653));
#61142=CARTESIAN_POINT('',(4.35,4.5,59.4601776313845));
#61143=CARTESIAN_POINT('Origin',(4.5,-4.5,59.4601776313845));
#61144=CARTESIAN_POINT('',(4.5,-4.35,80.7245766307521));
#61145=CARTESIAN_POINT('',(4.5,-4.35,59.4601776313845));
#61146=CARTESIAN_POINT('',(4.5,-2.25,80.7245766307521));
#61147=CARTESIAN_POINT('Origin',(4.42952305344106,-2.25,80.6239251200027));
#61148=CARTESIAN_POINT('',(4.42952305344105,-4.42047694655895,80.6239251200026));
#61149=CARTESIAN_POINT('',(0.955975399804484,-7.89402460019551,75.6631849621376));
#61150=CARTESIAN_POINT('',(4.35904610688211,-4.35,80.5232736092532));
#61151=CARTESIAN_POINT('',(2.65798516312021,-2.64893905623794,78.0939068130727));
#61152=CARTESIAN_POINT('',(4.35904610688211,4.35,80.5232736092532));
#61153=CARTESIAN_POINT('',(4.35904610688211,-2.25,80.5232736092532));
#61154=CARTESIAN_POINT('',(2.84848522267484,2.83943911579257,78.3659690934099));
#61155=CARTESIAN_POINT('Origin',(0.406329973557735,4.425,79.164415925155));
#61156=CARTESIAN_POINT('',(3.15,4.35,80.0832168144927));
#61157=CARTESIAN_POINT('',(0.431981484307159,4.35,79.0939389785961));
#61158=CARTESIAN_POINT('',(3.,4.5,80.1882479452241));
#61159=CARTESIAN_POINT('',(3.15,4.35,80.0832168144927));
#61160=CARTESIAN_POINT('',(0.380678462808311,4.5,79.234892871714));
#61161=CARTESIAN_POINT('Origin',(4.42952305344106,-2.25,79.1459860643051));
#61162=CARTESIAN_POINT('',(4.42952305344106,-4.42047694655894,79.1459860643051));
#61163=CARTESIAN_POINT('',(4.5,-4.35,79.0453345535557));
#61164=CARTESIAN_POINT('',(8.17687780157812,-0.673122198421876,73.7942088501973));
#61165=CARTESIAN_POINT('',(4.5,4.35,79.0453345535557));
#61166=CARTESIAN_POINT('',(4.5,-2.25,79.0453345535557));
#61167=CARTESIAN_POINT('',(4.42952305344106,4.42047694655894,79.1459860643051));
#61168=CARTESIAN_POINT('',(8.73386271393541,0.116137286064592,72.9987519578288));
#61169=CARTESIAN_POINT('',(4.35904610688211,4.35,79.2466375750545));
#61170=CARTESIAN_POINT('',(4.21501121113347,4.20596510425134,79.4523407243193));
#61171=CARTESIAN_POINT('',(4.35904610688211,-4.35,79.2466375750545));
#61172=CARTESIAN_POINT('',(4.35904610688211,-2.25,79.2466375750545));
#61173=CARTESIAN_POINT('',(4.02451115157885,-4.0154650446967,79.7244030046565));
#61174=CARTESIAN_POINT('Origin',(4.55,0.,79.1771360418424));
#61175=CARTESIAN_POINT('',(3.15,4.35,79.6866943698151));
#61176=CARTESIAN_POINT('',(7.69637858619779,4.35,78.0319478907338));
#61177=CARTESIAN_POINT('',(3.15,-4.35,79.6866943698151));
#61178=CARTESIAN_POINT('',(3.15,0.,79.6866943698151));
#61179=CARTESIAN_POINT('',(3.7227785891801,-4.35,79.4782200125285));
#61180=CARTESIAN_POINT('Origin',(7.67072707544837,4.425,77.9614709441749));
#61181=CARTESIAN_POINT('',(4.35,4.5,79.0903034228242));
#61182=CARTESIAN_POINT('',(2.14345992676436,6.70654007323564,77.5452674301829));
#61183=CARTESIAN_POINT('',(3.,4.5,79.5816632390836));
#61184=CARTESIAN_POINT('',(7.64507556469895,4.5,77.8909939976159));
#61185=CARTESIAN_POINT('',(3.15,4.35,79.6866943698151));
#61186=CARTESIAN_POINT('Origin',(4.425,4.425,59.4601776313845));
#61187=CARTESIAN_POINT('',(4.35,4.5,59.4601776313845));
#61188=CARTESIAN_POINT('',(4.5,4.35,59.4601776313845));
#61189=CARTESIAN_POINT('Origin',(4.42952305344106,-2.25,77.2610304721512));
#61190=CARTESIAN_POINT('',(4.42952305344106,-4.42047694655894,77.2610304721512));
#61191=CARTESIAN_POINT('',(4.5,-4.35,77.1603789614018));
#61192=CARTESIAN_POINT('',(7.84367759766981,-1.00632240233019,72.3851124651012));
#61193=CARTESIAN_POINT('',(4.5,4.35,77.1603789614018));
#61194=CARTESIAN_POINT('',(4.5,-2.25,77.1603789614018));
#61195=CARTESIAN_POINT('',(4.42952305344106,4.42047694655894,77.2610304721512));
#61196=CARTESIAN_POINT('',(8.4006625100271,0.449337489972902,71.5896555727327));
#61197=CARTESIAN_POINT('',(4.35904610688211,4.35,77.3616819829007));
#61198=CARTESIAN_POINT('',(4.15803062038505,4.14898451350291,77.6487618492658));
#61199=CARTESIAN_POINT('',(4.35904610688211,-4.35,77.3616819829007));
#61200=CARTESIAN_POINT('',(4.35904610688211,-2.25,77.3616819829007));
#61201=CARTESIAN_POINT('',(3.96753056083043,-3.95848445394826,77.920824129603));
#61202=CARTESIAN_POINT('Origin',(7.36782055058691,4.425,76.1867643108356));
#61203=CARTESIAN_POINT('',(4.35,4.5,77.2053478306703));
#61204=CARTESIAN_POINT('',(2.36314327285774,6.48685672714226,75.8141357729827));
#61205=CARTESIAN_POINT('',(3.,4.5,77.6967076469297));
#61206=CARTESIAN_POINT('',(7.34216903983748,4.5,76.1162873642766));
#61207=CARTESIAN_POINT('',(3.15,4.35,77.8017387776612));
#61208=CARTESIAN_POINT('',(3.15,4.35,77.8017387776612));
#61209=CARTESIAN_POINT('',(7.39347206133633,4.35,76.2572412573945));
#61210=CARTESIAN_POINT('Origin',(4.425,4.425,59.4601776313845));
#61211=CARTESIAN_POINT('',(4.5,4.35,76.9546654464443));
#61212=CARTESIAN_POINT('',(4.5,4.35,59.4601776313845));
#61213=CARTESIAN_POINT('',(4.42952305344105,4.42047694655895,76.8540139356949));
#61214=CARTESIAN_POINT('',(2.17936071997847,6.67063928002153,73.6404490843143));
#61215=CARTESIAN_POINT('',(4.35,4.5,76.9096965771758));
#61216=CARTESIAN_POINT('',(6.36020358479645,2.48979641520355,75.5021368737654));
#61217=CARTESIAN_POINT('',(4.35,4.5,59.4601776313845));
#61218=CARTESIAN_POINT('Origin',(4.5,-4.5,59.4601776313845));
#61219=CARTESIAN_POINT('',(4.5,-4.35,76.9546654464443));
#61220=CARTESIAN_POINT('',(4.5,-4.35,59.4601776313845));
#61221=CARTESIAN_POINT('',(4.5,-2.25,76.9546654464443));
#61222=CARTESIAN_POINT('Origin',(4.42952305344105,-2.25,76.8540139356949));
#61223=CARTESIAN_POINT('',(4.42952305344106,-4.42047694655894,76.8540139356949));
#61224=CARTESIAN_POINT('',(1.62237580762112,-7.22762419237888,72.8449921919458));
#61225=CARTESIAN_POINT('',(4.35904610688211,-4.35,76.7533624249455));
#61226=CARTESIAN_POINT('',(2.77194634461692,-2.76290023773472,74.4867490629657));
#61227=CARTESIAN_POINT('',(4.35904610688211,4.35,76.7533624249455));
#61228=CARTESIAN_POINT('',(4.35904610688211,-2.25,76.7533624249455));
#61229=CARTESIAN_POINT('',(2.96244640417157,2.95340029728938,74.7588113433029));
#61230=CARTESIAN_POINT('Origin',(1.01214302328067,4.425,75.6150026584765));
#61231=CARTESIAN_POINT('',(3.15,4.35,76.3133056301849));
#61232=CARTESIAN_POINT('',(1.0377945340301,4.35,75.5445257119175));
#61233=CARTESIAN_POINT('',(3.,4.5,76.4183367609164));
#61234=CARTESIAN_POINT('',(3.15,4.35,76.3133056301849));
#61235=CARTESIAN_POINT('',(0.986491512531251,4.5,75.6854796050354));
#61236=CARTESIAN_POINT('Origin',(4.42952305344106,-2.25,75.3760748799974));
#61237=CARTESIAN_POINT('',(4.42952305344106,-4.42047694655894,75.3760748799974));
#61238=CARTESIAN_POINT('',(4.5,-4.35,75.2754233692479));
#61239=CARTESIAN_POINT('',(7.51047739376151,-1.33952260623849,70.9760160800051));
#61240=CARTESIAN_POINT('',(4.5,4.35,75.2754233692479));
#61241=CARTESIAN_POINT('',(4.5,-2.25,75.2754233692479));
#61242=CARTESIAN_POINT('',(4.42952305344105,4.42047694655895,75.3760748799974));
#61243=CARTESIAN_POINT('',(8.06746230611879,0.782537693881209,70.1805591876365));
#61244=CARTESIAN_POINT('',(4.35904610688211,4.35,75.4767263907468));
#61245=CARTESIAN_POINT('',(4.10105002963662,4.09200392275448,75.8451829742122));
#61246=CARTESIAN_POINT('',(4.35904610688211,-4.35,75.4767263907468));
#61247=CARTESIAN_POINT('',(4.35904610688211,-2.25,75.4767263907468));
#61248=CARTESIAN_POINT('',(3.910549970082,-3.90150386319978,76.1172452545494));
#61249=CARTESIAN_POINT('Origin',(4.55,0.,75.4072248575346));
#61250=CARTESIAN_POINT('',(3.15,4.35,75.9167831855073));
#61251=CARTESIAN_POINT('',(7.09056553647487,4.35,74.4825346240552));
#61252=CARTESIAN_POINT('',(3.15,-4.35,75.9167831855073));
#61253=CARTESIAN_POINT('',(3.15,0.,75.9167831855073));
#61254=CARTESIAN_POINT('',(3.11696553945717,-4.35,75.9288067458499));
#61255=CARTESIAN_POINT('Origin',(7.06491402572544,4.425,74.4120576774963));
#61256=CARTESIAN_POINT('',(4.35,4.5,75.3203922385165));
#61257=CARTESIAN_POINT('',(2.58282661895114,6.26717338104886,74.0830041157826));
#61258=CARTESIAN_POINT('',(3.,4.5,75.8117520547759));
#61259=CARTESIAN_POINT('',(7.03926251497602,4.5,74.3415807309374));
#61260=CARTESIAN_POINT('',(3.15,4.35,75.9167831855073));
#61261=CARTESIAN_POINT('Origin',(4.425,4.425,59.4601776313845));
#61262=CARTESIAN_POINT('',(4.5,4.35,75.0697098542905));
#61263=CARTESIAN_POINT('',(4.5,4.35,59.4601776313845));
#61264=CARTESIAN_POINT('',(4.42952305344105,4.42047694655895,74.969058343541));
#61265=CARTESIAN_POINT('',(2.51256092388669,6.33743907611331,72.2313526992177));
#61266=CARTESIAN_POINT('',(4.35,4.5,75.0247409850219));
#61267=CARTESIAN_POINT('',(6.14052023870333,2.70947976129667,73.7710052165648));
#61268=CARTESIAN_POINT('',(4.35,4.5,59.4601776313845));
#61269=CARTESIAN_POINT('Origin',(4.42952305344106,-2.25,74.969058343541));
#61270=CARTESIAN_POINT('',(4.5,-4.35,75.0697098542905));
#61271=CARTESIAN_POINT('',(4.5,-2.25,75.0697098542905));
#61272=CARTESIAN_POINT('',(4.42952305344106,-4.42047694655895,74.969058343541));
#61273=CARTESIAN_POINT('',(1.95557601152941,-6.89442398847059,71.4358958068492));
#61274=CARTESIAN_POINT('',(4.35904610688211,-4.35,74.8684068327916));
#61275=CARTESIAN_POINT('',(2.8289269353655,-2.81988082848323,72.6831701879121));
#61276=CARTESIAN_POINT('',(4.35904610688211,4.35,74.8684068327916));
#61277=CARTESIAN_POINT('',(4.35904610688211,-2.25,74.8684068327916));
#61278=CARTESIAN_POINT('',(3.01942699492011,3.01038088803788,72.9552324682493));
#61279=CARTESIAN_POINT('Origin',(3.15,0.,74.4283500380311));
#61280=CARTESIAN_POINT('',(3.15,-4.35,74.4283500380311));
#61281=CARTESIAN_POINT('',(-2.63289893812614,-4.35,72.3235469567835));
#61282=CARTESIAN_POINT('',(3.15,4.35,74.4283500380311));
#61283=CARTESIAN_POINT('',(3.15,0.,74.4283500380311));
#61284=CARTESIAN_POINT('',(1.34070105889156,4.35,73.7698190785782));
#61285=CARTESIAN_POINT('Origin',(-2.65855044887556,-4.425,72.3940239033425));
#61286=CARTESIAN_POINT('',(4.35,-4.5,75.0247409850219));
#61287=CARTESIAN_POINT('',(5.54602950755777,-3.30397049244223,74.1872721079087));
#61288=CARTESIAN_POINT('',(3.,-4.5,74.5333811687625));
#61289=CARTESIAN_POINT('',(-2.68420195962499,-4.5,72.4645008499014));
#61290=CARTESIAN_POINT('',(3.,-4.5,74.5333811687625));
#61291=CARTESIAN_POINT('Origin',(4.425,-4.425,59.4601776313845));
#61292=CARTESIAN_POINT('',(4.35,-4.5,75.3203922385165));
#61293=CARTESIAN_POINT('',(1.98833588780573,-6.86166411219427,73.666737224439));
#61294=CARTESIAN_POINT('',(4.35,-4.5,59.4601776313845));
#61295=CARTESIAN_POINT('',(4.5,-4.35,59.4601776313845));
#61296=CARTESIAN_POINT('Origin',(4.42952305344106,-2.25,73.4911192878435));
#61297=CARTESIAN_POINT('',(4.42952305344106,-4.42047694655894,73.4911192878435));
#61298=CARTESIAN_POINT('',(4.5,-4.35,73.390467777094));
#61299=CARTESIAN_POINT('',(7.1772771898532,-1.6727228101468,69.5669196949089));
#61300=CARTESIAN_POINT('',(4.5,4.35,73.390467777094));
#61301=CARTESIAN_POINT('',(4.5,-2.25,73.390467777094));
#61302=CARTESIAN_POINT('',(4.42952305344105,4.42047694655895,73.4911192878435));
#61303=CARTESIAN_POINT('',(7.73426210221048,1.11573789778952,68.7714628025404));
#61304=CARTESIAN_POINT('',(4.35904610688211,4.35,73.5917707985929));
#61305=CARTESIAN_POINT('',(4.04406943888819,4.03502333200606,74.0416040991587));
#61306=CARTESIAN_POINT('',(4.35904610688211,-4.35,73.5917707985929));
#61307=CARTESIAN_POINT('',(4.35904610688211,-2.25,73.5917707985929));
#61308=CARTESIAN_POINT('',(3.85356937933357,-3.84452327245141,74.3136663794959));
#61309=CARTESIAN_POINT('Origin',(6.76200750086397,4.425,72.637351044157));
#61310=CARTESIAN_POINT('',(4.35,4.5,73.4354366463626));
#61311=CARTESIAN_POINT('',(2.80250996504453,6.04749003495547,72.3518724585824));
#61312=CARTESIAN_POINT('',(3.,4.5,73.926796462622));
#61313=CARTESIAN_POINT('',(6.73635599011455,4.5,72.5668740975981));
#61314=CARTESIAN_POINT('',(3.15,4.35,74.0318275933534));
#61315=CARTESIAN_POINT('',(3.15,4.35,74.0318275933534));
#61316=CARTESIAN_POINT('',(6.78765901161339,4.35,72.7078279907159));
#61317=CARTESIAN_POINT('Origin',(4.425,4.425,59.4601776313845));
#61318=CARTESIAN_POINT('',(4.5,4.35,73.1847542621366));
#61319=CARTESIAN_POINT('',(4.5,4.35,59.4601776313845));
#61320=CARTESIAN_POINT('',(4.42952305344106,4.42047694655894,73.0841027513871));
#61321=CARTESIAN_POINT('',(2.845761127795,6.004238872205,70.8222563141216));
#61322=CARTESIAN_POINT('',(4.35,4.5,73.139785392868));
#61323=CARTESIAN_POINT('',(5.92083689260995,2.92916310739005,72.0398735593647));
#61324=CARTESIAN_POINT('',(4.35,4.5,59.4601776313845));
#61325=CARTESIAN_POINT('Origin',(4.5,-4.5,59.4601776313845));
#61326=CARTESIAN_POINT('',(4.5,-4.35,73.1847542621366));
#61327=CARTESIAN_POINT('',(4.5,-4.35,59.4601776313845));
#61328=CARTESIAN_POINT('',(4.5,-2.25,73.1847542621366));
#61329=CARTESIAN_POINT('Origin',(4.42952305344106,-2.25,73.0841027513871));
#61330=CARTESIAN_POINT('',(4.42952305344106,-4.42047694655894,73.0841027513872));
#61331=CARTESIAN_POINT('',(2.28877621543772,-6.56122378456228,70.0267994217531));
#61332=CARTESIAN_POINT('',(4.35904610688211,-4.35,72.9834512406377));
#61333=CARTESIAN_POINT('',(2.88590752611388,-2.87686141923176,70.8795913128586));
#61334=CARTESIAN_POINT('',(4.35904610688211,4.35,72.9834512406377));
#61335=CARTESIAN_POINT('',(4.35904610688211,-2.25,72.9834512406377));
#61336=CARTESIAN_POINT('',(3.07640758566854,3.06736147878631,71.1516535931958));
#61337=CARTESIAN_POINT('Origin',(1.6179560730036,4.425,72.0655893917979));
#61338=CARTESIAN_POINT('',(3.15,4.35,72.5433944458772));
#61339=CARTESIAN_POINT('',(1.64360758375303,4.35,71.995112445239));
#61340=CARTESIAN_POINT('',(3.,4.5,72.6484255766087));
#61341=CARTESIAN_POINT('',(3.15,4.35,72.5433944458772));
#61342=CARTESIAN_POINT('',(1.59230456225418,4.5,72.1360663383568));
#61343=CARTESIAN_POINT('Origin',(4.42952305344106,-2.25,71.6061636956896));
#61344=CARTESIAN_POINT('',(4.42952305344105,-4.42047694655895,71.6061636956896));
#61345=CARTESIAN_POINT('',(4.5,-4.35,71.5055121849402));
#61346=CARTESIAN_POINT('',(6.84407698594489,-2.00592301405511,68.1578233098128));
#61347=CARTESIAN_POINT('',(4.5,4.35,71.5055121849402));
#61348=CARTESIAN_POINT('',(4.5,-2.25,71.5055121849402));
#61349=CARTESIAN_POINT('',(4.42952305344105,4.42047694655895,71.6061636956896));
#61350=CARTESIAN_POINT('',(7.40106189830217,1.44893810169782,67.3623664174442));
#61351=CARTESIAN_POINT('',(4.35904610688211,4.35,71.706815206439));
#61352=CARTESIAN_POINT('',(3.98708884813977,3.97804274125761,72.2380252241052));
#61353=CARTESIAN_POINT('',(4.35904610688211,-4.35,71.706815206439));
#61354=CARTESIAN_POINT('',(4.35904610688211,-2.25,71.706815206439));
#61355=CARTESIAN_POINT('',(3.79658878858514,-3.78754268170298,72.5100875044424));
#61356=CARTESIAN_POINT('Origin',(6.45910097600251,4.425,70.8626444108177));
#61357=CARTESIAN_POINT('',(4.35,4.5,71.5504810542087));
#61358=CARTESIAN_POINT('',(3.02219331113791,5.82780668886209,70.6207408013823));
#61359=CARTESIAN_POINT('',(3.,4.5,72.0418408704681));
#61360=CARTESIAN_POINT('',(6.43344946525308,4.5,70.7921674642588));
#61361=CARTESIAN_POINT('',(3.15,4.35,72.1468720011996));
#61362=CARTESIAN_POINT('',(3.15,4.35,72.1468720011996));
#61363=CARTESIAN_POINT('',(6.48475248675193,4.35,70.9331213573767));
#61364=CARTESIAN_POINT('Origin',(4.425,4.425,59.4601776313845));
#61365=CARTESIAN_POINT('',(4.5,4.35,71.2997986699827));
#61366=CARTESIAN_POINT('',(4.5,4.35,59.4601776313845));
#61367=CARTESIAN_POINT('',(4.42952305344104,4.42047694655896,71.1991471592332));
#61368=CARTESIAN_POINT('',(3.17896133170339,5.67103866829661,69.4131599290257));
#61369=CARTESIAN_POINT('',(4.35,4.5,71.2548298007141));
#61370=CARTESIAN_POINT('',(5.70115354651634,3.14884645348366,70.3087419021648));
#61371=CARTESIAN_POINT('',(4.35,4.5,59.4601776313845));
#61372=CARTESIAN_POINT('Origin',(4.5,-4.5,59.4601776313845));
#61373=CARTESIAN_POINT('',(4.5,-4.35,71.2997986699827));
#61374=CARTESIAN_POINT('',(4.5,-4.35,59.4601776313845));
#61375=CARTESIAN_POINT('',(4.5,-2.25,71.2997986699827));
#61376=CARTESIAN_POINT('Origin',(4.42952305344105,-2.25,71.1991471592333));
#61377=CARTESIAN_POINT('',(4.42952305344104,-4.42047694655895,71.1991471592332));
#61378=CARTESIAN_POINT('',(2.62197641934605,-6.22802358065395,68.6177030366572));
#61379=CARTESIAN_POINT('',(4.35904610688211,-4.35,71.0984956484838));
#61380=CARTESIAN_POINT('',(2.94288811686221,-2.93384200998003,69.0760124378051));
#61381=CARTESIAN_POINT('',(4.35904610688211,4.35,71.0984956484838));
#61382=CARTESIAN_POINT('',(4.35904610688211,-2.25,71.0984956484838));
#61383=CARTESIAN_POINT('',(3.13338817641685,3.12434206953468,69.3480747181423));
#61384=CARTESIAN_POINT('Origin',(1.92086259786507,4.425,70.2908827584586));
#61385=CARTESIAN_POINT('',(3.15,4.35,70.6584388537233));
#61386=CARTESIAN_POINT('',(1.94651410861449,4.35,70.2204058118997));
#61387=CARTESIAN_POINT('',(3.,4.5,70.7634699844547));
#61388=CARTESIAN_POINT('',(3.15,4.35,70.6584388537233));
#61389=CARTESIAN_POINT('',(1.89521108711565,4.5,70.3613597050175));
#61390=CARTESIAN_POINT('Origin',(4.42952305344106,-2.25,69.7212081035357));
#61391=CARTESIAN_POINT('',(4.42952305344105,-4.42047694655895,69.7212081035357));
#61392=CARTESIAN_POINT('',(4.5,-4.35,69.6205565927863));
#61393=CARTESIAN_POINT('',(6.51087678203658,-2.33912321796342,66.7487269247166));
#61394=CARTESIAN_POINT('',(4.5,4.35,69.6205565927863));
#61395=CARTESIAN_POINT('',(4.5,-2.25,69.6205565927863));
#61396=CARTESIAN_POINT('',(4.42952305344105,4.42047694655895,69.7212081035357));
#61397=CARTESIAN_POINT('',(7.06786169439386,1.78213830560614,65.9532700323481));
#61398=CARTESIAN_POINT('',(4.35904610688211,4.35,69.8218596142852));
#61399=CARTESIAN_POINT('',(3.93010825739134,3.92106215050918,70.4344463490517));
#61400=CARTESIAN_POINT('',(4.35904610688211,-4.35,69.8218596142852));
#61401=CARTESIAN_POINT('',(4.35904610688211,-2.25,69.8218596142852));
#61402=CARTESIAN_POINT('',(3.73960819783673,-3.73056209095443,70.7065086293889));
#61403=CARTESIAN_POINT('Origin',(2.18259445412334,-4.425,70.5342098992732));
#61404=CARTESIAN_POINT('',(3.15,-4.35,70.2619164090457));
#61405=CARTESIAN_POINT('',(2.20824596487276,-4.35,70.6046868458321));
#61406=CARTESIAN_POINT('',(3.,-4.5,70.1568852783142));
#61407=CARTESIAN_POINT('',(3.,-4.5,70.1568852783142));
#61408=CARTESIAN_POINT('',(4.35,-4.5,69.6655254620549));
#61409=CARTESIAN_POINT('',(2.15694294337392,-4.5,70.4637329527142));
#61410=CARTESIAN_POINT('',(2.64738592608591,-6.20261407391409,68.4733422528387));
#61411=CARTESIAN_POINT('Origin',(4.55,0.,69.752358081073));
#61412=CARTESIAN_POINT('',(3.15,4.35,70.2619164090457));
#61413=CARTESIAN_POINT('',(6.18184596189047,4.35,69.1584147240374));
#61414=CARTESIAN_POINT('',(3.15,0.,70.2619164090457));
#61415=CARTESIAN_POINT('Origin',(6.15619445114104,4.425,69.0879377774784));
#61416=CARTESIAN_POINT('',(4.35,4.5,69.6655254620549));
#61417=CARTESIAN_POINT('',(3.24187665723131,5.60812334276869,68.8896091441821));
#61418=CARTESIAN_POINT('',(3.,4.5,70.1568852783142));
#61419=CARTESIAN_POINT('',(6.13054294039162,4.5,69.0174608309195));
#61420=CARTESIAN_POINT('',(3.15,4.35,70.2619164090457));
#61421=CARTESIAN_POINT('Origin',(4.42952305344106,-2.25,116.845097907383));
#61422=CARTESIAN_POINT('',(4.42952305344105,-4.42047694655895,116.845097907383));
#61423=CARTESIAN_POINT('',(4.5,-4.35,116.744446396633));
#61424=CARTESIAN_POINT('',(14.8408818797443,5.9908818797443,101.97613655212));
#61425=CARTESIAN_POINT('',(4.5,4.35,116.744446396633));
#61426=CARTESIAN_POINT('',(4.5,-2.25,116.744446396633));
#61427=CARTESIAN_POINT('',(4.42952305344106,4.42047694655894,116.845097907383));
#61428=CARTESIAN_POINT('',(15.3978667921016,-6.54786679210158,101.180679659752));
#61429=CARTESIAN_POINT('',(4.35904610688211,4.35,116.945749418132));
#61430=CARTESIAN_POINT('',(5.35462302610208,5.34557691922005,115.52391822539));
#61431=CARTESIAN_POINT('',(4.35904610688212,-4.35,116.945749418132));
#61432=CARTESIAN_POINT('',(4.35904610688211,-2.25,116.945749418132));
#61433=CARTESIAN_POINT('',(5.16412296654744,-5.15507685966539,115.795980505727));
#61434=CARTESIAN_POINT('Origin',(13.7288575726779,4.425,113.45560361096));
#61435=CARTESIAN_POINT('',(4.35,4.5,116.789415265902));
#61436=CARTESIAN_POINT('',(-2.25020699510341,11.1002069951034,112.167900574186));
#61437=CARTESIAN_POINT('',(3.,4.5,117.280775082161));
#61438=CARTESIAN_POINT('',(13.7032060619285,4.5,113.385126664401));
#61439=CARTESIAN_POINT('',(3.15,4.35,117.385806212893));
#61440=CARTESIAN_POINT('',(3.15,4.35,117.385806212893));
#61441=CARTESIAN_POINT('',(13.7545090834273,4.35,113.526080557519));
#61442=CARTESIAN_POINT('Origin',(4.425,4.425,59.4601776313845));
#61443=CARTESIAN_POINT('',(4.5,4.35,116.538732881676));
#61444=CARTESIAN_POINT('',(4.5,4.35,59.4601776313845));
#61445=CARTESIAN_POINT('',(4.42952305344106,4.42047694655894,116.438081370926));
#61446=CARTESIAN_POINT('',(-4.8178435620961,13.6678435620961,103.231473171333));
#61447=CARTESIAN_POINT('',(4.35,4.5,116.493764012407));
#61448=CARTESIAN_POINT('',(10.9735538527579,-2.12355385275793,111.855901674968));
#61449=CARTESIAN_POINT('',(4.35,4.5,59.4601776313845));
#61450=CARTESIAN_POINT('Origin',(4.5,-4.5,59.4601776313845));
#61451=CARTESIAN_POINT('',(4.5,-4.35,116.538732881676));
#61452=CARTESIAN_POINT('',(4.5,-4.35,59.4601776313845));
#61453=CARTESIAN_POINT('',(4.5,-2.25,116.538732881676));
#61454=CARTESIAN_POINT('Origin',(4.42952305344106,-2.25,116.438081370926));
#61455=CARTESIAN_POINT('',(4.42952305344106,-4.42047694655894,116.438081370926));
#61456=CARTESIAN_POINT('',(-5.37482847445338,-14.2248284744534,102.436016278964));
#61457=CARTESIAN_POINT('',(4.35904610688211,-4.35,116.337429860177));
#61458=CARTESIAN_POINT('',(1.57535393889992,-1.56630783201787,112.361905439089));
#61459=CARTESIAN_POINT('',(4.35904610688211,4.35,116.337429860177));
#61460=CARTESIAN_POINT('',(4.35904610688211,-2.25,116.337429860177));
#61461=CARTESIAN_POINT('',(1.76585399845467,1.75680789157236,112.633967719427));
#61462=CARTESIAN_POINT('Origin',(-5.34889399881033,4.425,112.883841958601));
#61463=CARTESIAN_POINT('',(3.15,4.35,115.897373065416));
#61464=CARTESIAN_POINT('',(-5.3232424880609,4.35,112.813365012042));
#61465=CARTESIAN_POINT('',(3.,4.5,116.002404196148));
#61466=CARTESIAN_POINT('',(3.15,4.35,115.897373065416));
#61467=CARTESIAN_POINT('',(-5.37454550955975,4.5,112.95431890516));
#61468=CARTESIAN_POINT('Origin',(4.42952305344106,-2.25,114.960142315229));
#61469=CARTESIAN_POINT('',(4.42952305344107,-4.42047694655893,114.960142315229));
#61470=CARTESIAN_POINT('',(4.5,-4.35,114.859490804479));
#61471=CARTESIAN_POINT('',(14.507681675836,5.65768167583598,100.567040167024));
#61472=CARTESIAN_POINT('',(4.5,4.35,114.859490804479));
#61473=CARTESIAN_POINT('',(4.5,-2.25,114.859490804479));
#61474=CARTESIAN_POINT('',(4.42952305344106,4.42047694655894,114.960142315229));
#61475=CARTESIAN_POINT('',(15.0646665881933,-6.21466658819326,99.7715832746552));
#61476=CARTESIAN_POINT('',(4.35904610688211,4.35,115.060793825978));
#61477=CARTESIAN_POINT('',(5.29764243535362,5.28859632847161,113.720339350336));
#61478=CARTESIAN_POINT('',(4.35904610688212,-4.35,115.060793825978));
#61479=CARTESIAN_POINT('',(4.35904610688212,-2.25,115.060793825978));
#61480=CARTESIAN_POINT('',(5.10714237579906,-5.09809626891695,113.992401630673));
#61481=CARTESIAN_POINT('Origin',(13.4259510478164,4.425,111.680896977621));
#61482=CARTESIAN_POINT('',(4.35,4.5,114.904459673748));
#61483=CARTESIAN_POINT('',(-2.03052364901003,10.88052364901,110.436768916986));
#61484=CARTESIAN_POINT('',(3.,4.5,115.395819490007));
#61485=CARTESIAN_POINT('',(13.400299537067,4.5,111.610420031062));
#61486=CARTESIAN_POINT('',(3.15,4.35,115.500850620739));
#61487=CARTESIAN_POINT('',(3.15,4.35,115.500850620739));
#61488=CARTESIAN_POINT('',(13.4516025585659,4.35,111.75137392418));
#61489=CARTESIAN_POINT('Origin',(4.425,4.425,59.4601776313845));
#61490=CARTESIAN_POINT('',(4.5,4.35,114.653777289522));
#61491=CARTESIAN_POINT('',(4.5,4.35,59.4601776313845));
#61492=CARTESIAN_POINT('',(4.42952305344105,4.42047694655895,114.553125778772));
#61493=CARTESIAN_POINT('',(-4.48464335818771,13.3346433581877,101.822376786238));
#61494=CARTESIAN_POINT('',(4.35,4.5,114.608808420253));
#61495=CARTESIAN_POINT('',(10.7538705066645,-1.90387050666449,110.124770017768));
#61496=CARTESIAN_POINT('',(4.35,4.5,59.4601776313845));
#61497=CARTESIAN_POINT('Origin',(4.5,-4.5,59.4601776313845));
#61498=CARTESIAN_POINT('',(4.5,-4.35,114.653777289522));
#61499=CARTESIAN_POINT('',(4.5,-4.35,59.4601776313845));
#61500=CARTESIAN_POINT('',(4.5,-2.25,114.653777289522));
#61501=CARTESIAN_POINT('Origin',(4.42952305344105,-2.25,114.553125778772));
#61502=CARTESIAN_POINT('',(4.42952305344105,-4.42047694655895,114.553125778772));
#61503=CARTESIAN_POINT('',(-5.04162827054505,-13.8916282705451,101.02691989387));
#61504=CARTESIAN_POINT('',(4.35904610688211,-4.35,114.452474268023));
#61505=CARTESIAN_POINT('',(1.63233452964815,-1.62328842276621,110.558326564036));
#61506=CARTESIAN_POINT('',(4.35904610688211,4.35,114.452474268023));
#61507=CARTESIAN_POINT('',(4.35904610688211,-2.25,114.452474268023));
#61508=CARTESIAN_POINT('',(1.82283458920287,1.81378848232088,110.830388844373));
#61509=CARTESIAN_POINT('Origin',(-5.04598747394865,4.425,111.109135325262));
#61510=CARTESIAN_POINT('',(3.15,4.35,114.012417473262));
#61511=CARTESIAN_POINT('',(-5.02033596319923,4.35,111.038658378703));
#61512=CARTESIAN_POINT('',(3.,4.5,114.117448603994));
#61513=CARTESIAN_POINT('',(3.15,4.35,114.012417473262));
#61514=CARTESIAN_POINT('',(-5.07163898469808,4.5,111.179612271821));
#61515=CARTESIAN_POINT('Origin',(4.42952305344106,-2.25,113.075186723075));
#61516=CARTESIAN_POINT('',(4.5,4.35,112.974535212325));
#61517=CARTESIAN_POINT('',(4.5,-2.25,112.974535212325));
#61518=CARTESIAN_POINT('',(4.42952305344106,4.42047694655894,113.075186723075));
#61519=CARTESIAN_POINT('',(14.731466384285,-5.88146638428496,98.3624868895593));
#61520=CARTESIAN_POINT('',(4.35904610688211,4.35,113.175838233824));
#61521=CARTESIAN_POINT('',(5.24066184460522,5.23161573772318,111.916760475283));
#61522=CARTESIAN_POINT('',(4.35904610688212,-4.35,113.175838233824));
#61523=CARTESIAN_POINT('',(4.35904610688211,-2.25,113.175838233824));
#61524=CARTESIAN_POINT('',(5.05016178505058,-5.04111567816854,112.18882275562));
#61525=CARTESIAN_POINT('Origin',(9.14944452593728,-4.425,111.352462466077));
#61526=CARTESIAN_POINT('',(3.15,-4.35,113.615895028585));
#61527=CARTESIAN_POINT('',(9.17509603668671,-4.35,111.422939412636));
#61528=CARTESIAN_POINT('',(3.,-4.5,113.510863897853));
#61529=CARTESIAN_POINT('',(3.,-4.5,113.510863897853));
#61530=CARTESIAN_POINT('',(9.12379301518786,-4.5,111.281985519518));
#61531=CARTESIAN_POINT('Origin',(4.55,0.,113.106336700612));
#61532=CARTESIAN_POINT('',(3.15,4.35,113.615895028585));
#61533=CARTESIAN_POINT('',(13.1486960337044,4.35,109.976667290841));
#61534=CARTESIAN_POINT('',(3.15,0.,113.615895028585));
#61535=CARTESIAN_POINT('Origin',(13.123044522955,4.425,109.906190344282));
#61536=CARTESIAN_POINT('',(4.35,4.5,113.019504081594));
#61537=CARTESIAN_POINT('',(-1.81084030291663,10.6608403029166,108.705637259786));
#61538=CARTESIAN_POINT('',(3.,4.5,113.510863897853));
#61539=CARTESIAN_POINT('',(13.0973930122055,4.5,109.835713397723));
#61540=CARTESIAN_POINT('',(3.15,4.35,113.615895028585));
#61541=CARTESIAN_POINT('Origin',(4.178033008589,-1.125,59.5132106399735));
#61542=CARTESIAN_POINT('',(4.05000000000001,4.2,59.4601776313845));
#61543=CARTESIAN_POINT('',(4.30606601717799,4.30606601717799,59.5662436485625));
#61544=CARTESIAN_POINT('',(2.66093885398715,3.62463203435592,58.8848096657404));
#61545=CARTESIAN_POINT('',(4.30606601717799,-4.30606601717799,59.5662436485625));
#61546=CARTESIAN_POINT('',(4.30606601717798,-1.125,59.5662436485625));
#61547=CARTESIAN_POINT('',(4.05000000000001,-4.2,59.4601776313845));
#61548=CARTESIAN_POINT('',(1.33270642526082,-3.07446014839369,58.3346377797782));
#61549=CARTESIAN_POINT('',(4.05000000000001,-1.125,59.4601776313845));
#61550=CARTESIAN_POINT('Origin',(0.,0.,59.4601776313845));
#61551=CARTESIAN_POINT('',(-4.05000000000001,-4.2,59.4601776313845));
#61552=CARTESIAN_POINT('',(-2.25,-4.2,59.4601776313845));
#61553=CARTESIAN_POINT('',(-4.05000000000001,4.2,59.4601776313845));
#61554=CARTESIAN_POINT('',(-4.05000000000001,1.125,59.4601776313845));
#61555=CARTESIAN_POINT('',(2.25,4.2,59.4601776313845));
#61556=CARTESIAN_POINT('',(-1.905,2.33295215237571E-16,59.4601776313845));
#61557=CARTESIAN_POINT('Origin',(0.,0.,59.4601776313845));
#61558=CARTESIAN_POINT('Origin',(-2.25,-4.35,59.6101776313845));
#61559=CARTESIAN_POINT('',(4.39393398282202,-4.39393398282202,59.6541116142065));
#61560=CARTESIAN_POINT('',(4.2,-4.2,59.4601776313845));
#61561=CARTESIAN_POINT('',(-4.39393398282202,-4.39393398282202,59.6541116142065));
#61562=CARTESIAN_POINT('',(-3.375,-4.39393398282202,59.6541116142065));
#61563=CARTESIAN_POINT('',(-4.30606601717799,-4.30606601717799,59.5662436485625));
#61564=CARTESIAN_POINT('',(-4.2,-4.2,59.4601776313845));
#61565=CARTESIAN_POINT('',(-2.66093885398715,-3.62463203435592,58.8848096657404));
#61566=CARTESIAN_POINT('Origin',(-4.44696699141101,3.375,59.7821446227955));
#61567=CARTESIAN_POINT('',(-4.425,4.425,59.7291116142065));
#61568=CARTESIAN_POINT('',(-4.39393398282202,4.39393398282202,59.6541116142065));
#61569=CARTESIAN_POINT('',(-3.87891329166411,3.87891329166411,58.4107416767103));
#61570=CARTESIAN_POINT('',(-4.39393398282202,3.375,59.6541116142065));
#61571=CARTESIAN_POINT('',(-4.425,-4.425,59.7291116142065));
#61572=CARTESIAN_POINT('',(-3.87891329166411,-3.87891329166411,58.4107416767103));
#61573=CARTESIAN_POINT('',(-4.5,-4.35,59.9101776313845));
#61574=CARTESIAN_POINT('',(-4.89129647405225,-3.95870352594775,60.8548508859502));
#61575=CARTESIAN_POINT('',(-4.5,4.35,59.9101776313845));
#61576=CARTESIAN_POINT('',(-4.5,3.375,59.9101776313845));
#61577=CARTESIAN_POINT('',(-4.46017538852391,4.38982461147609,59.8140325142427));
#61578=CARTESIAN_POINT('Origin',(-4.35,2.25,59.6101776313845));
#61579=CARTESIAN_POINT('',(-4.30606601717799,4.30606601717799,59.5662436485625));
#61580=CARTESIAN_POINT('',(-4.5,4.5,59.7601776313845));
#61581=CARTESIAN_POINT('',(-4.30606601717798,1.125,59.5662436485625));
#61582=CARTESIAN_POINT('Origin',(3.375,4.44696699141101,59.7821446227955));
#61583=CARTESIAN_POINT('',(-4.35,4.5,59.9101776313845));
#61584=CARTESIAN_POINT('',(-3.95870352594775,4.89129647405225,60.8548508859502));
#61585=CARTESIAN_POINT('',(4.35,4.5,59.9101776313845));
#61586=CARTESIAN_POINT('',(3.375,4.5,59.9101776313845));
#61587=CARTESIAN_POINT('',(4.43786796564403,4.41213203435597,59.6980455970285));
#61588=CARTESIAN_POINT('',(4.38982461147609,4.46017538852391,59.8140325142427));
#61589=CARTESIAN_POINT('',(4.39393398282202,4.39393398282202,59.6541116142065));
#61590=CARTESIAN_POINT('',(3.53998854218627,4.04021819978403,58.8001661735708));
#61591=CARTESIAN_POINT('',(3.375,4.39393398282202,59.6541116142065));
#61592=CARTESIAN_POINT('Origin',(-4.425,4.425,59.4601776313845));
#61593=CARTESIAN_POINT('',(-4.5,4.35,144.510177631384));
#61594=CARTESIAN_POINT('',(-4.5,4.35,59.4601776313845));
#61595=CARTESIAN_POINT('',(-4.425,4.425,144.691243648562));
#61596=CARTESIAN_POINT('',(-17.6438747634856,-8.7938747634856,112.778056915244));
#61597=CARTESIAN_POINT('',(-4.35,4.5,144.510177631384));
#61598=CARTESIAN_POINT('',(9.22499584901393,18.0749958490139,111.737238543536));
#61599=CARTESIAN_POINT('',(-4.35,4.5,59.4601776313845));
#61600=CARTESIAN_POINT('Origin',(-4.178033008589,1.125,59.5132106399735));
#61601=CARTESIAN_POINT('',(-1.33270642526082,3.07446014839369,58.3346377797782));
#61602=CARTESIAN_POINT('Origin',(4.44696699141101,-3.375,144.638210639973));
#61603=CARTESIAN_POINT('',(4.425,4.425,144.691243648562));
#61604=CARTESIAN_POINT('',(4.39393398282201,4.39393398282201,144.766243648562));
#61605=CARTESIAN_POINT('',(3.87891329166412,3.87891329166412,146.009613586059));
#61606=CARTESIAN_POINT('',(4.39393398282201,-4.39393398282201,144.766243648562));
#61607=CARTESIAN_POINT('',(4.39393398282201,-3.375,144.766243648562));
#61608=CARTESIAN_POINT('',(4.425,-4.425,144.691243648562));
#61609=CARTESIAN_POINT('',(3.87891329166412,-3.87891329166411,146.009613586059));
#61610=CARTESIAN_POINT('',(4.5,-4.35,144.510177631384));
#61611=CARTESIAN_POINT('',(17.6438747634856,8.7938747634856,112.778056915244));
#61612=CARTESIAN_POINT('',(4.5,4.35,144.510177631384));
#61613=CARTESIAN_POINT('',(4.5,-3.375,144.510177631384));
#61614=CARTESIAN_POINT('',(18.0749958490139,-9.22499584901393,111.737238543536));
#61615=CARTESIAN_POINT('Origin',(3.375,4.44696699141101,144.638210639973));
#61616=CARTESIAN_POINT('',(4.35,4.5,144.510177631384));
#61617=CARTESIAN_POINT('',(-8.7938747634856,17.6438747634856,112.778056915244));
#61618=CARTESIAN_POINT('',(3.375,4.5,144.510177631384));
#61619=CARTESIAN_POINT('',(-4.39393398282201,4.39393398282201,144.766243648562));
#61620=CARTESIAN_POINT('',(-3.87891329166412,3.87891329166411,146.009613586059));
#61621=CARTESIAN_POINT('',(3.375,4.39393398282201,144.766243648562));
#61622=CARTESIAN_POINT('Origin',(4.425,4.425,59.4601776313845));
#61623=CARTESIAN_POINT('',(4.5,4.35,129.733422026753));
#61624=CARTESIAN_POINT('',(4.5,4.35,59.4601776313845));
#61625=CARTESIAN_POINT('',(4.42952305344106,4.42047694655894,129.632770516003));
#61626=CARTESIAN_POINT('',(-7.15024498945427,16.0002449894543,113.095147867005));
#61627=CARTESIAN_POINT('',(4.35,4.5,129.688453157484));
#61628=CARTESIAN_POINT('',(12.5113372754116,-3.66133727541164,123.973823275369));
#61629=CARTESIAN_POINT('',(4.35,4.5,59.4601776313845));
#61630=CARTESIAN_POINT('Origin',(4.5,-4.5,59.4601776313845));
#61631=CARTESIAN_POINT('',(4.5,-4.35,129.733422026753));
#61632=CARTESIAN_POINT('',(4.5,-4.35,59.4601776313845));
#61633=CARTESIAN_POINT('',(4.5,-2.25,129.733422026753));
#61634=CARTESIAN_POINT('Origin',(4.42952305344106,-2.25,126.269875868152));
#61635=CARTESIAN_POINT('',(4.42952305344105,-4.42047694655895,126.269875868152));
#61636=CARTESIAN_POINT('',(4.5,-4.35,126.169224357403));
#61637=CARTESIAN_POINT('',(16.5068828992858,7.65688289928583,109.0216184776));
#61638=CARTESIAN_POINT('',(4.5,4.35,126.169224357403));
#61639=CARTESIAN_POINT('',(4.5,-2.25,126.169224357403));
#61640=CARTESIAN_POINT('',(4.42952305344107,4.42047694655893,126.269875868152));
#61641=CARTESIAN_POINT('',(17.0638678116431,-8.21386781164311,108.226161585232));
#61642=CARTESIAN_POINT('',(4.35904610688212,4.35,126.370527378901));
#61643=CARTESIAN_POINT('',(5.63952597984432,5.63047987296221,124.541812600657));
#61644=CARTESIAN_POINT('',(4.35904610688212,-4.35,126.370527378901));
#61645=CARTESIAN_POINT('',(4.35904610688212,-2.25,126.370527378901));
#61646=CARTESIAN_POINT('',(5.44902592028955,-5.43997981340756,124.813874880994));
#61647=CARTESIAN_POINT('Origin',(15.2433901969853,4.425,122.329136777657));
#61648=CARTESIAN_POINT('',(4.35,4.5,126.214193226671));
#61649=CARTESIAN_POINT('',(-3.34862372557137,12.1986237255714,120.823558860185));
#61650=CARTESIAN_POINT('',(3.,4.5,126.705553042931));
#61651=CARTESIAN_POINT('',(15.2177386862358,4.5,122.258659831098));
#61652=CARTESIAN_POINT('',(3.15,4.35,126.810584173662));
#61653=CARTESIAN_POINT('',(3.15,4.35,126.810584173662));
#61654=CARTESIAN_POINT('',(15.2690417077347,4.35,122.399613724216));
#61655=CARTESIAN_POINT('Origin',(4.425,4.425,59.4601776313845));
#61656=CARTESIAN_POINT('',(4.5,4.35,125.963510842445));
#61657=CARTESIAN_POINT('',(4.5,4.35,59.4601776313845));
#61658=CARTESIAN_POINT('',(4.42952305344105,4.42047694655895,125.862859331696));
#61659=CARTESIAN_POINT('',(-6.48384458163758,15.3338445816376,110.276955096815));
#61660=CARTESIAN_POINT('',(4.35,4.5,125.918541973177));
#61661=CARTESIAN_POINT('',(12.0719705832239,-3.22197058322388,120.511559960971));
#61662=CARTESIAN_POINT('',(4.35,4.5,59.4601776313845));
#61663=CARTESIAN_POINT('Origin',(4.5,-4.5,59.4601776313845));
#61664=CARTESIAN_POINT('',(4.5,-4.35,125.963510842445));
#61665=CARTESIAN_POINT('',(4.5,-4.35,59.4601776313845));
#61666=CARTESIAN_POINT('',(4.5,-2.25,125.963510842445));
#61667=CARTESIAN_POINT('Origin',(4.42952305344106,-2.25,125.862859331696));
#61668=CARTESIAN_POINT('',(4.42952305344105,-4.42047694655895,125.862859331696));
#61669=CARTESIAN_POINT('',(-7.04082949399491,-15.8908294939949,109.481498204446));
#61670=CARTESIAN_POINT('',(4.35904610688211,-4.35,125.762207820946));
#61671=CARTESIAN_POINT('',(1.29045098515763,-1.28140487827559,121.379799814357));
#61672=CARTESIAN_POINT('',(4.35904610688211,4.35,125.762207820946));
#61673=CARTESIAN_POINT('',(4.35904610688211,-2.25,125.762207820946));
#61674=CARTESIAN_POINT('',(1.48095104471238,1.47190493783007,121.651862094694));
#61675=CARTESIAN_POINT('Origin',(-6.86342662311746,4.425,121.757375125298));
#61676=CARTESIAN_POINT('',(3.15,4.35,125.322151026186));
#61677=CARTESIAN_POINT('',(-6.83777511236803,4.35,121.686898178739));
#61678=CARTESIAN_POINT('',(3.,4.5,125.427182156917));
#61679=CARTESIAN_POINT('',(3.15,4.35,125.322151026186));
#61680=CARTESIAN_POINT('',(-6.88907813386688,4.5,121.827852071857));
#61681=CARTESIAN_POINT('Origin',(4.42952305344106,-2.25,124.384920275998));
#61682=CARTESIAN_POINT('',(4.42952305344105,-4.42047694655895,124.384920275998));
#61683=CARTESIAN_POINT('',(4.5,-4.35,124.284268765249));
#61684=CARTESIAN_POINT('',(16.1736826953775,7.32368269537753,107.612522092505));
#61685=CARTESIAN_POINT('',(4.5,4.35,124.284268765249));
#61686=CARTESIAN_POINT('',(4.5,-2.25,124.284268765249));
#61687=CARTESIAN_POINT('',(4.42952305344105,4.42047694655895,124.384920275998));
#61688=CARTESIAN_POINT('',(16.7306676077348,-7.88066760773481,106.817065200136));
#61689=CARTESIAN_POINT('',(4.35904610688212,4.35,124.485571786748));
#61690=CARTESIAN_POINT('',(5.58254538909579,5.57349928221377,122.738233725604));
#61691=CARTESIAN_POINT('',(4.35904610688211,-4.35,124.485571786748));
#61692=CARTESIAN_POINT('',(4.35904610688211,-2.25,124.485571786748));
#61693=CARTESIAN_POINT('',(5.39204532954109,-5.38299922265914,123.010296005941));
#61694=CARTESIAN_POINT('Origin',(14.9404836721238,4.425,120.554430144318));
#61695=CARTESIAN_POINT('',(4.35,4.5,124.329237634517));
#61696=CARTESIAN_POINT('',(-3.12894037947692,11.9789403794769,119.092427202987));
#61697=CARTESIAN_POINT('',(3.,4.5,124.820597450777));
#61698=CARTESIAN_POINT('',(14.9148321613744,4.5,120.483953197759));
#61699=CARTESIAN_POINT('',(3.15,4.35,124.925628581508));
#61700=CARTESIAN_POINT('',(3.15,4.35,124.925628581508));
#61701=CARTESIAN_POINT('',(14.9661351828732,4.35,120.624907090876));
#61702=CARTESIAN_POINT('Origin',(4.425,4.425,59.4601776313845));
#61703=CARTESIAN_POINT('',(4.5,4.35,124.078555250291));
#61704=CARTESIAN_POINT('',(4.5,4.35,59.4601776313845));
#61705=CARTESIAN_POINT('',(4.42952305344105,4.42047694655896,123.977903739542));
#61706=CARTESIAN_POINT('',(-6.15064437772934,15.0006443777293,108.867858711717));
#61707=CARTESIAN_POINT('',(4.35,4.5,124.033586381023));
#61708=CARTESIAN_POINT('',(11.8522872371324,-3.00228723713242,118.780428303768));
#61709=CARTESIAN_POINT('',(4.35,4.5,59.4601776313845));
#61710=CARTESIAN_POINT('Origin',(4.5,-4.5,59.4601776313845));
#61711=CARTESIAN_POINT('',(4.5,-4.35,124.078555250291));
#61712=CARTESIAN_POINT('',(4.5,-4.35,59.4601776313845));
#61713=CARTESIAN_POINT('',(4.5,-2.25,124.078555250291));
#61714=CARTESIAN_POINT('Origin',(4.42952305344106,-2.25,123.977903739542));
#61715=CARTESIAN_POINT('',(4.42952305344106,-4.42047694655894,123.977903739542));
#61716=CARTESIAN_POINT('',(-6.70762929008662,-15.5576292900866,108.072401819349));
#61717=CARTESIAN_POINT('',(4.35904610688212,-4.35,123.877252228792));
#61718=CARTESIAN_POINT('',(1.34743157590636,-1.33838546902397,119.576220939304));
#61719=CARTESIAN_POINT('',(4.35904610688212,4.35,123.877252228792));
#61720=CARTESIAN_POINT('',(4.35904610688212,-2.25,123.877252228792));
#61721=CARTESIAN_POINT('',(1.53793163546093,1.52888552857883,119.848283219641));
#61722=CARTESIAN_POINT('Origin',(-6.56052009825622,4.425,119.982668491958));
#61723=CARTESIAN_POINT('',(3.15,4.35,123.437195434032));
#61724=CARTESIAN_POINT('',(-6.53486858750679,4.35,119.912191545399));
#61725=CARTESIAN_POINT('',(3.,4.5,123.542226564763));
#61726=CARTESIAN_POINT('',(3.15,4.35,123.437195434032));
#61727=CARTESIAN_POINT('',(-6.58617160900565,4.5,120.053145438517));
#61728=CARTESIAN_POINT('Origin',(4.42952305344106,-2.25,122.499964683844));
#61729=CARTESIAN_POINT('',(4.42952305344106,-4.42047694655893,122.499964683844));
#61730=CARTESIAN_POINT('',(4.5,-4.35,122.399313173095));
#61731=CARTESIAN_POINT('',(15.8404824914692,6.99048249146922,106.203425707408));
#61732=CARTESIAN_POINT('',(4.5,4.35,122.399313173095));
#61733=CARTESIAN_POINT('',(4.5,-2.25,122.399313173095));
#61734=CARTESIAN_POINT('',(4.42952305344106,4.42047694655894,122.499964683844));
#61735=CARTESIAN_POINT('',(16.3974674038265,-7.54746740382649,105.40796881504));
#61736=CARTESIAN_POINT('',(4.35904610688212,4.35,122.600616194594));
#61737=CARTESIAN_POINT('',(5.52556479834734,5.51651869146533,120.93465485055));
#61738=CARTESIAN_POINT('',(4.35904610688211,-4.35,122.600616194594));
#61739=CARTESIAN_POINT('',(4.35904610688212,-2.25,122.600616194594));
#61740=CARTESIAN_POINT('',(5.33506473879272,-5.32601863191069,121.206717130887));
#61741=CARTESIAN_POINT('Origin',(14.6375771472623,4.425,118.779723510978));
#61742=CARTESIAN_POINT('',(4.35,4.5,122.444282042363));
#61743=CARTESIAN_POINT('',(-2.90925703338358,11.7592570333836,117.361295545787));
#61744=CARTESIAN_POINT('',(3.,4.5,122.935641858623));
#61745=CARTESIAN_POINT('',(14.6119256365129,4.5,118.709246564419));
#61746=CARTESIAN_POINT('',(3.15,4.35,123.040672989354));
#61747=CARTESIAN_POINT('',(3.15,4.35,123.040672989354));
#61748=CARTESIAN_POINT('',(14.6632286580117,4.35,118.850200457537));
#61749=CARTESIAN_POINT('Origin',(4.425,4.425,59.4601776313845));
#61750=CARTESIAN_POINT('',(4.5,4.35,122.193599658137));
#61751=CARTESIAN_POINT('',(4.5,4.35,59.4601776313845));
#61752=CARTESIAN_POINT('',(4.42952305344106,4.42047694655895,122.092948147388));
#61753=CARTESIAN_POINT('',(-5.81744417382102,14.667444173821,107.458762326621));
#61754=CARTESIAN_POINT('',(4.35,4.5,122.148630788869));
#61755=CARTESIAN_POINT('',(11.6326038910391,-2.78260389103911,117.049296646567));
#61756=CARTESIAN_POINT('',(4.35,4.5,59.4601776313845));
#61757=CARTESIAN_POINT('Origin',(4.5,-4.5,59.4601776313845));
#61758=CARTESIAN_POINT('',(4.5,-4.35,122.193599658137));
#61759=CARTESIAN_POINT('',(4.5,-4.35,59.4601776313845));
#61760=CARTESIAN_POINT('',(4.5,-2.25,122.193599658137));
#61761=CARTESIAN_POINT('Origin',(4.42952305344106,-2.25,122.092948147388));
#61762=CARTESIAN_POINT('',(4.42952305344105,-4.42047694655894,122.092948147388));
#61763=CARTESIAN_POINT('',(-6.37442908617831,-15.2244290861783,106.663305434253));
#61764=CARTESIAN_POINT('',(4.35904610688211,-4.35,121.992296636638));
#61765=CARTESIAN_POINT('',(1.40441216665457,-1.39536605977259,117.77264206425));
#61766=CARTESIAN_POINT('',(4.35904610688211,4.35,121.992296636638));
#61767=CARTESIAN_POINT('',(4.35904610688211,-2.25,121.992296636638));
#61768=CARTESIAN_POINT('',(1.59491222620929,1.58586611932729,118.044704344587));
#61769=CARTESIAN_POINT('Origin',(-6.25761357339475,4.425,118.207961858619));
#61770=CARTESIAN_POINT('',(3.15,4.35,121.552239841878));
#61771=CARTESIAN_POINT('',(-6.23196206264532,4.35,118.13748491206));
#61772=CARTESIAN_POINT('',(3.,4.5,121.657270972609));
#61773=CARTESIAN_POINT('',(3.15,4.35,121.552239841878));
#61774=CARTESIAN_POINT('',(-6.28326508414417,4.5,118.278438805178));
#61775=CARTESIAN_POINT('Origin',(4.42952305344106,-2.25,120.61500909169));
#61776=CARTESIAN_POINT('',(4.42952305344107,-4.42047694655894,120.61500909169));
#61777=CARTESIAN_POINT('',(4.5,-4.35,120.514357580941));
#61778=CARTESIAN_POINT('',(15.5072822875609,6.65728228756088,104.794329322311));
#61779=CARTESIAN_POINT('',(4.5,4.35,120.514357580941));
#61780=CARTESIAN_POINT('',(4.5,-2.25,120.514357580941));
#61781=CARTESIAN_POINT('',(4.42952305344106,4.42047694655894,120.61500909169));
#61782=CARTESIAN_POINT('',(16.0642671999181,-7.2142671999181,103.998872429942));
#61783=CARTESIAN_POINT('',(4.35904610688212,4.35,120.71566060244));
#61784=CARTESIAN_POINT('',(5.46858420759883,5.45953810071684,119.131075975497));
#61785=CARTESIAN_POINT('',(4.35904610688212,-4.35,120.71566060244));
#61786=CARTESIAN_POINT('',(4.35904610688212,-2.25,120.71566060244));
#61787=CARTESIAN_POINT('',(5.27808414804422,-5.26903804116222,119.403138255834));
#61788=CARTESIAN_POINT('Origin',(14.3346706224008,4.425,117.005016877639));
#61789=CARTESIAN_POINT('',(4.35,4.5,120.55932645021));
#61790=CARTESIAN_POINT('',(-2.68957368729112,11.5395736872911,115.630163888585));
#61791=CARTESIAN_POINT('',(3.,4.5,121.050686266469));
#61792=CARTESIAN_POINT('',(14.3090191116514,4.5,116.93453993108));
#61793=CARTESIAN_POINT('',(3.15,4.35,121.1557173972));
#61794=CARTESIAN_POINT('',(3.15,4.35,121.1557173972));
#61795=CARTESIAN_POINT('',(14.3603221331503,4.35,117.075493824198));
#61796=CARTESIAN_POINT('Origin',(4.425,4.425,59.4601776313845));
#61797=CARTESIAN_POINT('',(4.5,4.35,120.308644065983));
#61798=CARTESIAN_POINT('',(4.5,4.35,59.4601776313845));
#61799=CARTESIAN_POINT('',(4.42952305344105,4.42047694655895,120.207992555234));
#61800=CARTESIAN_POINT('',(-5.48424396991263,14.3342439699126,106.049665941527));
#61801=CARTESIAN_POINT('',(4.35,4.5,120.263675196715));
#61802=CARTESIAN_POINT('',(11.4129205449447,-2.56292054494465,115.318164989369));
#61803=CARTESIAN_POINT('',(4.35,4.5,59.4601776313845));
#61804=CARTESIAN_POINT('Origin',(4.5,-4.5,59.4601776313845));
#61805=CARTESIAN_POINT('',(4.5,-4.35,120.308644065983));
#61806=CARTESIAN_POINT('',(4.5,-4.35,59.4601776313845));
#61807=CARTESIAN_POINT('',(4.5,-2.25,120.308644065983));
#61808=CARTESIAN_POINT('Origin',(4.42952305344105,-2.25,120.207992555234));
#61809=CARTESIAN_POINT('',(4.42952305344106,-4.42047694655894,120.207992555234));
#61810=CARTESIAN_POINT('',(-6.04122888226998,-14.89122888227,105.254209049158));
#61811=CARTESIAN_POINT('',(4.35904610688211,-4.35,120.107341044485));
#61812=CARTESIAN_POINT('',(1.46139275740286,-1.45234665052089,115.969063189196));
#61813=CARTESIAN_POINT('',(4.35904610688211,4.35,120.107341044485));
#61814=CARTESIAN_POINT('',(4.35904610688211,-2.25,120.107341044485));
#61815=CARTESIAN_POINT('',(1.65189281695757,1.64284671007559,116.241125469534));
#61816=CARTESIAN_POINT('Origin',(-5.95470704853306,4.425,116.43325522528));
#61817=CARTESIAN_POINT('',(3.15,4.35,119.667284249724));
#61818=CARTESIAN_POINT('',(-5.92905553778363,4.35,116.362778278721));
#61819=CARTESIAN_POINT('',(3.,4.5,119.772315380456));
#61820=CARTESIAN_POINT('',(3.15,4.35,119.667284249724));
#61821=CARTESIAN_POINT('',(-5.98035855928248,4.5,116.503732171839));
#61822=CARTESIAN_POINT('Origin',(4.42952305344106,-2.25,118.730053499536));
#61823=CARTESIAN_POINT('',(4.42952305344105,-4.42047694655895,118.730053499537));
#61824=CARTESIAN_POINT('',(4.5,-4.35,118.629401988787));
#61825=CARTESIAN_POINT('',(15.1740820836526,6.3240820836526,103.385232937216));
#61826=CARTESIAN_POINT('',(4.5,4.35,118.629401988787));
#61827=CARTESIAN_POINT('',(4.5,-2.25,118.629401988787));
#61828=CARTESIAN_POINT('',(4.42952305344105,4.42047694655895,118.730053499536));
#61829=CARTESIAN_POINT('',(15.7310669960099,-6.88106699600987,102.589776044847));
#61830=CARTESIAN_POINT('',(4.35904610688212,4.35,118.830705010286));
#61831=CARTESIAN_POINT('',(5.41160361685048,5.40255750996847,117.327497100443));
#61832=CARTESIAN_POINT('',(4.35904610688212,-4.35,118.830705010286));
#61833=CARTESIAN_POINT('',(4.35904610688212,-2.25,118.830705010286));
#61834=CARTESIAN_POINT('',(5.22110355729585,-5.21205745041383,117.59955938078));
#61835=CARTESIAN_POINT('Origin',(4.55,0.,118.761203477074));
#61836=CARTESIAN_POINT('',(3.15,4.35,119.270761805046));
#61837=CARTESIAN_POINT('',(14.0574156082888,4.35,115.300787190859));
#61838=CARTESIAN_POINT('',(3.15,-4.35,119.270761805046));
#61839=CARTESIAN_POINT('',(3.15,0.,119.270761805046));
#61840=CARTESIAN_POINT('',(10.0838156112711,-4.35,116.747059312653));
#61841=CARTESIAN_POINT('Origin',(14.0317640975394,4.425,115.2303102443));
#61842=CARTESIAN_POINT('',(4.35,4.5,118.674370858056));
#61843=CARTESIAN_POINT('',(-2.46989034119679,11.3198903411968,113.899032231386));
#61844=CARTESIAN_POINT('',(3.,4.5,119.165730674315));
#61845=CARTESIAN_POINT('',(14.00611258679,4.5,115.159833297741));
#61846=CARTESIAN_POINT('',(3.15,4.35,119.270761805046));
#61847=CARTESIAN_POINT('Origin',(4.425,4.425,59.4601776313845));
#61848=CARTESIAN_POINT('',(4.35,4.5,59.4601776313845));
#61849=CARTESIAN_POINT('',(4.5,4.35,59.4601776313845));
#61850=CARTESIAN_POINT('Origin',(3.075,4.425,86.5380363299847));
#61851=CARTESIAN_POINT('',(3.,4.5,86.5380363299847));
#61852=CARTESIAN_POINT('',(3.15,4.35,86.5380363299847));
#61853=CARTESIAN_POINT('Origin',(3.15,0.,113.615895028585));
#61854=CARTESIAN_POINT('',(3.15,-4.35,114.012417473262));
#61855=CARTESIAN_POINT('',(3.15,0.,114.012417473262));
#61856=CARTESIAN_POINT('',(3.15,-4.35,86.5380363299847));
#61857=CARTESIAN_POINT('Origin',(3.15,0.,114.012417473262));
#61858=CARTESIAN_POINT('',(-8.99393596021693,-4.35,109.592386256909));
#61859=CARTESIAN_POINT('Origin',(3.075,4.425,87.4805141260616));
#61860=CARTESIAN_POINT('',(3.,4.5,87.4805141260616));
#61861=CARTESIAN_POINT('',(3.15,4.35,87.4805141260616));
#61862=CARTESIAN_POINT('Origin',(4.55,0.,114.991292292766));
#61863=CARTESIAN_POINT('',(3.15,-4.35,115.500850620739));
#61864=CARTESIAN_POINT('',(3.15,0.,115.500850620739));
#61865=CARTESIAN_POINT('',(9.47800256154818,-4.35,113.197646045975));
#61866=CARTESIAN_POINT('Origin',(3.15,0.,115.500850620739));
#61867=CARTESIAN_POINT('',(3.15,-4.35,115.897373065416));
#61868=CARTESIAN_POINT('',(3.15,0.,115.897373065416));
#61869=CARTESIAN_POINT('',(3.15,-4.35,87.4805141260616));
#61870=CARTESIAN_POINT('Origin',(3.15,0.,115.897373065416));
#61871=CARTESIAN_POINT('',(-9.29684248507857,-4.35,111.367092890248));
#61872=CARTESIAN_POINT('Origin',(3.075,4.425,88.4229919221386));
#61873=CARTESIAN_POINT('',(3.,4.5,88.4229919221386));
#61874=CARTESIAN_POINT('',(3.15,4.35,88.4229919221386));
#61875=CARTESIAN_POINT('Origin',(4.55,0.,116.87624788492));
#61876=CARTESIAN_POINT('',(3.15,-4.35,117.385806212893));
#61877=CARTESIAN_POINT('',(3.15,0.,117.385806212893));
#61878=CARTESIAN_POINT('',(9.78090908640965,-4.35,114.972352679314));
#61879=CARTESIAN_POINT('Origin',(3.15,0.,117.385806212893));
#61880=CARTESIAN_POINT('',(3.15,-4.35,88.4229919221386));
#61881=CARTESIAN_POINT('Origin',(4.5,4.5,59.4601776313845));
#61882=CARTESIAN_POINT('',(4.35,4.5,112.723852828099));
#61883=CARTESIAN_POINT('',(4.35,4.5,59.4601776313845));
#61884=CARTESIAN_POINT('',(3.,4.5,112.23249301184));
#61885=CARTESIAN_POINT('',(-4.7687324598368,4.5,109.404905638482));
#61886=CARTESIAN_POINT('',(3.,4.5,111.6259083057));
#61887=CARTESIAN_POINT('',(3.,4.5,85.5955585339077));
#61888=CARTESIAN_POINT('',(4.35,4.5,111.13454848944));
#61889=CARTESIAN_POINT('',(12.7944864873441,4.5,108.061006764384));
#61890=CARTESIAN_POINT('',(4.35,4.5,110.838897235946));
#61891=CARTESIAN_POINT('',(4.35,4.5,59.4601776313845));
#61892=CARTESIAN_POINT('',(3.,4.5,110.347537419686));
#61893=CARTESIAN_POINT('',(-4.46582593497534,4.5,107.630199005142));
#61894=CARTESIAN_POINT('',(3.,4.5,109.740952713546));
#61895=CARTESIAN_POINT('',(3.,4.5,84.6530807378308));
#61896=CARTESIAN_POINT('',(4.35,4.5,109.249592897286));
#61897=CARTESIAN_POINT('',(12.4915799624826,4.5,106.286300131044));
#61898=CARTESIAN_POINT('',(4.35,4.5,108.953941643792));
#61899=CARTESIAN_POINT('',(4.35,4.5,59.4601776313845));
#61900=CARTESIAN_POINT('',(3.,4.5,108.462581827532));
#61901=CARTESIAN_POINT('',(-4.16291941011368,4.5,105.855492371803));
#61902=CARTESIAN_POINT('',(3.,4.5,107.855997121392));
#61903=CARTESIAN_POINT('',(3.,4.5,83.7106029417538));
#61904=CARTESIAN_POINT('',(4.35,4.5,107.364637305132));
#61905=CARTESIAN_POINT('',(12.1886734376211,4.5,104.511593497705));
#61906=CARTESIAN_POINT('',(4.35,4.5,107.068986051638));
#61907=CARTESIAN_POINT('',(4.35,4.5,59.4601776313845));
#61908=CARTESIAN_POINT('',(3.,4.5,106.577626235378));
#61909=CARTESIAN_POINT('',(-3.86001288525238,4.5,104.080785738464));
#61910=CARTESIAN_POINT('',(3.,4.5,105.971041529238));
#61911=CARTESIAN_POINT('',(3.,4.5,82.7681251456769));
#61912=CARTESIAN_POINT('',(4.35,4.5,105.479681712978));
#61913=CARTESIAN_POINT('',(11.8857669127596,4.5,102.736886864366));
#61914=CARTESIAN_POINT('',(4.35,4.5,105.184030459484));
#61915=CARTESIAN_POINT('',(4.35,4.5,59.4601776313845));
#61916=CARTESIAN_POINT('',(3.,4.5,104.692670643225));
#61917=CARTESIAN_POINT('',(-3.55710636039092,4.5,102.306079105125));
#61918=CARTESIAN_POINT('',(3.,4.5,104.086085937084));
#61919=CARTESIAN_POINT('',(3.,4.5,81.8256473496));
#61920=CARTESIAN_POINT('',(4.35,4.5,103.594726120825));
#61921=CARTESIAN_POINT('',(11.5828603878982,4.5,100.962180231027));
#61922=CARTESIAN_POINT('',(4.35,4.5,103.29907486733));
#61923=CARTESIAN_POINT('',(4.35,4.5,59.4601776313845));
#61924=CARTESIAN_POINT('',(3.,4.5,102.807715051071));
#61925=CARTESIAN_POINT('',(-3.25419983552944,4.5,100.531372471785));
#61926=CARTESIAN_POINT('',(3.,4.5,102.20113034493));
#61927=CARTESIAN_POINT('',(3.,4.5,80.883169553523));
#61928=CARTESIAN_POINT('',(4.35,4.5,101.709770528671));
#61929=CARTESIAN_POINT('',(11.2799538630365,4.5,99.1874735976874));
#61930=CARTESIAN_POINT('',(4.35,4.5,101.414119275176));
#61931=CARTESIAN_POINT('',(4.35,4.5,59.4601776313845));
#61932=CARTESIAN_POINT('',(3.,4.5,100.922759458917));
#61933=CARTESIAN_POINT('',(-2.95129331066782,4.5,98.7566658384461));
#61934=CARTESIAN_POINT('',(3.,4.5,100.316174752776));
#61935=CARTESIAN_POINT('',(3.,4.5,79.9406917574461));
#61936=CARTESIAN_POINT('',(10.9770473381751,4.5,97.4127669643481));
#61937=CARTESIAN_POINT('',(3.,4.5,78.9982139613691));
#61938=CARTESIAN_POINT('',(3.,4.5,78.0557361652922));
#61939=CARTESIAN_POINT('',(3.,4.5,94.6613079763146));
#61940=CARTESIAN_POINT('',(3.,4.5,77.1132583692153));
#61941=CARTESIAN_POINT('',(4.35,4.5,94.1699481600552));
#61942=CARTESIAN_POINT('',(10.0683277635907,4.5,92.0886470643302));
#61943=CARTESIAN_POINT('',(4.35,4.5,93.8742969065607));
#61944=CARTESIAN_POINT('',(4.35,4.5,59.4601776313845));
#61945=CARTESIAN_POINT('',(3.,4.5,93.3829370903013));
#61946=CARTESIAN_POINT('',(-1.73966721122195,4.5,91.657839305089));
#61947=CARTESIAN_POINT('',(3.,4.5,92.7763523841607));
#61948=CARTESIAN_POINT('',(3.,4.5,76.1707805731383));
#61949=CARTESIAN_POINT('',(4.35,4.5,92.2849925679014));
#61950=CARTESIAN_POINT('',(9.76542123872922,4.5,90.3139404309909));
#61951=CARTESIAN_POINT('',(4.35,4.5,91.9893413144068));
#61952=CARTESIAN_POINT('',(4.35,4.5,59.4601776313845));
#61953=CARTESIAN_POINT('',(3.,4.5,91.4979814981474));
#61954=CARTESIAN_POINT('',(-1.43676068636049,4.5,89.8831326717497));
#61955=CARTESIAN_POINT('',(3.,4.5,90.8913967920069));
#61956=CARTESIAN_POINT('',(3.,4.5,75.2283027770614));
#61957=CARTESIAN_POINT('',(4.35,4.5,90.4000369757475));
#61958=CARTESIAN_POINT('',(9.46251471386775,4.5,88.5392337976516));
#61959=CARTESIAN_POINT('',(4.35,4.5,90.1043857222529));
#61960=CARTESIAN_POINT('',(4.35,4.5,59.4601776313845));
#61961=CARTESIAN_POINT('',(3.,4.5,89.6130259059935));
#61962=CARTESIAN_POINT('',(-1.13385416149902,4.5,88.1084260384104));
#61963=CARTESIAN_POINT('',(3.,4.5,89.006441199853));
#61964=CARTESIAN_POINT('',(3.,4.5,74.2858249809845));
#61965=CARTESIAN_POINT('',(4.35,4.5,88.5150813835936));
#61966=CARTESIAN_POINT('',(9.15960818900628,4.5,86.7645271643124));
#61967=CARTESIAN_POINT('',(4.35,4.5,88.219430130099));
#61968=CARTESIAN_POINT('',(4.35,4.5,59.4601776313845));
#61969=CARTESIAN_POINT('',(3.,4.5,87.7280703138397));
#61970=CARTESIAN_POINT('',(-0.830947636637549,4.5,86.3337194050711));
#61971=CARTESIAN_POINT('',(3.,4.5,87.1214856076991));
#61972=CARTESIAN_POINT('',(3.,4.5,73.3433471849075));
#61973=CARTESIAN_POINT('',(4.35,4.5,86.6301257914397));
#61974=CARTESIAN_POINT('',(8.85670166414481,4.5,84.9898205309731));
#61975=CARTESIAN_POINT('',(4.35,4.5,86.3344745379451));
#61976=CARTESIAN_POINT('',(4.35,4.5,59.4601776313845));
#61977=CARTESIAN_POINT('',(3.,4.5,85.8431147216858));
#61978=CARTESIAN_POINT('',(-0.528041111776089,4.5,84.5590127717318));
#61979=CARTESIAN_POINT('',(3.,4.5,85.2365300155452));
#61980=CARTESIAN_POINT('',(3.,4.5,72.4008693888306));
#61981=CARTESIAN_POINT('',(4.35,4.5,84.7451701992859));
#61982=CARTESIAN_POINT('',(8.55379513928335,4.5,83.2151138976338));
#61983=CARTESIAN_POINT('',(4.35,4.5,84.4495189457913));
#61984=CARTESIAN_POINT('',(4.35,4.5,59.4601776313845));
#61985=CARTESIAN_POINT('',(3.,4.5,83.9581591295319));
#61986=CARTESIAN_POINT('',(-0.225134586914621,4.5,82.7843061383926));
#61987=CARTESIAN_POINT('',(3.,4.5,83.3515744233914));
#61988=CARTESIAN_POINT('',(3.,4.5,71.4583915927537));
#61989=CARTESIAN_POINT('',(8.25088861442188,4.5,81.4404072642945));
#61990=CARTESIAN_POINT('',(3.,4.5,70.5159137966767));
#61991=CARTESIAN_POINT('',(3.,4.5,69.5734360005998));
#61992=CARTESIAN_POINT('',(3.,4.5,68.6309582045228));
#61993=CARTESIAN_POINT('',(3.,4.5,67.6884804084459));
#61994=CARTESIAN_POINT('',(3.,4.5,74.5333811687625));
#61995=CARTESIAN_POINT('',(1.28939803739271,4.5,73.9107729716961));
#61996=CARTESIAN_POINT('',(3.,4.5,66.746002612369));
#61997=CARTESIAN_POINT('',(3.,4.5,65.803524816292));
#61998=CARTESIAN_POINT('',(3.,4.5,64.8610470202151));
#61999=CARTESIAN_POINT('',(4.35,4.5,59.4601776313845));
#62000=CARTESIAN_POINT('',(3.,4.5,129.197093341225));
#62001=CARTESIAN_POINT('',(-7.49489118358982,4.5,125.377265338535));
#62002=CARTESIAN_POINT('',(3.,4.5,128.590508635084));
#62003=CARTESIAN_POINT('',(3.,4.5,94.0778586986002));
#62004=CARTESIAN_POINT('',(4.35,4.5,128.099148818825));
#62005=CARTESIAN_POINT('',(15.5206452110971,4.5,124.033366464437));
#62006=CARTESIAN_POINT('',(4.35,4.5,127.80349756533));
#62007=CARTESIAN_POINT('',(4.35,4.5,59.4601776313845));
#62008=CARTESIAN_POINT('',(3.,4.5,127.312137749071));
#62009=CARTESIAN_POINT('',(-7.19198465872859,4.5,123.602558705196));
#62010=CARTESIAN_POINT('',(3.,4.5,93.1353809025232));
#62011=CARTESIAN_POINT('',(3.,4.5,92.1929031064463));
#62012=CARTESIAN_POINT('',(3.,4.5,91.2504253103694));
#62013=CARTESIAN_POINT('',(3.,4.5,90.3079475142924));
#62014=CARTESIAN_POINT('',(3.,4.5,89.3654697182155));
#62015=CARTESIAN_POINT('Origin',(3.075,4.425,89.3654697182155));
#62016=CARTESIAN_POINT('',(3.15,4.35,89.3654697182155));
#62017=CARTESIAN_POINT('Origin',(3.15,0.,119.270761805046));
#62018=CARTESIAN_POINT('',(3.15,-4.35,119.667284249724));
#62019=CARTESIAN_POINT('',(3.15,0.,119.667284249724));
#62020=CARTESIAN_POINT('',(3.15,-4.35,89.3654697182155));
#62021=CARTESIAN_POINT('Origin',(3.15,0.,119.667284249724));
#62022=CARTESIAN_POINT('',(-9.90265553480133,-4.35,114.916506156926));
#62023=CARTESIAN_POINT('Origin',(3.075,4.425,90.3079475142924));
#62024=CARTESIAN_POINT('',(3.15,4.35,90.3079475142924));
#62025=CARTESIAN_POINT('Origin',(4.55,0.,120.646159069228));
#62026=CARTESIAN_POINT('',(3.15,-4.35,121.1557173972));
#62027=CARTESIAN_POINT('',(3.15,0.,121.1557173972));
#62028=CARTESIAN_POINT('',(10.3867221361326,-4.35,118.521765945993));
#62029=CARTESIAN_POINT('Origin',(3.15,0.,121.1557173972));
#62030=CARTESIAN_POINT('',(3.15,-4.35,121.552239841878));
#62031=CARTESIAN_POINT('',(3.15,0.,121.552239841878));
#62032=CARTESIAN_POINT('',(3.15,-4.35,90.3079475142924));
#62033=CARTESIAN_POINT('Origin',(3.15,0.,121.552239841878));
#62034=CARTESIAN_POINT('',(-10.205562059663,-4.35,116.691212790265));
#62035=CARTESIAN_POINT('Origin',(3.075,4.425,91.2504253103694));
#62036=CARTESIAN_POINT('',(3.15,4.35,91.2504253103694));
#62037=CARTESIAN_POINT('Origin',(4.55,0.,122.531114661382));
#62038=CARTESIAN_POINT('',(3.15,-4.35,123.040672989354));
#62039=CARTESIAN_POINT('',(3.15,0.,123.040672989354));
#62040=CARTESIAN_POINT('',(10.6896286609941,-4.35,120.296472579332));
#62041=CARTESIAN_POINT('Origin',(3.15,0.,123.040672989354));
#62042=CARTESIAN_POINT('',(3.15,-4.35,123.437195434032));
#62043=CARTESIAN_POINT('',(3.15,0.,123.437195434032));
#62044=CARTESIAN_POINT('',(3.15,-4.35,91.2504253103694));
#62045=CARTESIAN_POINT('Origin',(3.15,0.,123.437195434032));
#62046=CARTESIAN_POINT('',(-10.5084685845245,-4.35,118.465919423605));
#62047=CARTESIAN_POINT('Origin',(3.075,4.425,92.1929031064463));
#62048=CARTESIAN_POINT('',(3.15,4.35,92.1929031064463));
#62049=CARTESIAN_POINT('Origin',(4.55,0.,124.416070253535));
#62050=CARTESIAN_POINT('',(3.15,-4.35,124.925628581508));
#62051=CARTESIAN_POINT('',(3.15,0.,124.925628581508));
#62052=CARTESIAN_POINT('',(10.9925351858555,-4.35,122.071179212671));
#62053=CARTESIAN_POINT('Origin',(3.15,0.,124.925628581508));
#62054=CARTESIAN_POINT('',(3.15,-4.35,125.322151026186));
#62055=CARTESIAN_POINT('',(3.15,0.,125.322151026186));
#62056=CARTESIAN_POINT('',(3.15,-4.35,92.1929031064463));
#62057=CARTESIAN_POINT('Origin',(3.15,0.,125.322151026186));
#62058=CARTESIAN_POINT('',(-10.8113751093857,-4.35,120.240626056944));
#62059=CARTESIAN_POINT('Origin',(3.075,4.425,93.1353809025232));
#62060=CARTESIAN_POINT('',(3.15,4.35,127.20710661834));
#62061=CARTESIAN_POINT('',(6.34023534238099,1.159764657619,124.973279782941));
#62062=CARTESIAN_POINT('',(3.15,4.35,93.1353809025232));
#62063=CARTESIAN_POINT('Origin',(4.55,0.,126.301025845689));
#62064=CARTESIAN_POINT('',(3.15,-4.35,126.810584173662));
#62065=CARTESIAN_POINT('',(3.15,0.,126.810584173662));
#62066=CARTESIAN_POINT('',(11.295441710717,-4.35,123.845885846011));
#62067=CARTESIAN_POINT('Origin',(3.15,0.,126.810584173662));
#62068=CARTESIAN_POINT('',(3.15,-4.35,127.20710661834));
#62069=CARTESIAN_POINT('',(3.15,0.,127.20710661834));
#62070=CARTESIAN_POINT('',(3.15,-4.35,93.1353809025232));
#62071=CARTESIAN_POINT('Origin',(-4.17803300858899,1.125,144.907144622795));
#62072=CARTESIAN_POINT('',(-4.04999999999999,4.2,144.960177631385));
#62073=CARTESIAN_POINT('',(-4.30606601717799,4.30606601717799,144.854111614207));
#62074=CARTESIAN_POINT('',(-1.33270642526082,3.07446014839374,146.085717482991));
#62075=CARTESIAN_POINT('',(-4.30606601717799,-4.30606601717799,144.854111614207));
#62076=CARTESIAN_POINT('',(-4.30606601717798,1.125,144.854111614207));
#62077=CARTESIAN_POINT('',(-4.04999999999999,-4.2,144.960177631385));
#62078=CARTESIAN_POINT('',(-2.66093885398715,-3.62463203435597,145.535545597029));
#62079=CARTESIAN_POINT('',(-4.04999999999999,1.125,144.960177631385));
#62080=CARTESIAN_POINT('Origin',(-2.25,-4.35,144.810177631385));
#62081=CARTESIAN_POINT('',(-4.39393398282201,-4.39393398282201,144.766243648562));
#62082=CARTESIAN_POINT('',(-4.2,-4.2,144.960177631385));
#62083=CARTESIAN_POINT('',(-3.375,-4.39393398282201,144.766243648562));
#62084=CARTESIAN_POINT('',(4.2,-4.2,144.960177631385));
#62085=CARTESIAN_POINT('',(4.2,-4.2,144.960177631385));
#62086=CARTESIAN_POINT('',(-2.25,-4.2,144.960177631385));
#62087=CARTESIAN_POINT('Origin',(-4.35,2.25,144.810177631385));
#62088=CARTESIAN_POINT('',(-4.2,4.2,144.960177631385));
#62089=CARTESIAN_POINT('',(-4.39393398282201,3.375,144.766243648562));
#62090=CARTESIAN_POINT('Origin',(-4.44696699141101,3.375,144.638210639973));
#62091=CARTESIAN_POINT('',(-4.425,-4.425,144.691243648562));
#62092=CARTESIAN_POINT('',(-3.87891329166412,-3.87891329166412,146.009613586059));
#62093=CARTESIAN_POINT('',(-4.5,-4.35,144.510177631384));
#62094=CARTESIAN_POINT('',(-4.5,3.375,144.510177631384));
#62095=CARTESIAN_POINT('',(-18.0749958490139,9.22499584901393,111.737238543536));
#62096=CARTESIAN_POINT('Origin',(-3.375,-4.44696699141101,144.638210639973));
#62097=CARTESIAN_POINT('',(-4.35,-4.5,144.510177631384));
#62098=CARTESIAN_POINT('',(8.7938747634856,-17.6438747634856,112.778056915244));
#62099=CARTESIAN_POINT('',(4.35,-4.5,144.510177631384));
#62100=CARTESIAN_POINT('',(-3.375,-4.5,144.510177631384));
#62101=CARTESIAN_POINT('',(-9.22499584901393,-18.0749958490139,111.737238543536));
#62102=CARTESIAN_POINT('Origin',(-4.425,-4.425,59.4601776313845));
#62103=CARTESIAN_POINT('',(-4.35,-4.5,59.9101776313845));
#62104=CARTESIAN_POINT('',(-4.38982461147609,-4.46017538852391,59.8140325142427));
#62105=CARTESIAN_POINT('',(-4.35,-4.5,59.4601776313845));
#62106=CARTESIAN_POINT('',(-4.5,-4.35,59.4601776313845));
#62107=CARTESIAN_POINT('Origin',(4.42952305344106,-2.25,129.632770516003));
#62108=CARTESIAN_POINT('',(4.42952305344107,-4.42047694655894,129.632770516003));
#62109=CARTESIAN_POINT('',(-7.70722990181154,-16.5572299018115,112.299690974637));
#62110=CARTESIAN_POINT('',(4.35904610688212,-4.35,129.532119005254));
#62111=CARTESIAN_POINT('',(1.17648980366091,-1.16744369677909,124.986957564464));
#62112=CARTESIAN_POINT('',(4.35904610688212,4.35,129.532119005254));
#62113=CARTESIAN_POINT('',(4.35904610688212,-2.25,129.532119005254));
#62114=CARTESIAN_POINT('',(1.36698986321579,1.35794375633333,125.259019844801));
#62115=CARTESIAN_POINT('Origin',(-7.46923967284039,4.425,125.306788391976));
#62116=CARTESIAN_POINT('',(3.15,4.35,129.092062210493));
#62117=CARTESIAN_POINT('',(-7.44358816209097,4.35,125.236311445418));
#62118=CARTESIAN_POINT('',(3.15,4.35,129.092062210493));
#62119=CARTESIAN_POINT('Origin',(4.42952305344106,-2.25,128.154831460306));
#62120=CARTESIAN_POINT('',(4.42952305344106,-4.42047694655895,128.154831460306));
#62121=CARTESIAN_POINT('',(4.5,-4.35,128.054179949556));
#62122=CARTESIAN_POINT('',(16.8400831031941,7.99008310319415,110.430714862697));
#62123=CARTESIAN_POINT('',(4.5,4.35,128.054179949556));
#62124=CARTESIAN_POINT('',(4.5,-2.25,128.054179949556));
#62125=CARTESIAN_POINT('',(4.42952305344105,4.42047694655895,128.154831460306));
#62126=CARTESIAN_POINT('',(17.3970680155514,-8.54706801555143,109.635257970328));
#62127=CARTESIAN_POINT('',(4.35904610688211,4.35,128.255482971055));
#62128=CARTESIAN_POINT('',(5.69650657059256,5.68746046371058,126.345391475711));
#62129=CARTESIAN_POINT('',(4.35904610688211,-4.35,128.255482971055));
#62130=CARTESIAN_POINT('',(4.35904610688211,-2.25,128.255482971055));
#62131=CARTESIAN_POINT('',(5.50600651103787,-5.49696040415596,126.617453756048));
#62132=CARTESIAN_POINT('Origin',(15.5462967218465,4.425,124.103843410996));
#62133=CARTESIAN_POINT('',(-3.56830707166375,12.4183070716637,122.554690517387));
#62134=CARTESIAN_POINT('',(3.15,4.35,128.695539765816));
#62135=CARTESIAN_POINT('',(3.15,4.35,128.695539765816));
#62136=CARTESIAN_POINT('',(15.5719482325959,4.35,124.174320357555));
#62137=CARTESIAN_POINT('Origin',(4.425,4.425,59.4601776313845));
#62138=CARTESIAN_POINT('',(4.5,4.35,127.848466434599));
#62139=CARTESIAN_POINT('',(4.5,4.35,59.4601776313845));
#62140=CARTESIAN_POINT('',(4.42952305344106,4.42047694655894,127.74781492385));
#62141=CARTESIAN_POINT('',(-6.81704478554588,15.6670447855459,111.686051481911));
#62142=CARTESIAN_POINT('',(12.2916539293204,-3.44165392932035,122.242691618166));
#62143=CARTESIAN_POINT('Origin',(4.5,-4.5,59.4601776313845));
#62144=CARTESIAN_POINT('',(4.5,-4.35,127.848466434599));
#62145=CARTESIAN_POINT('',(4.5,-4.35,59.4601776313845));
#62146=CARTESIAN_POINT('',(4.5,-2.25,127.848466434599));
#62147=CARTESIAN_POINT('Origin',(4.42952305344106,-2.25,127.74781492385));
#62148=CARTESIAN_POINT('',(4.42952305344107,-4.42047694655893,127.74781492385));
#62149=CARTESIAN_POINT('',(-7.37402969790322,-16.2240296979032,110.890594589543));
#62150=CARTESIAN_POINT('',(4.35904610688211,-4.35,127.6471634131));
#62151=CARTESIAN_POINT('',(1.23347039440895,-1.22442428752731,123.18337868941));
#62152=CARTESIAN_POINT('',(4.35904610688211,4.35,127.6471634131));
#62153=CARTESIAN_POINT('',(4.35904610688211,-2.25,127.6471634131));
#62154=CARTESIAN_POINT('',(1.42397045396367,1.41492434708228,123.455440969748));
#62155=CARTESIAN_POINT('Origin',(-7.16633314797917,4.425,123.532081758637));
#62156=CARTESIAN_POINT('',(-7.14068163722974,4.35,123.461604812078));
#62157=CARTESIAN_POINT('Origin',(3.15,0.,127.20710661834));
#62158=CARTESIAN_POINT('',(-11.1142816342474,-4.35,122.015332690283));
#62159=CARTESIAN_POINT('Origin',(3.075,4.425,94.0778586986002));
#62160=CARTESIAN_POINT('',(3.15,4.35,94.0778586986002));
#62161=CARTESIAN_POINT('Origin',(4.55,0.,128.185981437843));
#62162=CARTESIAN_POINT('',(3.15,-4.35,128.695539765816));
#62163=CARTESIAN_POINT('',(3.15,0.,128.695539765816));
#62164=CARTESIAN_POINT('',(11.5983482355782,-4.35,125.62059247935));
#62165=CARTESIAN_POINT('Origin',(3.15,0.,128.695539765816));
#62166=CARTESIAN_POINT('',(3.15,-4.35,129.092062210493));
#62167=CARTESIAN_POINT('',(3.15,0.,129.092062210493));
#62168=CARTESIAN_POINT('',(3.15,-4.35,94.0778586986002));
#62169=CARTESIAN_POINT('Origin',(3.15,0.,129.092062210493));
#62170=CARTESIAN_POINT('',(-11.4171881591087,-4.35,123.790039323623));
#62171=CARTESIAN_POINT('Origin',(3.075,4.425,64.8610470202151));
#62172=CARTESIAN_POINT('',(3.15,4.35,64.8610470202151));
#62173=CARTESIAN_POINT('Origin',(3.15,0.,70.2619164090457));
#62174=CARTESIAN_POINT('',(3.15,-4.35,70.6584388537233));
#62175=CARTESIAN_POINT('',(3.15,0.,70.6584388537233));
#62176=CARTESIAN_POINT('',(3.15,-4.35,64.8610470202151));
#62177=CARTESIAN_POINT('Origin',(3.15,0.,70.6584388537233));
#62178=CARTESIAN_POINT('',(-2.0270858884032,-4.35,68.7741336901049));
#62179=CARTESIAN_POINT('Origin',(3.075,4.425,65.803524816292));
#62180=CARTESIAN_POINT('',(3.15,4.35,65.803524816292));
#62181=CARTESIAN_POINT('Origin',(4.55,0.,71.6373136732269));
#62182=CARTESIAN_POINT('',(3.15,-4.35,72.1468720011996));
#62183=CARTESIAN_POINT('',(3.15,0.,72.1468720011996));
#62184=CARTESIAN_POINT('',(2.51115248973423,-4.35,72.3793934791714));
#62185=CARTESIAN_POINT('Origin',(3.15,0.,72.1468720011996));
#62186=CARTESIAN_POINT('',(3.15,-4.35,72.5433944458772));
#62187=CARTESIAN_POINT('',(3.15,0.,72.5433944458772));
#62188=CARTESIAN_POINT('',(3.15,-4.35,65.803524816292));
#62189=CARTESIAN_POINT('Origin',(3.15,0.,72.5433944458772));
#62190=CARTESIAN_POINT('',(-2.32999241326467,-4.35,70.5488403234442));
#62191=CARTESIAN_POINT('Origin',(1.31504954814214,4.425,73.8402960251372));
#62192=CARTESIAN_POINT('',(3.15,4.35,74.4283500380311));
#62193=CARTESIAN_POINT('Origin',(3.075,4.425,66.746002612369));
#62194=CARTESIAN_POINT('',(3.15,4.35,66.746002612369));
#62195=CARTESIAN_POINT('Origin',(4.55,0.,73.5222692653807));
#62196=CARTESIAN_POINT('',(3.15,-4.35,74.0318275933534));
#62197=CARTESIAN_POINT('',(3.15,0.,74.0318275933534));
#62198=CARTESIAN_POINT('',(2.8140590145957,-4.35,74.1541001125106));
#62199=CARTESIAN_POINT('Origin',(3.15,0.,74.0318275933534));
#62200=CARTESIAN_POINT('',(3.15,-4.35,66.746002612369));
#62201=CARTESIAN_POINT('Origin',(3.075,4.425,67.6884804084459));
#62202=CARTESIAN_POINT('',(3.15,4.35,67.6884804084459));
#62203=CARTESIAN_POINT('Origin',(3.15,0.,75.9167831855073));
#62204=CARTESIAN_POINT('',(3.15,-4.35,76.3133056301849));
#62205=CARTESIAN_POINT('',(3.15,0.,76.3133056301849));
#62206=CARTESIAN_POINT('',(3.15,-4.35,67.6884804084459));
#62207=CARTESIAN_POINT('Origin',(3.15,0.,76.3133056301849));
#62208=CARTESIAN_POINT('',(-2.9358054629876,-4.35,74.0982535901228));
#62209=CARTESIAN_POINT('Origin',(3.075,4.425,68.6309582045228));
#62210=CARTESIAN_POINT('',(3.15,4.35,68.6309582045228));
#62211=CARTESIAN_POINT('Origin',(4.55,0.,77.2921804496885));
#62212=CARTESIAN_POINT('',(3.15,-4.35,77.8017387776612));
#62213=CARTESIAN_POINT('',(3.15,0.,77.8017387776612));
#62214=CARTESIAN_POINT('',(3.41987206431863,-4.35,77.7035133791892));
#62215=CARTESIAN_POINT('Origin',(3.15,0.,77.8017387776612));
#62216=CARTESIAN_POINT('',(3.15,-4.35,68.6309582045228));
#62217=CARTESIAN_POINT('Origin',(3.075,4.425,69.5734360005998));
#62218=CARTESIAN_POINT('',(3.15,4.35,69.5734360005998));
#62219=CARTESIAN_POINT('Origin',(3.15,0.,79.6866943698151));
#62220=CARTESIAN_POINT('',(3.15,-4.35,80.0832168144927));
#62221=CARTESIAN_POINT('',(3.15,0.,80.0832168144927));
#62222=CARTESIAN_POINT('',(3.15,-4.35,69.5734360005998));
#62223=CARTESIAN_POINT('Origin',(3.15,0.,80.0832168144927));
#62224=CARTESIAN_POINT('',(-3.54161851271054,-4.35,77.6476668568014));
#62225=CARTESIAN_POINT('Origin',(3.075,4.425,70.5159137966767));
#62226=CARTESIAN_POINT('',(3.15,4.35,70.5159137966767));
#62227=CARTESIAN_POINT('Origin',(4.55,0.,81.0620916339962));
#62228=CARTESIAN_POINT('',(3.15,-4.35,81.5716499619689));
#62229=CARTESIAN_POINT('',(3.15,0.,81.5716499619689));
#62230=CARTESIAN_POINT('',(4.02568511404156,-4.35,81.2529266458678));
#62231=CARTESIAN_POINT('Origin',(3.15,0.,81.5716499619689));
#62232=CARTESIAN_POINT('',(3.15,-4.35,81.9681724066466));
#62233=CARTESIAN_POINT('',(3.15,0.,81.9681724066466));
#62234=CARTESIAN_POINT('',(3.15,-4.35,70.5159137966767));
#62235=CARTESIAN_POINT('Origin',(3.15,0.,81.9681724066466));
#62236=CARTESIAN_POINT('',(-3.844525037572,-4.35,79.4223734901407));
#62237=CARTESIAN_POINT('Origin',(4.42952305344105,-2.25,94.2256308015361));
#62238=CARTESIAN_POINT('',(4.42952305344106,-4.42047694655894,94.2256308015361));
#62239=CARTESIAN_POINT('',(4.5,-4.35,94.1249792907867));
#62240=CARTESIAN_POINT('',(10.8424794328446,1.99247943284463,85.0669799309673));
#62241=CARTESIAN_POINT('',(4.5,4.35,94.1249792907867));
#62242=CARTESIAN_POINT('',(4.5,-2.25,94.1249792907867));
#62243=CARTESIAN_POINT('',(4.42952305344106,4.42047694655895,94.2256308015361));
#62244=CARTESIAN_POINT('',(11.399464345202,-2.54946434520197,84.2715230385988));
#62245=CARTESIAN_POINT('',(4.35904610688211,4.35,94.3262823122855));
#62246=CARTESIAN_POINT('',(4.67085593712091,4.66180983023882,93.8809717247474));
#62247=CARTESIAN_POINT('',(4.35904610688211,-4.35,94.3262823122855));
#62248=CARTESIAN_POINT('',(4.35904610688211,-2.25,94.3262823122855));
#62249=CARTESIAN_POINT('',(4.48035587756627,-4.47130977068416,94.1530340050846));
#62250=CARTESIAN_POINT('Origin',(10.0939792743401,4.425,92.1591240108891));
#62251=CARTESIAN_POINT('',(0.385993158017769,8.46400684198224,91.394320687785));
#62252=CARTESIAN_POINT('',(3.15,4.35,94.7663391070461));
#62253=CARTESIAN_POINT('',(3.15,4.35,94.7663391070461));
#62254=CARTESIAN_POINT('',(10.1196307850895,4.35,92.2296009574481));
#62255=CARTESIAN_POINT('Origin',(4.425,4.425,59.4601776313845));
#62256=CARTESIAN_POINT('',(4.5,4.35,93.9192657758292));
#62257=CARTESIAN_POINT('',(4.5,4.35,59.4601776313845));
#62258=CARTESIAN_POINT('',(4.42952305344104,4.42047694655896,93.8186142650798));
#62259=CARTESIAN_POINT('',(-0.819441115196317,9.66944111519632,86.32231655018));
#62260=CARTESIAN_POINT('',(8.33735369963672,0.512646300363287,91.0823217885672));
#62261=CARTESIAN_POINT('Origin',(4.5,-4.5,59.4601776313845));
#62262=CARTESIAN_POINT('',(4.5,-4.35,93.9192657758292));
#62263=CARTESIAN_POINT('',(4.5,-4.35,59.4601776313845));
#62264=CARTESIAN_POINT('',(4.5,-2.25,93.9192657758292));
#62265=CARTESIAN_POINT('Origin',(4.42952305344105,-2.25,93.8186142650798));
#62266=CARTESIAN_POINT('',(4.42952305344105,-4.42047694655895,93.8186142650798));
#62267=CARTESIAN_POINT('',(-1.37642602755366,-10.2264260275537,85.5268596578114));
#62268=CARTESIAN_POINT('',(4.35904610688211,-4.35,93.7179627543304));
#62269=CARTESIAN_POINT('',(2.25912102788096,-2.25007492099894,90.7189589384473));
#62270=CARTESIAN_POINT('',(4.35904610688211,4.35,93.7179627543304));
#62271=CARTESIAN_POINT('',(4.35904610688211,-2.25,93.7179627543304));
#62272=CARTESIAN_POINT('',(2.44962108743568,2.44057498055347,90.9910212187846));
#62273=CARTESIAN_POINT('Origin',(-1.71401570047253,4.425,91.58736235853));
#62274=CARTESIAN_POINT('',(3.15,4.35,93.2779059595698));
#62275=CARTESIAN_POINT('',(-1.6883641897231,4.35,91.5168854119711));
#62276=CARTESIAN_POINT('',(3.15,4.35,93.2779059595698));
#62277=CARTESIAN_POINT('Origin',(4.42952305344106,-2.25,92.3406752093822));
#62278=CARTESIAN_POINT('',(4.42952305344104,-4.42047694655896,92.3406752093823));
#62279=CARTESIAN_POINT('',(4.5,-4.35,92.2400236986328));
#62280=CARTESIAN_POINT('',(10.5092792289363,1.65927922893628,83.6578835458703));
#62281=CARTESIAN_POINT('',(4.5,4.35,92.2400236986328));
#62282=CARTESIAN_POINT('',(4.5,-2.25,92.2400236986328));
#62283=CARTESIAN_POINT('',(4.42952305344105,4.42047694655895,92.3406752093823));
#62284=CARTESIAN_POINT('',(11.0662641412936,-2.21626414129357,82.8624266535018));
#62285=CARTESIAN_POINT('',(4.35904610688211,4.35,92.4413267201317));
#62286=CARTESIAN_POINT('',(4.61387534637246,4.60482923949037,92.0773928496939));
#62287=CARTESIAN_POINT('',(4.35904610688212,-4.35,92.4413267201317));
#62288=CARTESIAN_POINT('',(4.35904610688211,-2.25,92.4413267201317));
#62289=CARTESIAN_POINT('',(4.42337528681781,-4.4143291799357,92.3494551300312));
#62290=CARTESIAN_POINT('Origin',(9.79107274947864,4.425,90.3844173775499));
#62291=CARTESIAN_POINT('',(0.605676504110624,8.24432349588938,89.663189030584));
#62292=CARTESIAN_POINT('',(3.15,4.35,92.8813835148922));
#62293=CARTESIAN_POINT('',(3.15,4.35,92.8813835148922));
#62294=CARTESIAN_POINT('',(9.81672426022806,4.35,90.4548943241088));
#62295=CARTESIAN_POINT('Origin',(4.425,4.425,59.4601776313845));
#62296=CARTESIAN_POINT('',(4.5,4.35,92.0343101836753));
#62297=CARTESIAN_POINT('',(4.5,4.35,59.4601776313845));
#62298=CARTESIAN_POINT('',(4.42952305344105,4.42047694655895,91.9336586729259));
#62299=CARTESIAN_POINT('',(-0.48624091128816,9.33624091128816,84.9132201650821));
#62300=CARTESIAN_POINT('',(8.11767035354384,0.732329646456161,89.3511901313663));
#62301=CARTESIAN_POINT('Origin',(4.5,-4.5,59.4601776313845));
#62302=CARTESIAN_POINT('',(4.5,-4.35,92.0343101836753));
#62303=CARTESIAN_POINT('',(4.5,-4.35,59.4601776313845));
#62304=CARTESIAN_POINT('',(4.5,-2.25,92.0343101836753));
#62305=CARTESIAN_POINT('Origin',(4.42952305344106,-2.25,91.9336586729259));
#62306=CARTESIAN_POINT('',(4.42952305344105,-4.42047694655895,91.9336586729259));
#62307=CARTESIAN_POINT('',(-1.04322582364539,-9.89322582364539,84.1177632727136));
#62308=CARTESIAN_POINT('',(4.35904610688212,-4.35,91.8330071621765));
#62309=CARTESIAN_POINT('',(2.31610161862991,-2.30705551174733,88.9153800633939));
#62310=CARTESIAN_POINT('',(4.35904610688212,4.35,91.8330071621765));
#62311=CARTESIAN_POINT('',(4.35904610688212,-2.25,91.8330071621765));
#62312=CARTESIAN_POINT('',(2.50660167818446,2.49755557130189,89.187442343731));
#62313=CARTESIAN_POINT('Origin',(-1.41110917561106,4.425,89.8126557251908));
#62314=CARTESIAN_POINT('',(3.15,4.35,91.3929503674159));
#62315=CARTESIAN_POINT('',(-1.38545766486164,4.35,89.7421787786318));
#62316=CARTESIAN_POINT('',(3.15,4.35,91.3929503674159));
#62317=CARTESIAN_POINT('Origin',(4.42952305344106,-2.25,90.4557196172284));
#62318=CARTESIAN_POINT('',(4.42952305344106,-4.42047694655894,90.4557196172284));
#62319=CARTESIAN_POINT('',(4.5,-4.35,90.3550681064789));
#62320=CARTESIAN_POINT('',(10.1760790250279,1.32607902502795,82.2487871607733));
#62321=CARTESIAN_POINT('',(4.5,4.35,90.3550681064789));
#62322=CARTESIAN_POINT('',(4.5,-2.25,90.3550681064789));
#62323=CARTESIAN_POINT('',(4.42952305344105,4.42047694655895,90.4557196172284));
#62324=CARTESIAN_POINT('',(10.7330639373852,-1.88306393738517,81.4533302684048));
#62325=CARTESIAN_POINT('',(4.35904610688212,4.35,90.5563711279778));
#62326=CARTESIAN_POINT('',(4.55689475562393,4.54784864874185,90.2738139746405));
#62327=CARTESIAN_POINT('',(4.35904610688212,-4.35,90.5563711279778));
#62328=CARTESIAN_POINT('',(4.35904610688212,-2.25,90.5563711279778));
#62329=CARTESIAN_POINT('',(4.36639469606939,-4.35734858918728,90.5458762549776));
#62330=CARTESIAN_POINT('Origin',(9.48816622461717,4.425,88.6097107442106));
#62331=CARTESIAN_POINT('',(0.825359850204014,8.02464014979599,87.9320573733839));
#62332=CARTESIAN_POINT('',(3.15,4.35,90.9964279227383));
#62333=CARTESIAN_POINT('',(3.15,4.35,90.9964279227383));
#62334=CARTESIAN_POINT('',(9.5138177353666,4.35,88.6801876907695));
#62335=CARTESIAN_POINT('Origin',(4.425,4.425,59.4601776313845));
#62336=CARTESIAN_POINT('',(4.5,4.35,90.1493545915215));
#62337=CARTESIAN_POINT('',(4.5,4.35,59.4601776313845));
#62338=CARTESIAN_POINT('',(4.42952305344106,4.42047694655894,90.048703080772));
#62339=CARTESIAN_POINT('',(-0.153040707379776,9.00304070737977,83.5041237799868));
#62340=CARTESIAN_POINT('',(7.89798700745046,0.952012992549535,87.6200584741661));
#62341=CARTESIAN_POINT('Origin',(4.5,-4.5,59.4601776313845));
#62342=CARTESIAN_POINT('',(4.5,-4.35,90.1493545915215));
#62343=CARTESIAN_POINT('',(4.5,-4.35,59.4601776313845));
#62344=CARTESIAN_POINT('',(4.5,-2.25,90.1493545915215));
#62345=CARTESIAN_POINT('Origin',(4.42952305344106,-2.25,90.048703080772));
#62346=CARTESIAN_POINT('',(4.42952305344105,-4.42047694655895,90.048703080772));
#62347=CARTESIAN_POINT('',(-0.71002561973706,-9.56002561973706,82.7086668876183));
#62348=CARTESIAN_POINT('',(4.35904610688212,-4.35,89.9480515700226));
#62349=CARTESIAN_POINT('',(2.37308220937808,-2.36403610249577,87.1118011883403));
#62350=CARTESIAN_POINT('',(4.35904610688211,4.35,89.9480515700226));
#62351=CARTESIAN_POINT('',(4.35904610688211,-2.25,89.9480515700226));
#62352=CARTESIAN_POINT('',(2.5635822689327,2.55453616205042,87.3838634686775));
#62353=CARTESIAN_POINT('Origin',(-1.1082026507496,4.425,88.0379490918515));
#62354=CARTESIAN_POINT('',(3.15,4.35,89.5079947752621));
#62355=CARTESIAN_POINT('',(-1.08255114000017,4.35,87.9674721452925));
#62356=CARTESIAN_POINT('',(3.15,4.35,89.5079947752621));
#62357=CARTESIAN_POINT('Origin',(4.42952305344106,-2.25,88.5707640250745));
#62358=CARTESIAN_POINT('',(4.42952305344105,-4.42047694655895,88.5707640250745));
#62359=CARTESIAN_POINT('',(4.5,-4.35,88.4701125143251));
#62360=CARTESIAN_POINT('',(9.84287882111967,0.992878821119667,80.839690775678));
#62361=CARTESIAN_POINT('',(4.5,4.35,88.4701125143251));
#62362=CARTESIAN_POINT('',(4.5,-2.25,88.4701125143251));
#62363=CARTESIAN_POINT('',(4.42952305344105,4.42047694655895,88.5707640250745));
#62364=CARTESIAN_POINT('',(10.399863733477,-1.54986373347695,80.0442338833095));
#62365=CARTESIAN_POINT('',(4.35904610688211,4.35,88.6714155358239));
#62366=CARTESIAN_POINT('',(4.49991416487561,4.49086805799351,88.4702350995869));
#62367=CARTESIAN_POINT('',(4.35904610688211,-4.35,88.6714155358239));
#62368=CARTESIAN_POINT('',(4.35904610688211,-2.25,88.6714155358239));
#62369=CARTESIAN_POINT('',(4.30941410532098,-4.30036799843887,88.7422973799241));
#62370=CARTESIAN_POINT('Origin',(4.55,0.,88.6019140026118));
#62371=CARTESIAN_POINT('',(3.15,4.35,89.1114723305844));
#62372=CARTESIAN_POINT('',(9.21091121050513,4.35,86.9054810574302));
#62373=CARTESIAN_POINT('',(3.15,-4.35,89.1114723305844));
#62374=CARTESIAN_POINT('',(3.15,0.,89.1114723305844));
#62375=CARTESIAN_POINT('',(5.23731121348743,-4.35,88.351753179225));
#62376=CARTESIAN_POINT('Origin',(9.18525969975571,4.425,86.8350041108713));
#62377=CARTESIAN_POINT('',(1.04504319629739,7.80495680370261,86.2009257161837));
#62378=CARTESIAN_POINT('',(3.15,4.35,89.1114723305844));
#62379=CARTESIAN_POINT('Origin',(4.425,4.425,59.4601776313845));
#62380=CARTESIAN_POINT('',(4.5,4.35,88.2643989993676));
#62381=CARTESIAN_POINT('',(4.5,4.35,59.4601776313845));
#62382=CARTESIAN_POINT('',(4.42952305344106,4.42047694655894,88.1637474886182));
#62383=CARTESIAN_POINT('',(0.180159496528611,8.66984050347139,82.0950273948914));
#62384=CARTESIAN_POINT('',(7.67830366135663,1.17169633864337,85.8889268169666));
#62385=CARTESIAN_POINT('Origin',(4.42952305344105,-2.25,88.1637474886182));
#62386=CARTESIAN_POINT('',(4.5,-4.35,88.2643989993676));
#62387=CARTESIAN_POINT('',(4.5,-2.25,88.2643989993676));
#62388=CARTESIAN_POINT('',(4.42952305344106,-4.42047694655894,88.1637474886182));
#62389=CARTESIAN_POINT('',(-0.37682541582873,-9.22682541582873,81.2995705025229));
#62390=CARTESIAN_POINT('',(4.35904610688211,-4.35,88.0630959778687));
#62391=CARTESIAN_POINT('',(2.43006280012634,-2.42101669324411,85.3082223132868));
#62392=CARTESIAN_POINT('',(4.35904610688211,4.35,88.0630959778687));
#62393=CARTESIAN_POINT('',(4.35904610688211,-2.25,88.0630959778687));
#62394=CARTESIAN_POINT('',(2.62056285968098,2.61151675279877,85.580284593624));
#62395=CARTESIAN_POINT('Origin',(3.15,0.,87.6230391831082));
#62396=CARTESIAN_POINT('',(3.15,-4.35,87.6230391831082));
#62397=CARTESIAN_POINT('',(-4.75324461215641,-4.35,84.7464933901585));
#62398=CARTESIAN_POINT('',(3.15,4.35,87.6230391831082));
#62399=CARTESIAN_POINT('',(3.15,0.,87.6230391831082));
#62400=CARTESIAN_POINT('',(-0.779644615138703,4.35,86.1927655119533));
#62401=CARTESIAN_POINT('Origin',(-4.77889612290583,-4.425,84.8169703367175));
#62402=CARTESIAN_POINT('',(4.35,-4.5,88.219430130099));
#62403=CARTESIAN_POINT('',(7.08381293021095,-1.76618706978904,86.3051937083105));
#62404=CARTESIAN_POINT('',(3.,-4.5,87.7280703138396));
#62405=CARTESIAN_POINT('',(-4.80454763365525,-4.5,84.8874472832764));
#62406=CARTESIAN_POINT('',(3.,-4.5,87.7280703138396));
#62407=CARTESIAN_POINT('Origin',(4.425,-4.425,59.4601776313845));
#62408=CARTESIAN_POINT('',(4.35,-4.5,88.5150813835936));
#62409=CARTESIAN_POINT('',(0.450552465151825,-8.39944753484817,85.7846588248398));
#62410=CARTESIAN_POINT('',(4.35,-4.5,59.4601776313845));
#62411=CARTESIAN_POINT('',(4.5,-4.35,59.4601776313845));
#62412=CARTESIAN_POINT('Origin',(4.42952305344106,-2.25,86.6858084329206));
#62413=CARTESIAN_POINT('',(4.42952305344105,-4.42047694655895,86.6858084329206));
#62414=CARTESIAN_POINT('',(4.5,-4.35,86.5851569221712));
#62415=CARTESIAN_POINT('',(9.50967861721136,0.659678617211358,79.4305943905819));
#62416=CARTESIAN_POINT('',(4.5,4.35,86.5851569221712));
#62417=CARTESIAN_POINT('',(4.5,-2.25,86.5851569221712));
#62418=CARTESIAN_POINT('',(4.42952305344105,4.42047694655895,86.6858084329206));
#62419=CARTESIAN_POINT('',(10.0666635295686,-1.21666352956864,78.6351374982134));
#62420=CARTESIAN_POINT('',(4.35904610688211,4.35,86.78645994367));
#62421=CARTESIAN_POINT('',(4.44293357412718,4.43388746724507,86.6666562245334));
#62422=CARTESIAN_POINT('',(4.35904610688212,-4.35,86.78645994367));
#62423=CARTESIAN_POINT('',(4.35904610688211,-2.25,86.78645994367));
#62424=CARTESIAN_POINT('',(4.25243351457254,-4.24338740769039,86.9387185048706));
#62425=CARTESIAN_POINT('Origin',(8.88235317489424,4.425,85.060297477532));
#62426=CARTESIAN_POINT('',(1.26472654239079,7.5852734576092,84.4697940589836));
#62427=CARTESIAN_POINT('',(3.15,4.35,87.2265167384306));
#62428=CARTESIAN_POINT('',(3.15,4.35,87.2265167384306));
#62429=CARTESIAN_POINT('',(8.90800468564366,4.35,85.1307744240909));
#62430=CARTESIAN_POINT('Origin',(4.425,4.425,59.4601776313845));
#62431=CARTESIAN_POINT('',(4.5,4.35,86.3794434072137));
#62432=CARTESIAN_POINT('',(4.5,4.35,59.4601776313845));
#62433=CARTESIAN_POINT('',(4.42952305344105,4.42047694655895,86.2787918964643));
#62434=CARTESIAN_POINT('',(0.513359700436765,8.33664029956323,80.6859310097939));
#62435=CARTESIAN_POINT('',(7.45862031526367,1.39137968473633,84.1577951597658));
#62436=CARTESIAN_POINT('Origin',(4.5,-4.5,59.4601776313845));
#62437=CARTESIAN_POINT('',(4.5,-4.35,86.3794434072137));
#62438=CARTESIAN_POINT('',(4.5,-4.35,59.4601776313845));
#62439=CARTESIAN_POINT('',(4.5,-2.25,86.3794434072137));
#62440=CARTESIAN_POINT('Origin',(4.42952305344106,-2.25,86.2787918964643));
#62441=CARTESIAN_POINT('',(4.42952305344106,-4.42047694655894,86.2787918964643));
#62442=CARTESIAN_POINT('',(-0.0436252119204612,-8.89362521192046,79.8904741174253));
#62443=CARTESIAN_POINT('',(4.35904610688211,-4.35,86.1781403857149));
#62444=CARTESIAN_POINT('',(2.48704339087517,-2.47799728399261,83.5046434382333));
#62445=CARTESIAN_POINT('',(4.35904610688212,4.35,86.1781403857148));
#62446=CARTESIAN_POINT('',(4.35904610688212,-2.25,86.1781403857148));
#62447=CARTESIAN_POINT('',(2.67754345042971,2.6684973435472,83.7767057185704));
#62448=CARTESIAN_POINT('Origin',(-0.502389601026665,4.425,84.4885358251729));
#62449=CARTESIAN_POINT('',(3.15,4.35,85.7380835909543));
#62450=CARTESIAN_POINT('',(-0.476738090277241,4.35,84.4180588786139));
#62451=CARTESIAN_POINT('',(3.15,4.35,85.7380835909543));
#62452=CARTESIAN_POINT('Origin',(4.42952305344106,-2.25,84.8008528407667));
#62453=CARTESIAN_POINT('',(4.42952305344105,-4.42047694655895,84.8008528407668));
#62454=CARTESIAN_POINT('',(4.5,-4.35,84.7002013300173));
#62455=CARTESIAN_POINT('',(9.17647841330305,0.326478413303049,78.0214980054857));
#62456=CARTESIAN_POINT('',(4.5,4.35,84.7002013300173));
#62457=CARTESIAN_POINT('',(4.5,-2.25,84.7002013300173));
#62458=CARTESIAN_POINT('',(4.42952305344105,4.42047694655895,84.8008528407668));
#62459=CARTESIAN_POINT('',(9.73346332566033,-0.883463325660333,77.2260411131172));
#62460=CARTESIAN_POINT('',(4.35904610688211,4.35,84.9015043515162));
#62461=CARTESIAN_POINT('',(4.38595298337875,4.37690687649664,84.8630773494798));
#62462=CARTESIAN_POINT('',(4.35904610688211,-4.35,84.9015043515162));
#62463=CARTESIAN_POINT('',(4.35904610688211,-2.25,84.9015043515162));
#62464=CARTESIAN_POINT('',(4.19545292382413,-4.186406816942,85.135139629817));
#62465=CARTESIAN_POINT('Origin',(8.57944665003277,4.425,83.2855908441927));
#62466=CARTESIAN_POINT('',(1.48440988848418,7.36559011151582,82.7386624017834));
#62467=CARTESIAN_POINT('',(3.15,4.35,85.3415611462767));
#62468=CARTESIAN_POINT('',(3.15,4.35,85.3415611462767));
#62469=CARTESIAN_POINT('',(8.60509816078219,4.35,83.3560677907517));
#62470=CARTESIAN_POINT('Origin',(4.425,4.425,59.4601776313845));
#62471=CARTESIAN_POINT('',(4.5,4.35,84.4944878150598));
#62472=CARTESIAN_POINT('',(4.5,4.35,59.4601776313845));
#62473=CARTESIAN_POINT('',(4.42952305344106,4.42047694655894,84.3938363043104));
#62474=CARTESIAN_POINT('',(0.846559904345152,8.00344009565485,79.2768346246984));
#62475=CARTESIAN_POINT('',(7.23893696917029,1.61106303082971,82.4266635025656));
#62476=CARTESIAN_POINT('Origin',(4.5,-4.5,59.4601776313845));
#62477=CARTESIAN_POINT('',(4.5,-4.35,84.4944878150598));
#62478=CARTESIAN_POINT('',(4.5,-4.35,59.4601776313845));
#62479=CARTESIAN_POINT('',(4.5,-2.25,84.4944878150598));
#62480=CARTESIAN_POINT('Origin',(4.42952305344106,-2.25,84.3938363043104));
#62481=CARTESIAN_POINT('',(4.42952305344105,-4.42047694655895,84.3938363043104));
#62482=CARTESIAN_POINT('',(0.289574991987868,-8.56042500801213,78.4813777323299));
#62483=CARTESIAN_POINT('',(4.35904610688212,-4.35,84.293184793561));
#62484=CARTESIAN_POINT('',(2.54402398162343,-2.53497787474096,81.7010645631798));
#62485=CARTESIAN_POINT('',(4.35904610688211,4.35,84.293184793561));
#62486=CARTESIAN_POINT('',(4.35904610688211,-2.25,84.293184793561));
#62487=CARTESIAN_POINT('',(2.73452404117798,2.72547793429572,81.9731268435169));
#62488=CARTESIAN_POINT('Origin',(-0.199483076165196,4.425,82.7138291918336));
#62489=CARTESIAN_POINT('',(3.15,4.35,83.8531279988004));
#62490=CARTESIAN_POINT('',(-0.173831565415771,4.35,82.6433522452747));
#62491=CARTESIAN_POINT('',(3.15,4.35,83.8531279988004));
#62492=CARTESIAN_POINT('Origin',(4.42952305344106,-2.25,82.9158972486129));
#62493=CARTESIAN_POINT('',(4.42952305344105,-4.42047694655895,82.9158972486129));
#62494=CARTESIAN_POINT('',(8.84327820939474,-0.0067217906052579,76.6124016203896));
#62495=CARTESIAN_POINT('',(4.35904610688211,4.35,83.0165487593623));
#62496=CARTESIAN_POINT('',(4.32897239263033,4.31992628574822,83.0594984744263));
#62497=CARTESIAN_POINT('',(4.35904610688211,-4.35,83.0165487593623));
#62498=CARTESIAN_POINT('',(4.35904610688211,-2.25,83.0165487593623));
#62499=CARTESIAN_POINT('',(4.1384723330757,-4.12942622619357,83.3315607547635));
#62500=CARTESIAN_POINT('Origin',(4.30294012815361,-4.425,82.9571563326482));
#62501=CARTESIAN_POINT('',(3.15,-4.35,83.4566055541228));
#62502=CARTESIAN_POINT('',(4.32859163890303,-4.35,83.0276332792071));
#62503=CARTESIAN_POINT('',(3.,-4.5,83.3515744233914));
#62504=CARTESIAN_POINT('',(3.,-4.5,83.3515744233914));
#62505=CARTESIAN_POINT('',(4.35,-4.5,82.860214607132));
#62506=CARTESIAN_POINT('',(4.27728861740418,-4.5,82.8866793860892));
#62507=CARTESIAN_POINT('',(1.10960250343199,-7.740397496568,80.5912638532393));
#62508=CARTESIAN_POINT('Origin',(4.55,0.,82.9470472261501));
#62509=CARTESIAN_POINT('',(3.15,4.35,83.4566055541228));
#62510=CARTESIAN_POINT('',(8.30219163592073,4.35,81.5813611574124));
#62511=CARTESIAN_POINT('',(3.15,0.,83.4566055541228));
#62512=CARTESIAN_POINT('Origin',(8.27654012517131,4.425,81.5108842108534));
#62513=CARTESIAN_POINT('',(3.15,4.35,83.4566055541228));
#62514=CARTESIAN_POINT('Origin',(3.075,4.425,71.4583915927537));
#62515=CARTESIAN_POINT('',(3.15,4.35,71.4583915927537));
#62516=CARTESIAN_POINT('Origin',(3.15,0.,83.4566055541228));
#62517=CARTESIAN_POINT('',(3.15,-4.35,83.8531279988004));
#62518=CARTESIAN_POINT('',(3.15,0.,83.8531279988004));
#62519=CARTESIAN_POINT('',(3.15,-4.35,71.4583915927537));
#62520=CARTESIAN_POINT('Origin',(3.15,0.,83.8531279988004));
#62521=CARTESIAN_POINT('',(-4.14743156243347,-4.35,81.1970801234799));
#62522=CARTESIAN_POINT('Origin',(3.075,4.425,72.4008693888306));
#62523=CARTESIAN_POINT('',(3.15,4.35,72.4008693888306));
#62524=CARTESIAN_POINT('Origin',(4.55,0.,84.832002818304));
#62525=CARTESIAN_POINT('',(3.15,-4.35,85.3415611462767));
#62526=CARTESIAN_POINT('',(3.15,0.,85.3415611462767));
#62527=CARTESIAN_POINT('',(4.6314981637645,-4.35,84.8023399125464));
#62528=CARTESIAN_POINT('Origin',(3.15,0.,85.3415611462767));
#62529=CARTESIAN_POINT('',(3.15,-4.35,85.7380835909543));
#62530=CARTESIAN_POINT('',(3.15,0.,85.7380835909543));
#62531=CARTESIAN_POINT('',(3.15,-4.35,72.4008693888306));
#62532=CARTESIAN_POINT('Origin',(3.15,0.,85.7380835909543));
#62533=CARTESIAN_POINT('',(-4.45033808729494,-4.35,82.9717867568192));
#62534=CARTESIAN_POINT('Origin',(-0.805296125888126,4.425,86.2632424585122));
#62535=CARTESIAN_POINT('',(3.15,4.35,87.6230391831082));
#62536=CARTESIAN_POINT('Origin',(3.075,4.425,73.3433471849075));
#62537=CARTESIAN_POINT('',(3.15,4.35,73.3433471849075));
#62538=CARTESIAN_POINT('Origin',(4.55,0.,86.7169584104579));
#62539=CARTESIAN_POINT('',(3.15,-4.35,87.2265167384306));
#62540=CARTESIAN_POINT('',(3.15,0.,87.2265167384306));
#62541=CARTESIAN_POINT('',(4.93440468862596,-4.35,86.5770465458857));
#62542=CARTESIAN_POINT('Origin',(3.15,0.,87.2265167384306));
#62543=CARTESIAN_POINT('',(3.15,-4.35,73.3433471849075));
#62544=CARTESIAN_POINT('Origin',(3.075,4.425,74.2858249809845));
#62545=CARTESIAN_POINT('',(3.15,4.35,74.2858249809845));
#62546=CARTESIAN_POINT('Origin',(3.15,0.,89.1114723305844));
#62547=CARTESIAN_POINT('',(3.15,-4.35,89.5079947752621));
#62548=CARTESIAN_POINT('',(3.15,0.,89.5079947752621));
#62549=CARTESIAN_POINT('',(3.15,-4.35,74.2858249809845));
#62550=CARTESIAN_POINT('Origin',(3.15,0.,89.5079947752621));
#62551=CARTESIAN_POINT('',(-5.05615113701787,-4.35,86.5212000234978));
#62552=CARTESIAN_POINT('Origin',(3.075,4.425,75.2283027770614));
#62553=CARTESIAN_POINT('',(3.15,4.35,75.2283027770614));
#62554=CARTESIAN_POINT('Origin',(4.55,0.,90.4868695947656));
#62555=CARTESIAN_POINT('',(3.15,-4.35,90.9964279227383));
#62556=CARTESIAN_POINT('',(3.15,0.,90.9964279227383));
#62557=CARTESIAN_POINT('',(5.5402177383489,-4.35,90.1264598125642));
#62558=CARTESIAN_POINT('Origin',(3.15,0.,90.9964279227383));
#62559=CARTESIAN_POINT('',(3.15,-4.35,91.3929503674159));
#62560=CARTESIAN_POINT('',(3.15,0.,91.3929503674159));
#62561=CARTESIAN_POINT('',(3.15,-4.35,75.2283027770614));
#62562=CARTESIAN_POINT('Origin',(3.15,0.,91.3929503674159));
#62563=CARTESIAN_POINT('',(-5.35905766187934,-4.35,88.2959066568371));
#62564=CARTESIAN_POINT('Origin',(3.075,4.425,76.1707805731383));
#62565=CARTESIAN_POINT('',(3.15,4.35,76.1707805731383));
#62566=CARTESIAN_POINT('Origin',(4.55,0.,92.3718251869195));
#62567=CARTESIAN_POINT('',(3.15,-4.35,92.8813835148922));
#62568=CARTESIAN_POINT('',(3.15,0.,92.8813835148922));
#62569=CARTESIAN_POINT('',(5.84312426321037,-4.35,91.9011664459035));
#62570=CARTESIAN_POINT('Origin',(3.15,0.,92.8813835148922));
#62571=CARTESIAN_POINT('',(3.15,-4.35,93.2779059595698));
#62572=CARTESIAN_POINT('',(3.15,0.,93.2779059595698));
#62573=CARTESIAN_POINT('',(3.15,-4.35,76.1707805731383));
#62574=CARTESIAN_POINT('Origin',(3.15,0.,93.2779059595698));
#62575=CARTESIAN_POINT('',(-5.6619641867408,-4.35,90.0706132901764));
#62576=CARTESIAN_POINT('Origin',(3.075,4.425,77.1132583692153));
#62577=CARTESIAN_POINT('',(3.15,4.35,77.1132583692153));
#62578=CARTESIAN_POINT('Origin',(4.55,0.,94.2567807790734));
#62579=CARTESIAN_POINT('',(3.15,-4.35,94.7663391070461));
#62580=CARTESIAN_POINT('',(3.15,0.,94.7663391070461));
#62581=CARTESIAN_POINT('',(6.14603078807183,-4.35,93.6758730792428));
#62582=CARTESIAN_POINT('Origin',(3.15,0.,94.7663391070461));
#62583=CARTESIAN_POINT('',(3.15,-4.35,77.1132583692153));
#62584=CARTESIAN_POINT('Origin',(3.075,4.425,78.0557361652922));
#62585=CARTESIAN_POINT('',(3.15,4.35,78.0557361652922));
#62586=CARTESIAN_POINT('Origin',(3.15,0.,96.6512946992));
#62587=CARTESIAN_POINT('',(3.15,-4.35,97.0478171438776));
#62588=CARTESIAN_POINT('',(3.15,0.,97.0478171438776));
#62589=CARTESIAN_POINT('',(3.15,-4.35,78.0557361652922));
#62590=CARTESIAN_POINT('Origin',(3.15,0.,97.0478171438776));
#62591=CARTESIAN_POINT('',(-6.26777723646374,-4.35,93.620026556855));
#62592=CARTESIAN_POINT('Origin',(3.075,4.425,78.9982139613691));
#62593=CARTESIAN_POINT('',(3.15,4.35,78.9982139613691));
#62594=CARTESIAN_POINT('Origin',(4.55,0.,98.0266919633811));
#62595=CARTESIAN_POINT('',(3.15,-4.35,98.5362502913538));
#62596=CARTESIAN_POINT('',(3.15,0.,98.5362502913538));
#62597=CARTESIAN_POINT('',(6.75184383779476,-4.35,97.2252863459214));
#62598=CARTESIAN_POINT('Origin',(3.15,0.,98.5362502913538));
#62599=CARTESIAN_POINT('',(3.15,-4.35,98.9327727360315));
#62600=CARTESIAN_POINT('',(3.15,0.,98.9327727360315));
#62601=CARTESIAN_POINT('',(3.15,-4.35,78.9982139613691));
#62602=CARTESIAN_POINT('Origin',(3.15,0.,98.9327727360315));
#62603=CARTESIAN_POINT('',(-6.5706837613252,-4.35,95.3947331901942));
#62604=CARTESIAN_POINT('Origin',(4.42952305344106,-2.25,111.190231130921));
#62605=CARTESIAN_POINT('',(4.42952305344105,-4.42047694655895,111.190231130921));
#62606=CARTESIAN_POINT('',(4.5,-4.35,111.089579620172));
#62607=CARTESIAN_POINT('',(13.8412812680194,4.99128126801937,97.7488473968316));
#62608=CARTESIAN_POINT('',(4.5,4.35,111.089579620172));
#62609=CARTESIAN_POINT('',(4.5,-2.25,111.089579620172));
#62610=CARTESIAN_POINT('',(4.42952305344104,4.42047694655895,111.190231130921));
#62611=CARTESIAN_POINT('',(14.3982661803767,-5.54826618037665,96.9533905044631));
#62612=CARTESIAN_POINT('',(4.35904610688211,4.35,111.29088264167));
#62613=CARTESIAN_POINT('',(5.1836812538568,5.17463514697474,110.113181600229));
#62614=CARTESIAN_POINT('',(4.35904610688211,-4.35,111.29088264167));
#62615=CARTESIAN_POINT('',(4.35904610688211,-2.25,111.29088264167));
#62616=CARTESIAN_POINT('',(4.99318119430216,-4.98413508742011,110.385243880566));
#62617=CARTESIAN_POINT('Origin',(12.8201379980935,4.425,108.131483710943));
#62618=CARTESIAN_POINT('',(-1.59115695682325,10.4411569568232,106.974505602586));
#62619=CARTESIAN_POINT('',(3.15,4.35,111.730939436431));
#62620=CARTESIAN_POINT('',(3.15,4.35,111.730939436431));
#62621=CARTESIAN_POINT('',(12.8457895088429,4.35,108.201960657502));
#62622=CARTESIAN_POINT('Origin',(4.425,4.425,59.4601776313845));
#62623=CARTESIAN_POINT('',(4.5,4.35,110.883866105214));
#62624=CARTESIAN_POINT('',(4.5,4.35,59.4601776313845));
#62625=CARTESIAN_POINT('',(4.42952305344106,4.42047694655894,110.783214594465));
#62626=CARTESIAN_POINT('',(-3.81824295037126,12.6682429503713,99.0041840160429));
#62627=CARTESIAN_POINT('',(10.3145038144786,-1.46450381447857,106.662506703367));
#62628=CARTESIAN_POINT('Origin',(4.5,-4.5,59.4601776313845));
#62629=CARTESIAN_POINT('',(4.5,-4.35,110.883866105214));
#62630=CARTESIAN_POINT('',(4.5,-4.35,59.4601776313845));
#62631=CARTESIAN_POINT('',(4.5,-2.25,110.883866105214));
#62632=CARTESIAN_POINT('Origin',(4.42952305344106,-2.25,110.783214594465));
#62633=CARTESIAN_POINT('',(4.42952305344105,-4.42047694655896,110.783214594465));
#62634=CARTESIAN_POINT('',(-4.37522786272848,-13.2252278627285,98.2087271236743));
#62635=CARTESIAN_POINT('',(4.35904610688212,-4.35,110.682563083715));
#62636=CARTESIAN_POINT('',(1.74629571114559,-1.73724960426314,106.951168813929));
#62637=CARTESIAN_POINT('',(4.35904610688212,4.35,110.682563083715));
#62638=CARTESIAN_POINT('',(4.35904610688212,-2.25,110.682563083715));
#62639=CARTESIAN_POINT('',(1.9367957707002,1.92774966381778,107.223231094266));
#62640=CARTESIAN_POINT('Origin',(-4.44017442422591,4.425,107.559722058583));
#62641=CARTESIAN_POINT('',(3.15,4.35,110.242506288955));
#62642=CARTESIAN_POINT('',(-4.41452291347648,4.35,107.489245112025));
#62643=CARTESIAN_POINT('',(3.15,4.35,110.242506288955));
#62644=CARTESIAN_POINT('Origin',(4.42952305344106,-2.25,109.305275538767));
#62645=CARTESIAN_POINT('',(4.42952305344107,-4.42047694655893,109.305275538767));
#62646=CARTESIAN_POINT('',(4.5,-4.35,109.204624028018));
#62647=CARTESIAN_POINT('',(13.5080810641111,4.65808106411106,96.3397510117354));
#62648=CARTESIAN_POINT('',(4.5,4.35,109.204624028018));
#62649=CARTESIAN_POINT('',(4.5,-2.25,109.204624028018));
#62650=CARTESIAN_POINT('',(4.42952305344105,4.42047694655895,109.305275538767));
#62651=CARTESIAN_POINT('',(14.0650659764683,-5.21506597646833,95.5442941193668));
#62652=CARTESIAN_POINT('',(4.35904610688212,4.35,109.405927049517));
#62653=CARTESIAN_POINT('',(5.12670066310835,5.11765455622629,108.309602725176));
#62654=CARTESIAN_POINT('',(4.35904610688212,-4.35,109.405927049517));
#62655=CARTESIAN_POINT('',(4.35904610688212,-2.25,109.405927049517));
#62656=CARTESIAN_POINT('',(4.93620060355377,-4.92715449667165,108.581665005513));
#62657=CARTESIAN_POINT('Origin',(12.517231473232,4.425,106.356777077603));
#62658=CARTESIAN_POINT('',(-1.37147361072985,10.2214736107299,105.243373945386));
#62659=CARTESIAN_POINT('',(3.15,4.35,109.845983844277));
#62660=CARTESIAN_POINT('',(3.15,4.35,109.845983844277));
#62661=CARTESIAN_POINT('',(12.5428829839814,4.35,106.427254024162));
#62662=CARTESIAN_POINT('Origin',(4.425,4.425,59.4601776313845));
#62663=CARTESIAN_POINT('',(4.5,4.35,108.99891051306));
#62664=CARTESIAN_POINT('',(4.5,4.35,59.4601776313845));
#62665=CARTESIAN_POINT('',(4.42952305344105,4.42047694655895,108.898259002311));
#62666=CARTESIAN_POINT('',(-3.48504274646279,12.3350427464628,97.5950876309494));
#62667=CARTESIAN_POINT('',(10.0948204683843,-1.24482046838432,104.931375046168));
#62668=CARTESIAN_POINT('Origin',(4.5,-4.5,59.4601776313845));
#62669=CARTESIAN_POINT('',(4.5,-4.35,108.99891051306));
#62670=CARTESIAN_POINT('',(4.5,-4.35,59.4601776313845));
#62671=CARTESIAN_POINT('',(4.5,-2.25,108.99891051306));
#62672=CARTESIAN_POINT('Origin',(4.42952305344106,-2.25,108.898259002311));
#62673=CARTESIAN_POINT('',(4.42952305344105,-4.42047694655895,108.898259002311));
#62674=CARTESIAN_POINT('',(-4.04202765882012,-12.8920276588201,96.7996307385808));
#62675=CARTESIAN_POINT('',(4.35904610688211,-4.35,108.797607491561));
#62676=CARTESIAN_POINT('',(1.80327630189361,-1.79423019501132,105.147589938876));
#62677=CARTESIAN_POINT('',(4.35904610688211,4.35,108.797607491561));
#62678=CARTESIAN_POINT('',(4.35904610688211,-2.25,108.797607491561));
#62679=CARTESIAN_POINT('',(1.9937763614482,1.98473025456618,105.419652219213));
#62680=CARTESIAN_POINT('Origin',(-4.13726789936425,4.425,105.785015425244));
#62681=CARTESIAN_POINT('',(3.15,4.35,108.357550696801));
#62682=CARTESIAN_POINT('',(-4.11161638861483,4.35,105.714538478685));
#62683=CARTESIAN_POINT('',(3.15,4.35,108.357550696801));
#62684=CARTESIAN_POINT('Origin',(4.42952305344106,-2.25,107.420319946613));
#62685=CARTESIAN_POINT('',(4.42952305344105,-4.42047694655894,107.420319946613));
#62686=CARTESIAN_POINT('',(4.5,-4.35,107.319668435864));
#62687=CARTESIAN_POINT('',(13.1748808602028,4.32488086020279,94.9306546266404));
#62688=CARTESIAN_POINT('',(4.5,4.35,107.319668435864));
#62689=CARTESIAN_POINT('',(4.5,-2.25,107.319668435864));
#62690=CARTESIAN_POINT('',(4.42952305344105,4.42047694655895,107.420319946613));
#62691=CARTESIAN_POINT('',(13.7318657725601,-4.88186577256012,94.1351977342719));
#62692=CARTESIAN_POINT('',(4.35904610688211,4.35,107.520971457363));
#62693=CARTESIAN_POINT('',(5.06972007235996,5.06067396547791,106.506023850122));
#62694=CARTESIAN_POINT('',(4.35904610688211,-4.35,107.520971457363));
#62695=CARTESIAN_POINT('',(4.35904610688211,-2.25,107.520971457363));
#62696=CARTESIAN_POINT('',(4.87922001280538,-4.87017390592325,106.778086130459));
#62697=CARTESIAN_POINT('Origin',(12.2143249483705,4.425,104.582070444264));
#62698=CARTESIAN_POINT('',(-1.1517902646357,10.0017902646357,103.512242288186));
#62699=CARTESIAN_POINT('',(3.15,4.35,107.961028252123));
#62700=CARTESIAN_POINT('',(3.15,4.35,107.961028252123));
#62701=CARTESIAN_POINT('',(12.23997645912,4.35,104.652547390823));
#62702=CARTESIAN_POINT('Origin',(4.425,4.425,59.4601776313845));
#62703=CARTESIAN_POINT('',(4.5,4.35,107.113954920906));
#62704=CARTESIAN_POINT('',(4.5,4.35,59.4601776313845));
#62705=CARTESIAN_POINT('',(4.42952305344105,4.42047694655895,107.013303410157));
#62706=CARTESIAN_POINT('',(-3.15184254255455,12.0018425425546,96.1859912458521));
#62707=CARTESIAN_POINT('',(9.87513712229095,-1.02513712229095,103.200243388968));
#62708=CARTESIAN_POINT('Origin',(4.5,-4.5,59.4601776313845));
#62709=CARTESIAN_POINT('',(4.5,-4.35,107.113954920906));
#62710=CARTESIAN_POINT('',(4.5,-4.35,59.4601776313845));
#62711=CARTESIAN_POINT('',(4.5,-2.25,107.113954920906));
#62712=CARTESIAN_POINT('Origin',(4.42952305344106,-2.25,107.013303410157));
#62713=CARTESIAN_POINT('',(4.42952305344105,-4.42047694655895,107.013303410157));
#62714=CARTESIAN_POINT('',(-3.70882745491184,-12.5588274549118,95.3905343534835));
#62715=CARTESIAN_POINT('',(4.35904610688212,-4.35,106.912651899407));
#62716=CARTESIAN_POINT('',(1.86025689264218,-1.85121078575986,103.344011063822));
#62717=CARTESIAN_POINT('',(4.35904610688211,4.35,106.912651899407));
#62718=CARTESIAN_POINT('',(4.35904610688211,-2.25,106.912651899407));
#62719=CARTESIAN_POINT('',(2.05075695219681,2.04171084531453,103.616073344159));
#62720=CARTESIAN_POINT('Origin',(-3.83436137450296,4.425,104.010308791905));
#62721=CARTESIAN_POINT('',(3.15,4.35,106.472595104647));
#62722=CARTESIAN_POINT('',(-3.80870986375353,4.35,103.939831845346));
#62723=CARTESIAN_POINT('',(3.15,4.35,106.472595104647));
#62724=CARTESIAN_POINT('Origin',(4.42952305344106,-2.25,105.535364354459));
#62725=CARTESIAN_POINT('',(4.42952305344105,-4.42047694655895,105.535364354459));
#62726=CARTESIAN_POINT('',(4.5,-4.35,105.43471284371));
#62727=CARTESIAN_POINT('',(12.8416806562944,3.99168065629444,93.5215582415431));
#62728=CARTESIAN_POINT('',(4.5,4.35,105.43471284371));
#62729=CARTESIAN_POINT('',(4.5,-2.25,105.43471284371));
#62730=CARTESIAN_POINT('',(4.42952305344106,4.42047694655894,105.535364354459));
#62731=CARTESIAN_POINT('',(13.3986655686517,-4.54866556865172,92.7261013491746));
#62732=CARTESIAN_POINT('',(4.35904610688211,4.35,105.636015865209));
#62733=CARTESIAN_POINT('',(5.01273948161149,5.00369337472944,104.702444975068));
#62734=CARTESIAN_POINT('',(4.35904610688212,-4.35,105.636015865209));
#62735=CARTESIAN_POINT('',(4.35904610688212,-2.25,105.636015865209));
#62736=CARTESIAN_POINT('',(4.82223942205686,-4.81319331517479,104.974507255406));
#62737=CARTESIAN_POINT('Origin',(11.9114184235091,4.425,102.807363810925));
#62738=CARTESIAN_POINT('',(-0.932106918543077,9.78210691854308,101.781110630985));
#62739=CARTESIAN_POINT('',(3.15,4.35,106.076072659969));
#62740=CARTESIAN_POINT('',(3.15,4.35,106.076072659969));
#62741=CARTESIAN_POINT('',(11.9370699342585,4.35,102.877840757484));
#62742=CARTESIAN_POINT('Origin',(4.425,4.425,59.4601776313845));
#62743=CARTESIAN_POINT('',(4.5,4.35,105.228999328752));
#62744=CARTESIAN_POINT('',(4.5,4.35,59.4601776313845));
#62745=CARTESIAN_POINT('',(4.42952305344105,4.42047694655895,105.128347818003));
#62746=CARTESIAN_POINT('',(-2.81864233864633,11.6686423386463,94.7768948607546));
#62747=CARTESIAN_POINT('',(9.65545377619829,-0.805453776198292,101.469111731766));
#62748=CARTESIAN_POINT('Origin',(4.5,-4.5,59.4601776313845));
#62749=CARTESIAN_POINT('',(4.5,-4.35,105.228999328752));
#62750=CARTESIAN_POINT('',(4.5,-4.35,59.4601776313845));
#62751=CARTESIAN_POINT('',(4.5,-2.25,105.228999328752));
#62752=CARTESIAN_POINT('Origin',(4.42952305344106,-2.25,105.128347818003));
#62753=CARTESIAN_POINT('',(4.42952305344105,-4.42047694655895,105.128347818003));
#62754=CARTESIAN_POINT('',(-3.37562725100355,-12.2256272510036,93.9814379683861));
#62755=CARTESIAN_POINT('',(4.35904610688212,-4.35,105.027696307254));
#62756=CARTESIAN_POINT('',(1.91723748339086,-1.90819137650842,101.540432188768));
#62757=CARTESIAN_POINT('',(4.35904610688212,4.35,105.027696307254));
#62758=CARTESIAN_POINT('',(4.35904610688212,-2.25,105.027696307254));
#62759=CARTESIAN_POINT('',(2.10773754294547,2.09869143606306,101.812494469106));
#62760=CARTESIAN_POINT('Origin',(-3.53145484964149,4.425,102.235602158566));
#62761=CARTESIAN_POINT('',(3.15,4.35,104.587639512493));
#62762=CARTESIAN_POINT('',(-3.50580333889206,4.35,102.165125212007));
#62763=CARTESIAN_POINT('',(3.15,4.35,104.587639512493));
#62764=CARTESIAN_POINT('Origin',(4.42952305344106,-2.25,103.650408762305));
#62765=CARTESIAN_POINT('',(4.42952305344105,-4.42047694655894,103.650408762305));
#62766=CARTESIAN_POINT('',(4.5,-4.35,103.549757251556));
#62767=CARTESIAN_POINT('',(12.5084804523861,3.65848045238613,92.1124618564469));
#62768=CARTESIAN_POINT('',(4.5,4.35,103.549757251556));
#62769=CARTESIAN_POINT('',(4.5,-2.25,103.549757251556));
#62770=CARTESIAN_POINT('',(4.42952305344106,4.42047694655894,103.650408762305));
#62771=CARTESIAN_POINT('',(13.0654653647434,-4.21546536474341,91.3170049640784));
#62772=CARTESIAN_POINT('',(4.35904610688211,4.35,103.751060273055));
#62773=CARTESIAN_POINT('',(4.95575889086306,4.94671278398101,102.898866100015));
#62774=CARTESIAN_POINT('',(4.35904610688212,-4.35,103.751060273055));
#62775=CARTESIAN_POINT('',(4.35904610688212,-2.25,103.751060273055));
#62776=CARTESIAN_POINT('',(4.76525883130843,-4.75621272442636,103.170928380352));
#62777=CARTESIAN_POINT('Origin',(11.6085118986476,4.425,101.032657177585));
#62778=CARTESIAN_POINT('',(-0.712423572449715,9.56242357244971,100.049978973785));
#62779=CARTESIAN_POINT('',(3.15,4.35,104.191117067815));
#62780=CARTESIAN_POINT('',(3.15,4.35,104.191117067815));
#62781=CARTESIAN_POINT('',(11.634163409397,4.35,101.103134124144));
#62782=CARTESIAN_POINT('Origin',(4.425,4.425,59.4601776313845));
#62783=CARTESIAN_POINT('',(4.5,4.35,103.344043736599));
#62784=CARTESIAN_POINT('',(4.5,4.35,59.4601776313845));
#62785=CARTESIAN_POINT('',(4.42952305344105,4.42047694655894,103.243392225849));
#62786=CARTESIAN_POINT('',(-2.48544213473794,11.3354421347379,93.3677984756598));
#62787=CARTESIAN_POINT('',(9.43577043010417,-0.585770430104168,99.7379800745673));
#62788=CARTESIAN_POINT('Origin',(4.5,-4.5,59.4601776313845));
#62789=CARTESIAN_POINT('',(4.5,-4.35,103.344043736599));
#62790=CARTESIAN_POINT('',(4.5,-4.35,59.4601776313845));
#62791=CARTESIAN_POINT('',(4.5,-2.25,103.344043736599));
#62792=CARTESIAN_POINT('Origin',(4.42952305344106,-2.25,103.243392225849));
#62793=CARTESIAN_POINT('',(4.42952305344105,-4.42047694655895,103.243392225849));
#62794=CARTESIAN_POINT('',(-3.04242704709522,-11.8924270470952,92.5723415832913));
#62795=CARTESIAN_POINT('',(4.35904610688211,-4.35,103.1427407151));
#62796=CARTESIAN_POINT('',(1.97421807413904,-1.96517196725673,99.7368533137148));
#62797=CARTESIAN_POINT('',(4.35904610688211,4.35,103.1427407151));
#62798=CARTESIAN_POINT('',(4.35904610688211,-2.25,103.1427407151));
#62799=CARTESIAN_POINT('',(2.16471813369367,2.15567202681139,100.008915594052));
#62800=CARTESIAN_POINT('Origin',(-3.22854832478001,4.425,100.460895525226));
#62801=CARTESIAN_POINT('',(3.15,4.35,102.702683920339));
#62802=CARTESIAN_POINT('',(-3.20289681403059,4.35,100.390418578667));
#62803=CARTESIAN_POINT('',(3.15,4.35,102.702683920339));
#62804=CARTESIAN_POINT('Origin',(4.42952305344106,-2.25,101.765453170152));
#62805=CARTESIAN_POINT('',(4.42952305344105,-4.42047694655895,101.765453170152));
#62806=CARTESIAN_POINT('',(4.5,-4.35,101.664801659402));
#62807=CARTESIAN_POINT('',(12.1752802484778,3.32528024847783,90.703365471351));
#62808=CARTESIAN_POINT('',(4.5,4.35,101.664801659402));
#62809=CARTESIAN_POINT('',(4.5,-2.25,101.664801659402));
#62810=CARTESIAN_POINT('',(4.42952305344106,4.42047694655895,101.765453170152));
#62811=CARTESIAN_POINT('',(12.7322651608351,-3.88226516083512,89.9079085789825));
#62812=CARTESIAN_POINT('',(4.35904610688211,4.35,101.866104680901));
#62813=CARTESIAN_POINT('',(4.8987783001146,4.88973219323253,101.095287224962));
#62814=CARTESIAN_POINT('',(4.35904610688211,-4.35,101.866104680901));
#62815=CARTESIAN_POINT('',(4.35904610688211,-2.25,101.866104680901));
#62816=CARTESIAN_POINT('',(4.70827824055998,-4.69923213367789,101.367349505299));
#62817=CARTESIAN_POINT('Origin',(11.305605373786,4.425,99.2579505442463));
#62818=CARTESIAN_POINT('',(-0.492740226356329,9.34274022635633,98.3188473165849));
#62819=CARTESIAN_POINT('',(3.15,4.35,102.306161475662));
#62820=CARTESIAN_POINT('',(3.15,4.35,102.306161475662));
#62821=CARTESIAN_POINT('',(11.3312568845354,4.35,99.3284274908053));
#62822=CARTESIAN_POINT('Origin',(4.425,4.425,59.4601776313845));
#62823=CARTESIAN_POINT('',(4.5,4.35,101.459088144445));
#62824=CARTESIAN_POINT('',(4.5,4.35,59.4601776313845));
#62825=CARTESIAN_POINT('',(4.42952305344105,4.42047694655894,101.358436633695));
#62826=CARTESIAN_POINT('',(-2.15224193082962,11.0022419308296,91.9587020905637));
#62827=CARTESIAN_POINT('',(9.2160870840108,-0.366087084010803,98.0068484173671));
#62828=CARTESIAN_POINT('Origin',(4.5,-4.5,59.4601776313845));
#62829=CARTESIAN_POINT('',(4.5,-4.35,101.459088144445));
#62830=CARTESIAN_POINT('',(4.5,-4.35,59.4601776313845));
#62831=CARTESIAN_POINT('',(4.5,-2.25,101.459088144445));
#62832=CARTESIAN_POINT('Origin',(4.42952305344106,-2.25,101.358436633695));
#62833=CARTESIAN_POINT('',(4.42952305344105,-4.42047694655895,101.358436633695));
#62834=CARTESIAN_POINT('',(-2.70922684318691,-11.5592268431869,91.1632451981952));
#62835=CARTESIAN_POINT('',(4.35904610688212,-4.35,101.257785122946));
#62836=CARTESIAN_POINT('',(2.03119866488751,-2.02215255800518,97.9332744386614));
#62837=CARTESIAN_POINT('',(4.35904610688211,4.35,101.257785122946));
#62838=CARTESIAN_POINT('',(4.35904610688211,-2.25,101.257785122946));
#62839=CARTESIAN_POINT('',(2.22169872444213,2.21265261755984,98.2053367189986));
#62840=CARTESIAN_POINT('Origin',(-2.92564179991839,4.425,98.6861888918872));
#62841=CARTESIAN_POINT('',(3.15,4.35,100.817728328185));
#62842=CARTESIAN_POINT('',(-2.89999028916897,4.35,98.6157119453282));
#62843=CARTESIAN_POINT('',(3.15,4.35,100.817728328185));
#62844=CARTESIAN_POINT('Origin',(4.42952305344105,-2.25,99.8804975779977));
#62845=CARTESIAN_POINT('',(4.42952305344105,-4.42047694655895,99.8804975779977));
#62846=CARTESIAN_POINT('',(11.8420800445696,2.99208004456955,89.2942690862559));
#62847=CARTESIAN_POINT('',(4.35904610688211,4.35,99.9811490887472));
#62848=CARTESIAN_POINT('',(4.8417977093661,4.83275160248406,99.2917083499081));
#62849=CARTESIAN_POINT('',(4.35904610688211,-4.35,99.9811490887472));
#62850=CARTESIAN_POINT('',(4.35904610688211,-2.25,99.9811490887472));
#62851=CARTESIAN_POINT('',(4.65129764981156,-4.64225154292948,99.5637706302452));
#62852=CARTESIAN_POINT('Origin',(7.02909885190681,-4.425,98.9295160327017));
#62853=CARTESIAN_POINT('',(3.15,-4.35,100.421205883508));
#62854=CARTESIAN_POINT('',(7.05475036265623,-4.35,98.9999929792607));
#62855=CARTESIAN_POINT('',(3.,-4.5,100.316174752776));
#62856=CARTESIAN_POINT('',(3.,-4.5,100.316174752776));
#62857=CARTESIAN_POINT('',(4.35,-4.5,99.8248149365169));
#62858=CARTESIAN_POINT('',(7.00344734115739,-4.5,98.8590390861428));
#62859=CARTESIAN_POINT('',(-0.867547611407954,-9.71754761140796,96.1714487680417));
#62860=CARTESIAN_POINT('Origin',(4.55,0.,99.911647555535));
#62861=CARTESIAN_POINT('',(3.15,4.35,100.421205883508));
#62862=CARTESIAN_POINT('',(11.0283503596739,4.35,97.5537208574659));
#62863=CARTESIAN_POINT('',(3.15,0.,100.421205883508));
#62864=CARTESIAN_POINT('Origin',(11.0026988489245,4.425,97.483243910907));
#62865=CARTESIAN_POINT('',(3.15,4.35,100.421205883508));
#62866=CARTESIAN_POINT('Origin',(3.075,4.425,79.9406917574461));
#62867=CARTESIAN_POINT('',(3.15,4.35,79.9406917574461));
#62868=CARTESIAN_POINT('Origin',(3.15,0.,100.421205883508));
#62869=CARTESIAN_POINT('',(3.15,-4.35,100.817728328185));
#62870=CARTESIAN_POINT('',(3.15,0.,100.817728328185));
#62871=CARTESIAN_POINT('',(3.15,-4.35,79.9406917574461));
#62872=CARTESIAN_POINT('Origin',(3.15,0.,100.817728328185));
#62873=CARTESIAN_POINT('',(-6.87359028618667,-4.35,97.1694398235335));
#62874=CARTESIAN_POINT('Origin',(3.075,4.425,80.883169553523));
#62875=CARTESIAN_POINT('',(3.15,4.35,80.883169553523));
#62876=CARTESIAN_POINT('Origin',(4.55,0.,101.796603147689));
#62877=CARTESIAN_POINT('',(3.15,-4.35,102.306161475662));
#62878=CARTESIAN_POINT('',(3.15,0.,102.306161475662));
#62879=CARTESIAN_POINT('',(7.3576568875177,-4.35,100.7746996126));
#62880=CARTESIAN_POINT('Origin',(3.15,0.,102.306161475662));
#62881=CARTESIAN_POINT('',(3.15,-4.35,102.702683920339));
#62882=CARTESIAN_POINT('',(3.15,0.,102.702683920339));
#62883=CARTESIAN_POINT('',(3.15,-4.35,80.883169553523));
#62884=CARTESIAN_POINT('Origin',(3.15,0.,102.702683920339));
#62885=CARTESIAN_POINT('',(-7.17649681104826,-4.35,98.9441464568727));
#62886=CARTESIAN_POINT('Origin',(3.075,4.425,81.8256473496));
#62887=CARTESIAN_POINT('',(3.15,4.35,81.8256473496));
#62888=CARTESIAN_POINT('Origin',(4.55,0.,103.681558739843));
#62889=CARTESIAN_POINT('',(3.15,-4.35,104.191117067815));
#62890=CARTESIAN_POINT('',(3.15,0.,104.191117067815));
#62891=CARTESIAN_POINT('',(7.66056341237934,-4.35,102.549406245939));
#62892=CARTESIAN_POINT('Origin',(3.15,0.,104.191117067815));
#62893=CARTESIAN_POINT('',(3.15,-4.35,104.587639512493));
#62894=CARTESIAN_POINT('',(3.15,0.,104.587639512493));
#62895=CARTESIAN_POINT('',(3.15,-4.35,81.8256473496));
#62896=CARTESIAN_POINT('Origin',(3.15,0.,104.587639512493));
#62897=CARTESIAN_POINT('',(-7.47940333590974,-4.35,100.718853090212));
#62898=CARTESIAN_POINT('Origin',(3.075,4.425,82.7681251456769));
#62899=CARTESIAN_POINT('',(3.15,4.35,82.7681251456769));
#62900=CARTESIAN_POINT('Origin',(4.55,0.,105.566514331997));
#62901=CARTESIAN_POINT('',(3.15,-4.35,106.076072659969));
#62902=CARTESIAN_POINT('',(3.15,0.,106.076072659969));
#62903=CARTESIAN_POINT('',(7.96346993724081,-4.35,104.324112879278));
#62904=CARTESIAN_POINT('Origin',(3.15,0.,106.076072659969));
#62905=CARTESIAN_POINT('',(3.15,-4.35,106.472595104647));
#62906=CARTESIAN_POINT('',(3.15,0.,106.472595104647));
#62907=CARTESIAN_POINT('',(3.15,-4.35,82.7681251456769));
#62908=CARTESIAN_POINT('Origin',(3.15,0.,106.472595104647));
#62909=CARTESIAN_POINT('',(-7.78230986077121,-4.35,102.493559723551));
#62910=CARTESIAN_POINT('Origin',(3.075,4.425,83.7106029417538));
#62911=CARTESIAN_POINT('',(3.15,4.35,83.7106029417538));
#62912=CARTESIAN_POINT('Origin',(4.55,0.,107.451469924151));
#62913=CARTESIAN_POINT('',(3.15,-4.35,107.961028252123));
#62914=CARTESIAN_POINT('',(3.15,0.,107.961028252123));
#62915=CARTESIAN_POINT('',(8.26637646210229,-4.35,106.098819512618));
#62916=CARTESIAN_POINT('Origin',(3.15,0.,107.961028252123));
#62917=CARTESIAN_POINT('',(3.15,-4.35,108.357550696801));
#62918=CARTESIAN_POINT('',(3.15,0.,108.357550696801));
#62919=CARTESIAN_POINT('',(3.15,-4.35,83.7106029417538));
#62920=CARTESIAN_POINT('Origin',(3.15,0.,108.357550696801));
#62921=CARTESIAN_POINT('',(-8.08521638563253,-4.35,104.268266356891));
#62922=CARTESIAN_POINT('Origin',(3.075,4.425,84.6530807378308));
#62923=CARTESIAN_POINT('',(3.15,4.35,84.6530807378308));
#62924=CARTESIAN_POINT('Origin',(4.55,0.,109.336425516304));
#62925=CARTESIAN_POINT('',(3.15,-4.35,109.845983844277));
#62926=CARTESIAN_POINT('',(3.15,0.,109.845983844277));
#62927=CARTESIAN_POINT('',(8.56928298696376,-4.35,107.873526145957));
#62928=CARTESIAN_POINT('Origin',(3.15,0.,109.845983844277));
#62929=CARTESIAN_POINT('',(3.15,-4.35,110.242506288955));
#62930=CARTESIAN_POINT('',(3.15,0.,110.242506288955));
#62931=CARTESIAN_POINT('',(3.15,-4.35,84.6530807378308));
#62932=CARTESIAN_POINT('Origin',(3.15,0.,110.242506288955));
#62933=CARTESIAN_POINT('',(-8.38812291049415,-4.35,106.04297299023));
#62934=CARTESIAN_POINT('Origin',(3.075,4.425,85.5955585339077));
#62935=CARTESIAN_POINT('',(5.64277347156452,1.85722652843546,110.38200310527));
#62936=CARTESIAN_POINT('',(3.15,4.35,85.5955585339077));
#62937=CARTESIAN_POINT('Origin',(4.55,0.,111.221381108458));
#62938=CARTESIAN_POINT('',(3.15,-4.35,111.730939436431));
#62939=CARTESIAN_POINT('',(3.15,0.,111.730939436431));
#62940=CARTESIAN_POINT('',(8.87218951182523,-4.35,109.648232779296));
#62941=CARTESIAN_POINT('Origin',(3.15,0.,111.730939436431));
#62942=CARTESIAN_POINT('',(3.15,-4.35,85.5955585339077));
#62943=CARTESIAN_POINT('Origin',(-4.74308094908738,4.425,109.334428691923));
#62944=CARTESIAN_POINT('',(10.5341871605711,-1.68418716057113,108.393638360568));
#62945=CARTESIAN_POINT('Origin',(-10.8370266201352,-4.425,120.311103003503));
#62946=CARTESIAN_POINT('',(4.35,-4.5,125.918541973177));
#62947=CARTESIAN_POINT('',(11.4774798520793,2.62747985207928,120.927826852313));
#62948=CARTESIAN_POINT('',(3.,-4.5,125.427182156917));
#62949=CARTESIAN_POINT('',(-10.8626781308846,-4.5,120.381579950062));
#62950=CARTESIAN_POINT('',(3.,-4.5,125.427182156917));
#62951=CARTESIAN_POINT('Origin',(3.075,-4.425,92.1929031064463));
#62952=CARTESIAN_POINT('',(3.,-4.5,124.820597450777));
#62953=CARTESIAN_POINT('',(3.,-4.5,92.1929031064463));
#62954=CARTESIAN_POINT('',(3.,-4.5,124.820597450777));
#62955=CARTESIAN_POINT('Origin',(10.9668836751061,-4.425,122.000702266112));
#62956=CARTESIAN_POINT('',(4.35,-4.5,124.329237634517));
#62957=CARTESIAN_POINT('',(10.9412321643567,-4.5,121.930225319553));
#62958=CARTESIAN_POINT('',(-3.72343111062165,-12.5734311106217,118.676160311644));
#62959=CARTESIAN_POINT('Origin',(-4.5,-4.5,59.4601776313845));
#62960=CARTESIAN_POINT('',(4.35,-4.5,126.214193226671));
#62961=CARTESIAN_POINT('',(4.35,-4.5,59.4601776313845));
#62962=CARTESIAN_POINT('',(3.,-4.5,126.705553042931));
#62963=CARTESIAN_POINT('',(11.2441386892182,-4.5,123.704931952893));
#62964=CARTESIAN_POINT('',(3.,-4.5,127.312137749071));
#62965=CARTESIAN_POINT('',(3.,-4.5,93.1353809025232));
#62966=CARTESIAN_POINT('',(4.35,-4.5,127.80349756533));
#62967=CARTESIAN_POINT('',(-11.1655846557463,-4.5,122.156286583401));
#62968=CARTESIAN_POINT('',(4.35,-4.5,128.099148818825));
#62969=CARTESIAN_POINT('',(4.35,-4.5,59.4601776313845));
#62970=CARTESIAN_POINT('',(2.99999999999999,-4.5,128.590508635084));
#62971=CARTESIAN_POINT('',(11.5470452140794,-4.5,125.479638586232));
#62972=CARTESIAN_POINT('',(3.,-4.5,129.197093341225));
#62973=CARTESIAN_POINT('',(3.,-4.5,94.0778586986002));
#62974=CARTESIAN_POINT('',(4.35,-4.5,129.688453157484));
#62975=CARTESIAN_POINT('',(-11.4684911806075,-4.5,123.930993216741));
#62976=CARTESIAN_POINT('',(4.35,-4.5,59.4601776313845));
#62977=CARTESIAN_POINT('',(4.35,-4.5,59.9101776313845));
#62978=CARTESIAN_POINT('',(-3.375,-4.5,59.9101776313845));
#62979=CARTESIAN_POINT('',(4.35,-4.5,59.4601776313845));
#62980=CARTESIAN_POINT('',(3.,-4.5,70.7634699844547));
#62981=CARTESIAN_POINT('',(3.,-4.5,64.8610470202151));
#62982=CARTESIAN_POINT('',(4.35,-4.5,71.2548298007141));
#62983=CARTESIAN_POINT('',(-2.07838890990205,-4.5,68.9150875832228));
#62984=CARTESIAN_POINT('',(4.35,-4.5,71.5504810542087));
#62985=CARTESIAN_POINT('',(4.35,-4.5,59.4601776313845));
#62986=CARTESIAN_POINT('',(3.,-4.5,72.0418408704681));
#62987=CARTESIAN_POINT('',(2.45984946823538,-4.5,72.2384395860535));
#62988=CARTESIAN_POINT('',(3.,-4.5,72.6484255766087));
#62989=CARTESIAN_POINT('',(3.,-4.5,65.803524816292));
#62990=CARTESIAN_POINT('',(4.35,-4.5,73.139785392868));
#62991=CARTESIAN_POINT('',(-2.38129543476353,-4.5,70.6897942165621));
#62992=CARTESIAN_POINT('',(4.35,-4.5,73.4354366463626));
#62993=CARTESIAN_POINT('',(4.35,-4.5,59.4601776313845));
#62994=CARTESIAN_POINT('',(3.,-4.5,73.926796462622));
#62995=CARTESIAN_POINT('',(2.76275599309685,-4.5,74.0131462193928));
#62996=CARTESIAN_POINT('',(3.,-4.5,66.746002612369));
#62997=CARTESIAN_POINT('',(3.,-4.5,75.8117520547759));
#62998=CARTESIAN_POINT('',(3.06566251795832,-4.5,75.7878528527321));
#62999=CARTESIAN_POINT('',(3.,-4.5,76.4183367609164));
#63000=CARTESIAN_POINT('',(3.,-4.5,67.6884804084459));
#63001=CARTESIAN_POINT('',(4.35,-4.5,76.9096965771758));
#63002=CARTESIAN_POINT('',(-2.98710848448645,-4.5,74.2392074832407));
#63003=CARTESIAN_POINT('',(4.35,-4.5,77.2053478306704));
#63004=CARTESIAN_POINT('',(4.35,-4.5,59.4601776313845));
#63005=CARTESIAN_POINT('',(3.,-4.5,77.6967076469297));
#63006=CARTESIAN_POINT('',(3.36856904281978,-4.5,77.5625594860714));
#63007=CARTESIAN_POINT('',(3.,-4.5,68.6309582045228));
#63008=CARTESIAN_POINT('',(4.35,-4.5,79.0903034228242));
#63009=CARTESIAN_POINT('',(4.35,-4.5,59.4601776313845));
#63010=CARTESIAN_POINT('',(3.,-4.5,79.5816632390836));
#63011=CARTESIAN_POINT('',(3.67147556768125,-4.5,79.3372661194106));
#63012=CARTESIAN_POINT('',(3.,-4.5,80.1882479452242));
#63013=CARTESIAN_POINT('',(3.,-4.5,69.5734360005998));
#63014=CARTESIAN_POINT('',(4.35,-4.5,80.6796077614835));
#63015=CARTESIAN_POINT('',(-3.59292153420939,-4.5,77.7886207499193));
#63016=CARTESIAN_POINT('',(4.35,-4.5,80.9752590149781));
#63017=CARTESIAN_POINT('',(4.35,-4.5,59.4601776313845));
#63018=CARTESIAN_POINT('',(3.,-4.5,81.4666188312375));
#63019=CARTESIAN_POINT('',(3.97438209254272,-4.5,81.1119727527499));
#63020=CARTESIAN_POINT('',(3.,-4.5,82.073203537378));
#63021=CARTESIAN_POINT('',(3.,-4.5,70.5159137966767));
#63022=CARTESIAN_POINT('',(4.35,-4.5,82.5645633536374));
#63023=CARTESIAN_POINT('',(-3.89582805907085,-4.5,79.5633273832586));
#63024=CARTESIAN_POINT('',(4.35,-4.5,59.4601776313845));
#63025=CARTESIAN_POINT('',(3.,-4.5,83.9581591295319));
#63026=CARTESIAN_POINT('',(3.,-4.5,71.4583915927537));
#63027=CARTESIAN_POINT('',(4.35,-4.5,84.4495189457913));
#63028=CARTESIAN_POINT('',(-4.19873458393231,-4.5,81.3380340165978));
#63029=CARTESIAN_POINT('',(4.35,-4.5,84.7451701992859));
#63030=CARTESIAN_POINT('',(4.35,-4.5,59.4601776313845));
#63031=CARTESIAN_POINT('',(3.,-4.5,85.2365300155452));
#63032=CARTESIAN_POINT('',(4.58019514226565,-4.5,84.6613860194285));
#63033=CARTESIAN_POINT('',(3.,-4.5,85.8431147216858));
#63034=CARTESIAN_POINT('',(3.,-4.5,72.4008693888306));
#63035=CARTESIAN_POINT('',(4.35,-4.5,86.3344745379451));
#63036=CARTESIAN_POINT('',(-4.50164110879379,-4.5,83.1127406499371));
#63037=CARTESIAN_POINT('',(4.35,-4.5,86.6301257914398));
#63038=CARTESIAN_POINT('',(4.35,-4.5,59.4601776313845));
#63039=CARTESIAN_POINT('',(3.,-4.5,87.1214856076991));
#63040=CARTESIAN_POINT('',(4.88310166712712,-4.5,86.4360926527678));
#63041=CARTESIAN_POINT('',(3.,-4.5,73.3433471849075));
#63042=CARTESIAN_POINT('',(3.,-4.5,89.006441199853));
#63043=CARTESIAN_POINT('',(5.18600819198858,-4.5,88.2107992861071));
#63044=CARTESIAN_POINT('',(3.,-4.5,89.6130259059935));
#63045=CARTESIAN_POINT('',(3.,-4.5,74.2858249809845));
#63046=CARTESIAN_POINT('',(4.35,-4.5,90.1043857222529));
#63047=CARTESIAN_POINT('',(-5.10745415851671,-4.5,86.6621539166157));
#63048=CARTESIAN_POINT('',(4.35,-4.5,90.4000369757475));
#63049=CARTESIAN_POINT('',(4.35,-4.5,59.4601776313845));
#63050=CARTESIAN_POINT('',(2.99999999999999,-4.5,90.8913967920069));
#63051=CARTESIAN_POINT('',(5.48891471685005,-4.5,89.9855059194464));
#63052=CARTESIAN_POINT('',(3.,-4.5,91.4979814981474));
#63053=CARTESIAN_POINT('',(3.,-4.5,75.2283027770614));
#63054=CARTESIAN_POINT('',(4.35,-4.5,91.9893413144068));
#63055=CARTESIAN_POINT('',(-5.41036068337819,-4.5,88.436860549955));
#63056=CARTESIAN_POINT('',(4.35,-4.5,92.2849925679014));
#63057=CARTESIAN_POINT('',(4.35,-4.5,59.4601776313845));
#63058=CARTESIAN_POINT('',(3.,-4.5,92.7763523841608));
#63059=CARTESIAN_POINT('',(5.79182124171152,-4.5,91.7602125527857));
#63060=CARTESIAN_POINT('',(3.,-4.5,93.3829370903013));
#63061=CARTESIAN_POINT('',(3.,-4.5,76.1707805731383));
#63062=CARTESIAN_POINT('',(4.35,-4.5,93.8742969065607));
#63063=CARTESIAN_POINT('',(-5.71326720823965,-4.5,90.2115671832943));
#63064=CARTESIAN_POINT('',(4.35,-4.5,94.1699481600552));
#63065=CARTESIAN_POINT('',(4.35,-4.5,59.4601776313845));
#63066=CARTESIAN_POINT('',(3.,-4.5,94.6613079763146));
#63067=CARTESIAN_POINT('',(6.09472776657299,-4.5,93.5349191861249));
#63068=CARTESIAN_POINT('',(3.,-4.5,77.1132583692153));
#63069=CARTESIAN_POINT('',(4.35,-4.5,96.0549037522091));
#63070=CARTESIAN_POINT('',(4.35,-4.5,59.4601776313845));
#63071=CARTESIAN_POINT('',(2.99999999999999,-4.5,96.5462635684685));
#63072=CARTESIAN_POINT('',(6.39763429143445,-4.5,95.3096258194642));
#63073=CARTESIAN_POINT('',(3.,-4.5,97.152848274609));
#63074=CARTESIAN_POINT('',(3.,-4.5,78.0557361652922));
#63075=CARTESIAN_POINT('',(4.35,-4.5,97.6442080908684));
#63076=CARTESIAN_POINT('',(-6.31908025796259,-4.5,93.7609804499728));
#63077=CARTESIAN_POINT('',(4.35,-4.5,97.939859344363));
#63078=CARTESIAN_POINT('',(4.35,-4.5,59.4601776313845));
#63079=CARTESIAN_POINT('',(3.,-4.5,98.4312191606224));
#63080=CARTESIAN_POINT('',(6.70054081629591,-4.5,97.0843324528035));
#63081=CARTESIAN_POINT('',(3.,-4.5,99.0378038667629));
#63082=CARTESIAN_POINT('',(3.,-4.5,78.9982139613691));
#63083=CARTESIAN_POINT('',(4.35,-4.5,99.5291636830223));
#63084=CARTESIAN_POINT('',(-6.62198678282405,-4.5,95.5356870833121));
#63085=CARTESIAN_POINT('',(4.35,-4.5,59.4601776313845));
#63086=CARTESIAN_POINT('',(3.,-4.5,100.922759458917));
#63087=CARTESIAN_POINT('',(3.,-4.5,79.9406917574461));
#63088=CARTESIAN_POINT('',(4.35,-4.5,101.414119275176));
#63089=CARTESIAN_POINT('',(-6.92489330768551,-4.5,97.3103937166514));
#63090=CARTESIAN_POINT('',(4.35,-4.5,101.709770528671));
#63091=CARTESIAN_POINT('',(4.35,-4.5,59.4601776313845));
#63092=CARTESIAN_POINT('',(3.,-4.5,102.20113034493));
#63093=CARTESIAN_POINT('',(7.30635386601885,-4.5,100.633745719482));
#63094=CARTESIAN_POINT('',(3.,-4.5,102.807715051071));
#63095=CARTESIAN_POINT('',(3.,-4.5,80.883169553523));
#63096=CARTESIAN_POINT('',(4.35,-4.5,103.29907486733));
#63097=CARTESIAN_POINT('',(-7.22779983254711,-4.5,99.0851003499905));
#63098=CARTESIAN_POINT('',(4.35,-4.5,103.594726120825));
#63099=CARTESIAN_POINT('',(4.35,-4.5,59.4601776313845));
#63100=CARTESIAN_POINT('',(3.,-4.5,104.086085937084));
#63101=CARTESIAN_POINT('',(7.60926039088049,-4.5,102.408452352821));
#63102=CARTESIAN_POINT('',(3.,-4.5,104.692670643225));
#63103=CARTESIAN_POINT('',(3.,-4.5,81.8256473496));
#63104=CARTESIAN_POINT('',(4.35,-4.5,105.184030459484));
#63105=CARTESIAN_POINT('',(-7.53070635740859,-4.5,100.85980698333));
#63106=CARTESIAN_POINT('',(4.35,-4.5,105.479681712979));
#63107=CARTESIAN_POINT('',(4.35,-4.5,59.4601776313845));
#63108=CARTESIAN_POINT('',(3.,-4.5,105.971041529238));
#63109=CARTESIAN_POINT('',(7.91216691574196,-4.5,104.183158986161));
#63110=CARTESIAN_POINT('',(3.,-4.5,106.577626235378));
#63111=CARTESIAN_POINT('',(3.,-4.5,82.7681251456769));
#63112=CARTESIAN_POINT('',(4.35,-4.5,107.068986051638));
#63113=CARTESIAN_POINT('',(-7.83361288227006,-4.5,102.634513616669));
#63114=CARTESIAN_POINT('',(4.35,-4.5,107.364637305132));
#63115=CARTESIAN_POINT('',(4.35,-4.5,59.4601776313845));
#63116=CARTESIAN_POINT('',(3.,-4.5,107.855997121392));
#63117=CARTESIAN_POINT('',(8.21507344060344,-4.5,105.9578656195));
#63118=CARTESIAN_POINT('',(3.,-4.5,108.462581827532));
#63119=CARTESIAN_POINT('',(3.,-4.5,83.7106029417538));
#63120=CARTESIAN_POINT('',(4.35,-4.5,108.953941643792));
#63121=CARTESIAN_POINT('',(-8.13651940713138,-4.5,104.409220250009));
#63122=CARTESIAN_POINT('',(4.35,-4.5,109.249592897286));
#63123=CARTESIAN_POINT('',(4.35,-4.5,59.4601776313845));
#63124=CARTESIAN_POINT('',(3.,-4.5,109.740952713546));
#63125=CARTESIAN_POINT('',(8.51797996546491,-4.5,107.732572252839));
#63126=CARTESIAN_POINT('',(3.,-4.5,110.347537419686));
#63127=CARTESIAN_POINT('',(3.,-4.5,84.6530807378308));
#63128=CARTESIAN_POINT('',(4.35,-4.5,110.838897235946));
#63129=CARTESIAN_POINT('',(-8.43942593199301,-4.5,106.183926883348));
#63130=CARTESIAN_POINT('',(4.35,-4.5,111.13454848944));
#63131=CARTESIAN_POINT('',(4.35,-4.5,59.4601776313845));
#63132=CARTESIAN_POINT('',(3.,-4.5,111.6259083057));
#63133=CARTESIAN_POINT('',(8.82088649032638,-4.5,109.507278886178));
#63134=CARTESIAN_POINT('',(3.,-4.5,85.5955585339077));
#63135=CARTESIAN_POINT('',(3.,-4.5,114.117448603994));
#63136=CARTESIAN_POINT('',(3.,-4.5,86.5380363299847));
#63137=CARTESIAN_POINT('',(4.35,-4.5,114.608808420253));
#63138=CARTESIAN_POINT('',(-9.04523898171578,-4.5,109.733340150026));
#63139=CARTESIAN_POINT('',(4.35,-4.5,114.904459673748));
#63140=CARTESIAN_POINT('',(4.35,-4.5,59.4601776313845));
#63141=CARTESIAN_POINT('',(3.,-4.5,115.395819490007));
#63142=CARTESIAN_POINT('',(9.42669954004933,-4.5,113.056692152857));
#63143=CARTESIAN_POINT('',(3.,-4.5,116.002404196148));
#63144=CARTESIAN_POINT('',(3.,-4.5,87.4805141260616));
#63145=CARTESIAN_POINT('',(4.35,-4.5,116.493764012407));
#63146=CARTESIAN_POINT('',(-9.34814550657743,-4.5,111.508046783366));
#63147=CARTESIAN_POINT('',(4.35,-4.5,116.789415265902));
#63148=CARTESIAN_POINT('',(4.35,-4.5,59.4601776313845));
#63149=CARTESIAN_POINT('',(3.,-4.5,117.280775082161));
#63150=CARTESIAN_POINT('',(9.7296060649108,-4.5,114.831398786196));
#63151=CARTESIAN_POINT('',(3.,-4.5,88.4229919221386));
#63152=CARTESIAN_POINT('',(4.35,-4.5,118.674370858056));
#63153=CARTESIAN_POINT('',(4.35,-4.5,59.4601776313845));
#63154=CARTESIAN_POINT('',(3.,-4.5,119.165730674315));
#63155=CARTESIAN_POINT('',(10.0325125897723,-4.5,116.606105419536));
#63156=CARTESIAN_POINT('',(3.,-4.5,119.772315380456));
#63157=CARTESIAN_POINT('',(3.,-4.5,89.3654697182155));
#63158=CARTESIAN_POINT('',(4.35,-4.5,120.263675196715));
#63159=CARTESIAN_POINT('',(-9.95395855630018,-4.5,115.057460050044));
#63160=CARTESIAN_POINT('',(4.35,-4.5,120.559326450209));
#63161=CARTESIAN_POINT('',(4.35,-4.5,59.4601776313845));
#63162=CARTESIAN_POINT('',(3.,-4.5,121.050686266469));
#63163=CARTESIAN_POINT('',(10.3354191146337,-4.5,118.380812052875));
#63164=CARTESIAN_POINT('',(3.,-4.5,121.657270972609));
#63165=CARTESIAN_POINT('',(3.,-4.5,90.3079475142924));
#63166=CARTESIAN_POINT('',(4.35,-4.5,122.148630788869));
#63167=CARTESIAN_POINT('',(-10.2568650811618,-4.5,116.832166683383));
#63168=CARTESIAN_POINT('',(4.35,-4.5,122.444282042363));
#63169=CARTESIAN_POINT('',(4.35,-4.5,59.4601776313845));
#63170=CARTESIAN_POINT('',(3.,-4.5,122.935641858623));
#63171=CARTESIAN_POINT('',(10.6383256394952,-4.5,120.155518686214));
#63172=CARTESIAN_POINT('',(3.,-4.5,123.542226564763));
#63173=CARTESIAN_POINT('',(3.,-4.5,91.2504253103694));
#63174=CARTESIAN_POINT('',(4.35,-4.5,124.033586381023));
#63175=CARTESIAN_POINT('',(-10.5597716060233,-4.5,118.606873316723));
#63176=CARTESIAN_POINT('',(4.35,-4.5,59.4601776313845));
#63177=CARTESIAN_POINT('',(1.10830535322836E-16,-4.5,60.5551776313845));
#63178=CARTESIAN_POINT('Origin',(0.,-4.5,61.4601776313845));
#63179=CARTESIAN_POINT('Origin',(4.425,-4.425,59.4601776313845));
#63180=CARTESIAN_POINT('',(-3.94311445671589,-12.7931144567159,120.407291968843));
#63181=CARTESIAN_POINT('Origin',(-10.5341200952739,-4.425,118.536396370164));
#63182=CARTESIAN_POINT('',(11.2577965059859,2.4077965059859,119.196695195113));
#63183=CARTESIAN_POINT('',(3.,-4.5,123.542226564763));
#63184=CARTESIAN_POINT('Origin',(3.075,-4.425,91.2504253103694));
#63185=CARTESIAN_POINT('',(3.,-4.5,122.935641858623));
#63186=CARTESIAN_POINT('Origin',(10.6639771502446,-4.425,120.225995632773));
#63187=CARTESIAN_POINT('',(-3.50374776452922,-12.3537477645292,116.945028654443));
#63188=CARTESIAN_POINT('Origin',(4.425,-4.425,59.4601776313845));
#63189=CARTESIAN_POINT('Origin',(-10.2312135704124,-4.425,116.761689736824));
#63190=CARTESIAN_POINT('',(11.0381131598936,2.18811315989359,117.465563537911));
#63191=CARTESIAN_POINT('',(3.,-4.5,121.657270972609));
#63192=CARTESIAN_POINT('Origin',(3.075,-4.425,90.3079475142924));
#63193=CARTESIAN_POINT('',(3.,-4.5,121.050686266469));
#63194=CARTESIAN_POINT('Origin',(10.3610706253832,-4.425,118.451288999434));
#63195=CARTESIAN_POINT('',(-3.28406441843662,-12.1340644184366,115.213896997241));
#63196=CARTESIAN_POINT('Origin',(4.425,-4.425,59.4601776313845));
#63197=CARTESIAN_POINT('Origin',(-9.92830704555076,-4.425,114.986983103485));
#63198=CARTESIAN_POINT('',(10.8184298137991,1.96842981379911,115.734431880713));
#63199=CARTESIAN_POINT('',(3.,-4.5,119.772315380456));
#63200=CARTESIAN_POINT('Origin',(3.075,-4.425,89.3654697182155));
#63201=CARTESIAN_POINT('',(3.,-4.5,119.165730674315));
#63202=CARTESIAN_POINT('Origin',(10.0581641005217,-4.425,116.676582366094));
#63203=CARTESIAN_POINT('',(-3.06438107234234,-11.9143810723423,113.482765340042));
#63204=CARTESIAN_POINT('Origin',(4.425,-4.425,59.4601776313845));
#63205=CARTESIAN_POINT('Origin',(3.075,-4.425,88.4229919221386));
#63206=CARTESIAN_POINT('',(3.,-4.5,117.280775082161));
#63207=CARTESIAN_POINT('Origin',(9.75525757566023,-4.425,114.901875732755));
#63208=CARTESIAN_POINT('',(-2.84469772624895,-11.694697726249,111.751633682842));
#63209=CARTESIAN_POINT('Origin',(4.425,-4.425,59.4601776313845));
#63210=CARTESIAN_POINT('',(4.5,-4.35,59.4601776313845));
#63211=CARTESIAN_POINT('Origin',(-9.322493995828,-4.425,111.437569836807));
#63212=CARTESIAN_POINT('',(10.3790631216133,1.52906312161332,112.272168566311));
#63213=CARTESIAN_POINT('',(3.,-4.5,116.002404196148));
#63214=CARTESIAN_POINT('Origin',(3.075,-4.425,87.4805141260616));
#63215=CARTESIAN_POINT('',(3.,-4.5,115.395819490007));
#63216=CARTESIAN_POINT('Origin',(9.45235105079875,-4.425,113.127169099416));
#63217=CARTESIAN_POINT('',(-2.62501438015637,-11.4750143801564,110.020502025641));
#63218=CARTESIAN_POINT('Origin',(4.425,-4.425,59.4601776313845));
#63219=CARTESIAN_POINT('Origin',(-9.01958747096636,-4.425,109.662863203467));
#63220=CARTESIAN_POINT('',(10.159379775519,1.30937977551898,110.541036909112));
#63221=CARTESIAN_POINT('',(5.13546547427087,-2.36453452572912,112.622179581323));
#63222=CARTESIAN_POINT('Origin',(3.075,-4.425,86.5380363299847));
#63223=CARTESIAN_POINT('Origin',(3.075,-4.425,85.5955585339077));
#63224=CARTESIAN_POINT('',(3.,-4.5,111.6259083057));
#63225=CARTESIAN_POINT('Origin',(8.84653800107581,-4.425,109.577755832737));
#63226=CARTESIAN_POINT('',(-2.18564768796881,-11.0356476879688,106.558238711242));
#63227=CARTESIAN_POINT('Origin',(-8.41377442124358,-4.425,106.113449936789));
#63228=CARTESIAN_POINT('',(9.72001308333303,0.870013083333027,107.078773594711));
#63229=CARTESIAN_POINT('',(3.,-4.5,110.347537419686));
#63230=CARTESIAN_POINT('Origin',(3.075,-4.425,84.6530807378308));
#63231=CARTESIAN_POINT('',(3.,-4.5,109.740952713546));
#63232=CARTESIAN_POINT('Origin',(8.54363147621433,-4.425,107.803049199398));
#63233=CARTESIAN_POINT('',(-1.96596434187612,-10.8159643418761,104.82710705404));
#63234=CARTESIAN_POINT('Origin',(4.425,-4.425,59.4601776313845));
#63235=CARTESIAN_POINT('Origin',(-8.11086789638195,-4.425,104.33874330345));
#63236=CARTESIAN_POINT('',(9.50032973723794,0.650329737237946,105.347641937513));
#63237=CARTESIAN_POINT('',(3.,-4.5,108.462581827532));
#63238=CARTESIAN_POINT('Origin',(3.075,-4.425,83.7106029417538));
#63239=CARTESIAN_POINT('',(3.,-4.5,107.855997121392));
#63240=CARTESIAN_POINT('Origin',(8.24072495135287,-4.425,106.028342566059));
#63241=CARTESIAN_POINT('',(-1.74628099578204,-10.596280995782,103.095975396841));
#63242=CARTESIAN_POINT('Origin',(4.425,-4.425,59.4601776313845));
#63243=CARTESIAN_POINT('Origin',(-7.80796137152063,-4.425,102.56403667011));
#63244=CARTESIAN_POINT('',(9.28064639114536,0.430646391145358,103.616510280312));
#63245=CARTESIAN_POINT('',(3.,-4.5,106.577626235378));
#63246=CARTESIAN_POINT('Origin',(3.075,-4.425,82.7681251456769));
#63247=CARTESIAN_POINT('',(3.,-4.5,105.971041529238));
#63248=CARTESIAN_POINT('Origin',(7.93781842649139,-4.425,104.253635932719));
#63249=CARTESIAN_POINT('',(-1.52659764968865,-10.3765976496886,101.364843739641));
#63250=CARTESIAN_POINT('Origin',(4.425,-4.425,59.4601776313845));
#63251=CARTESIAN_POINT('Origin',(-7.50505484665916,-4.425,100.789330036771));
#63252=CARTESIAN_POINT('',(9.06096304505277,0.210963045052771,101.88537862311));
#63253=CARTESIAN_POINT('',(3.,-4.5,104.692670643225));
#63254=CARTESIAN_POINT('Origin',(3.075,-4.425,81.8256473496));
#63255=CARTESIAN_POINT('',(3.,-4.5,104.086085937084));
#63256=CARTESIAN_POINT('Origin',(7.63491190162991,-4.425,102.47892929938));
#63257=CARTESIAN_POINT('',(-1.30691430359526,-10.1569143035953,99.6337120824411));
#63258=CARTESIAN_POINT('Origin',(4.425,-4.425,59.4601776313845));
#63259=CARTESIAN_POINT('Origin',(-7.20214832179769,-4.425,99.0146234034316));
#63260=CARTESIAN_POINT('',(8.84127969895858,-0.00872030104142052,100.154246965911));
#63261=CARTESIAN_POINT('',(3.,-4.5,102.807715051071));
#63262=CARTESIAN_POINT('Origin',(3.075,-4.425,80.883169553523));
#63263=CARTESIAN_POINT('',(3.,-4.5,102.20113034493));
#63264=CARTESIAN_POINT('Origin',(7.33200537676827,-4.425,100.704222666041));
#63265=CARTESIAN_POINT('',(-1.08723095750194,-9.93723095750194,97.9025804252409));
#63266=CARTESIAN_POINT('Origin',(4.425,-4.425,59.4601776313845));
#63267=CARTESIAN_POINT('Origin',(-6.89924179693609,-4.425,97.2399167700925));
#63268=CARTESIAN_POINT('',(8.62159635286518,-0.22840364713482,98.423115308711));
#63269=CARTESIAN_POINT('',(3.,-4.5,100.922759458917));
#63270=CARTESIAN_POINT('Origin',(3.075,-4.425,79.9406917574461));
#63271=CARTESIAN_POINT('Origin',(4.425,-4.425,59.4601776313845));
#63272=CARTESIAN_POINT('Origin',(-6.59633527207463,-4.425,95.4652101367532));
#63273=CARTESIAN_POINT('',(8.40191300677184,-0.448086993228164,96.6919836515108));
#63274=CARTESIAN_POINT('',(3.,-4.5,99.0378038667629));
#63275=CARTESIAN_POINT('Origin',(3.075,-4.425,78.9982139613691));
#63276=CARTESIAN_POINT('',(3.,-4.5,98.4312191606224));
#63277=CARTESIAN_POINT('Origin',(6.72619232704534,-4.425,97.1548093993624));
#63278=CARTESIAN_POINT('',(-0.647864265315112,-9.49786426531512,94.4403171108406));
#63279=CARTESIAN_POINT('Origin',(4.425,-4.425,59.4601776313845));
#63280=CARTESIAN_POINT('Origin',(-6.29342874721316,-4.425,93.6905035034139));
#63281=CARTESIAN_POINT('',(8.18222966067847,-0.667770339321526,94.9608519943106));
#63282=CARTESIAN_POINT('',(3.,-4.5,97.152848274609));
#63283=CARTESIAN_POINT('Origin',(3.075,-4.425,78.0557361652922));
#63284=CARTESIAN_POINT('',(3.,-4.5,96.5462635684685));
#63285=CARTESIAN_POINT('Origin',(6.42328580218387,-4.425,95.3801027660232));
#63286=CARTESIAN_POINT('',(-0.428180919221253,-9.27818091922125,92.7091854536413));
#63287=CARTESIAN_POINT('Origin',(4.425,-4.425,59.4601776313845));
#63288=CARTESIAN_POINT('Origin',(3.075,-4.425,77.1132583692153));
#63289=CARTESIAN_POINT('',(3.,-4.5,94.6613079763146));
#63290=CARTESIAN_POINT('Origin',(6.12037927732241,-4.425,93.6053961326839));
#63291=CARTESIAN_POINT('',(-0.208497573127868,-9.05849757312787,90.9780537964411));
#63292=CARTESIAN_POINT('Origin',(4.425,-4.425,59.4601776313845));
#63293=CARTESIAN_POINT('',(4.5,-4.35,59.4601776313845));
#63294=CARTESIAN_POINT('Origin',(-5.68761569749023,-4.425,90.1410902367353));
#63295=CARTESIAN_POINT('',(7.74286296849167,-1.10713703150834,91.4985886799104));
#63296=CARTESIAN_POINT('',(3.,-4.5,93.3829370903013));
#63297=CARTESIAN_POINT('Origin',(3.075,-4.425,76.1707805731383));
#63298=CARTESIAN_POINT('',(3.,-4.5,92.7763523841608));
#63299=CARTESIAN_POINT('Origin',(5.81747275246094,-4.425,91.8306894993446));
#63300=CARTESIAN_POINT('',(0.0111857729655158,-8.83881422703448,89.246922139241));
#63301=CARTESIAN_POINT('Origin',(4.425,-4.425,59.4601776313845));
#63302=CARTESIAN_POINT('Origin',(-5.38470917262876,-4.425,88.366383603396));
#63303=CARTESIAN_POINT('',(7.5231796223983,-1.3268203776017,89.7674570227101));
#63304=CARTESIAN_POINT('',(3.,-4.5,91.4979814981474));
#63305=CARTESIAN_POINT('Origin',(3.075,-4.425,75.2283027770614));
#63306=CARTESIAN_POINT('',(3.,-4.5,90.8913967920069));
#63307=CARTESIAN_POINT('Origin',(5.51456622759947,-4.425,90.0559828660053));
#63308=CARTESIAN_POINT('',(0.230869119058417,-8.61913088094158,87.5157904820399));
#63309=CARTESIAN_POINT('Origin',(4.425,-4.425,59.4601776313845));
#63310=CARTESIAN_POINT('Origin',(-5.08180264776729,-4.425,86.5916769700568));
#63311=CARTESIAN_POINT('',(7.30349627630486,-1.54650372369514,88.0363253655101));
#63312=CARTESIAN_POINT('',(3.,-4.5,89.6130259059935));
#63313=CARTESIAN_POINT('Origin',(3.075,-4.425,74.2858249809845));
#63314=CARTESIAN_POINT('',(1.31774799117218,-6.18225200882782,87.8285156621034));
#63315=CARTESIAN_POINT('Origin',(5.21165970273801,-4.425,88.281276232666));
#63316=CARTESIAN_POINT('Origin',(3.075,-4.425,73.3433471849075));
#63317=CARTESIAN_POINT('',(3.,-4.5,87.1214856076991));
#63318=CARTESIAN_POINT('Origin',(4.90875317787654,-4.425,86.5065695993267));
#63319=CARTESIAN_POINT('',(0.670235811245595,-8.1797641887544,84.0535271676404));
#63320=CARTESIAN_POINT('Origin',(-4.47598959804436,-4.425,83.0422637033782));
#63321=CARTESIAN_POINT('',(6.86412958411812,-1.98587041588188,84.5740620511097));
#63322=CARTESIAN_POINT('',(3.,-4.5,85.8431147216858));
#63323=CARTESIAN_POINT('Origin',(3.075,-4.425,72.4008693888306));
#63324=CARTESIAN_POINT('',(3.,-4.5,85.2365300155452));
#63325=CARTESIAN_POINT('Origin',(4.60584665301507,-4.425,84.7318629659874));
#63326=CARTESIAN_POINT('',(0.889919157338593,-7.96008084266141,82.3223955104395));
#63327=CARTESIAN_POINT('Origin',(4.425,-4.425,59.4601776313845));
#63328=CARTESIAN_POINT('Origin',(-4.17308307318289,-4.425,81.2675570700389));
#63329=CARTESIAN_POINT('',(6.64444623802422,-2.20555376197578,82.8429303939101));
#63330=CARTESIAN_POINT('',(3.,-4.5,83.9581591295319));
#63331=CARTESIAN_POINT('Origin',(3.075,-4.425,71.4583915927537));
#63332=CARTESIAN_POINT('Origin',(4.425,-4.425,59.4601776313845));
#63333=CARTESIAN_POINT('Origin',(-3.87017654832143,-4.425,79.4928504366996));
#63334=CARTESIAN_POINT('',(6.42476289193132,-2.42523710806868,81.1117987367094));
#63335=CARTESIAN_POINT('',(3.,-4.5,82.073203537378));
#63336=CARTESIAN_POINT('Origin',(3.075,-4.425,70.5159137966767));
#63337=CARTESIAN_POINT('',(3.,-4.5,81.4666188312375));
#63338=CARTESIAN_POINT('Origin',(4.00003360329214,-4.425,81.1824496993089));
#63339=CARTESIAN_POINT('',(1.32928584952567,-7.52071415047433,78.8601321960397));
#63340=CARTESIAN_POINT('Origin',(4.425,-4.425,59.4601776313845));
#63341=CARTESIAN_POINT('Origin',(-3.56727002345996,-4.425,77.7181438033603));
#63342=CARTESIAN_POINT('',(6.20507954583794,-2.64492045416205,79.3806670795092));
#63343=CARTESIAN_POINT('',(3.,-4.5,80.1882479452242));
#63344=CARTESIAN_POINT('Origin',(3.075,-4.425,69.5734360005998));
#63345=CARTESIAN_POINT('',(3.,-4.5,79.5816632390836));
#63346=CARTESIAN_POINT('Origin',(3.69712707843067,-4.425,79.4077430659696));
#63347=CARTESIAN_POINT('',(1.54896919561877,-7.30103080438123,77.129000538839));
#63348=CARTESIAN_POINT('Origin',(4.425,-4.425,59.4601776313845));
#63349=CARTESIAN_POINT('Origin',(3.075,-4.425,68.6309582045228));
#63350=CARTESIAN_POINT('',(3.,-4.5,77.6967076469297));
#63351=CARTESIAN_POINT('Origin',(3.39422055356921,-4.425,77.6330364326303));
#63352=CARTESIAN_POINT('',(1.76865254171217,-7.08134745828783,75.3978688816388));
#63353=CARTESIAN_POINT('Origin',(4.425,-4.425,59.4601776313845));
#63354=CARTESIAN_POINT('',(4.5,-4.35,59.4601776313845));
#63355=CARTESIAN_POINT('Origin',(-2.96145697373703,-4.425,74.1687305366817));
#63356=CARTESIAN_POINT('',(5.7657128536508,-3.0842871463492,75.9184037651093));
#63357=CARTESIAN_POINT('',(3.39181079723248,-4.10818920276752,76.1439878871423));
#63358=CARTESIAN_POINT('Origin',(3.075,-4.425,67.6884804084459));
#63359=CARTESIAN_POINT('',(3.,-4.5,75.8117520547759));
#63360=CARTESIAN_POINT('Origin',(3.09131402870775,-4.425,75.858329799291));
#63361=CARTESIAN_POINT('Origin',(3.075,-4.425,66.746002612369));
#63362=CARTESIAN_POINT('',(3.,-4.5,73.926796462622));
#63363=CARTESIAN_POINT('Origin',(2.78840750384627,-4.425,74.0836231659517));
#63364=CARTESIAN_POINT('',(2.20801923389894,-6.64198076610106,71.9356055672385));
#63365=CARTESIAN_POINT('Origin',(-2.3556439240141,-4.425,70.6193172700032));
#63366=CARTESIAN_POINT('',(5.32634616146465,-3.52365383853535,72.4561404507083));
#63367=CARTESIAN_POINT('',(3.,-4.5,72.6484255766087));
#63368=CARTESIAN_POINT('Origin',(3.075,-4.425,65.803524816292));
#63369=CARTESIAN_POINT('',(3.,-4.5,72.0418408704681));
#63370=CARTESIAN_POINT('Origin',(2.48550097898481,-4.425,72.3089165326124));
#63371=CARTESIAN_POINT('',(2.42770257999234,-6.42229742000766,70.2044739100384));
#63372=CARTESIAN_POINT('Origin',(4.425,-4.425,59.4601776313845));
#63373=CARTESIAN_POINT('Origin',(-2.05273739915263,-4.425,68.8446106366639));
#63374=CARTESIAN_POINT('',(5.10666281537071,-3.74333718462929,70.7250087935087));
#63375=CARTESIAN_POINT('',(3.,-4.5,70.7634699844547));
#63376=CARTESIAN_POINT('Origin',(3.075,-4.425,64.8610470202151));
#63377=CARTESIAN_POINT('Origin',(4.425,-4.425,59.4601776313845));
#63378=CARTESIAN_POINT('Origin',(-3.375,-4.44696699141101,59.7821446227955));
#63379=CARTESIAN_POINT('',(4.43786796564403,-4.41213203435596,59.6980455970285));
#63380=CARTESIAN_POINT('',(2.41498854218627,-3.57422794211429,57.6751661735708));
#63381=CARTESIAN_POINT('',(3.95870352594775,-4.89129647405225,60.8548508859502));
#63382=CARTESIAN_POINT('Origin',(-11.4428396698581,-4.425,123.860516270182));
#63383=CARTESIAN_POINT('',(11.9168465442685,3.06684654426849,124.39009016671));
#63384=CARTESIAN_POINT('',(3.,-4.5,129.197093341225));
#63385=CARTESIAN_POINT('Origin',(3.075,-4.425,94.0778586986002));
#63386=CARTESIAN_POINT('',(2.99999999999999,-4.5,128.590508635084));
#63387=CARTESIAN_POINT('Origin',(11.5726967248288,-4.425,125.550115532791));
#63388=CARTESIAN_POINT('',(-4.16279780280838,-13.0127978028084,122.138423626045));
#63389=CARTESIAN_POINT('Origin',(4.425,-4.425,59.4601776313845));
#63390=CARTESIAN_POINT('Origin',(-11.1399331449968,-4.425,122.085809636842));
#63391=CARTESIAN_POINT('',(11.6971631981738,2.84716319817385,122.658958509512));
#63392=CARTESIAN_POINT('',(3.,-4.5,127.312137749071));
#63393=CARTESIAN_POINT('Origin',(3.075,-4.425,93.1353809025232));
#63394=CARTESIAN_POINT('',(3.,-4.5,126.705553042931));
#63395=CARTESIAN_POINT('Origin',(11.2697901999676,-4.425,123.775408899452));
#63396=CARTESIAN_POINT('Origin',(4.425,-4.425,59.4601776313845));
#63397=CARTESIAN_POINT('Ctrl Pts',(-0.935227410421504,-1.48505040008624,
61.4601776313845));
#63398=CARTESIAN_POINT('Ctrl Pts',(-0.935227410421504,-1.48505040008624,
61.3891441263593));
#63399=CARTESIAN_POINT('Ctrl Pts',(-0.919615649085625,-1.49487746321015,
61.2422731598338));
#63400=CARTESIAN_POINT('Ctrl Pts',(-0.849468438578091,-1.53686812251223,
61.0333879936081));
#63401=CARTESIAN_POINT('Ctrl Pts',(-0.735914858055534,-1.59497632661104,
60.8514498111743));
#63402=CARTESIAN_POINT('Ctrl Pts',(-0.598310313784555,-1.65242100436025,
60.7107010115764));
#63403=CARTESIAN_POINT('Ctrl Pts',(-0.448703130287871,-1.69877028516103,
60.6130238318804));
#63404=CARTESIAN_POINT('Ctrl Pts',(-0.33264122576857,-1.72358803958856,
60.564437741829));
#63405=CARTESIAN_POINT('Ctrl Pts',(-0.272364982794092,-1.73372376318135,
60.5450033341972));
#63406=CARTESIAN_POINT('Ctrl Pts',(-0.237531681197459,-1.73876819237024,
60.5354423077009));
#63407=CARTESIAN_POINT('Ctrl Pts',(-0.0789701298399566,-1.75925740461135,
60.4969143456161));
#63408=CARTESIAN_POINT('Ctrl Pts',(0.0760194607809564,-1.75928712608876,
60.4968764455387));
#63409=CARTESIAN_POINT('Ctrl Pts',(0.228735482046854,-1.73994680766547,
60.5332249124204));
#63410=CARTESIAN_POINT('Ctrl Pts',(0.252049875042143,-1.73674755611036,
60.5392730095349));
#63411=CARTESIAN_POINT('Ctrl Pts',(0.292578207370474,-1.73057269707577,
60.5510083786442));
#63412=CARTESIAN_POINT('Ctrl Pts',(0.372075688502887,-1.71598007394311,
60.5791940588586));
#63413=CARTESIAN_POINT('Ctrl Pts',(0.479224028492418,-1.6897225475368,60.6316466004299));
#63414=CARTESIAN_POINT('Ctrl Pts',(0.594393972224216,-1.6522873143202,60.7127508682801));
#63415=CARTESIAN_POINT('Ctrl Pts',(0.722593849137971,-1.60147251676923,
60.834783417798));
#63416=CARTESIAN_POINT('Ctrl Pts',(0.814959219695543,-1.55505030204574,
60.9708247013374));
#63417=CARTESIAN_POINT('Ctrl Pts',(0.871291361756753,-1.52340370940006,
61.10429390882));
#63418=CARTESIAN_POINT('Ctrl Pts',(0.902393644067836,-1.50528176938052,
61.196100120568));
#63419=CARTESIAN_POINT('Ctrl Pts',(0.938735066575289,-1.48284224282614,
61.3654968018582));
#63420=CARTESIAN_POINT('Ctrl Pts',(0.938582534367773,-1.48290872908077,
61.5313282028974));
#63421=CARTESIAN_POINT('Ctrl Pts',(0.904175169636998,-1.50419692024269,
61.7242600329632));
#63422=CARTESIAN_POINT('Ctrl Pts',(0.85721285894179,-1.53213405783326,61.8633698692225));
#63423=CARTESIAN_POINT('Ctrl Pts',(0.775381471169404,-1.57514340099823,
62.0083583724577));
#63424=CARTESIAN_POINT('Ctrl Pts',(0.690738387260799,-1.61425222701105,
62.1162128434089));
#63425=CARTESIAN_POINT('Ctrl Pts',(0.59471425097924,-1.6523256721306,62.2076820178571));
#63426=CARTESIAN_POINT('Ctrl Pts',(0.441520175140093,-1.70219588091644,
62.3156185449291));
#63427=CARTESIAN_POINT('Ctrl Pts',(0.260489914084767,-1.74025400897717,
62.3877929030015));
#63428=CARTESIAN_POINT('Ctrl Pts',(0.0692954676913469,-1.75545738735951,
62.4159688547089));
#63429=CARTESIAN_POINT('Ctrl Pts',(-0.116362742719129,-1.75565543297752,
62.4160667144284));
#63430=CARTESIAN_POINT('Ctrl Pts',(-0.356773244315879,-1.72599810988677,
62.3624101762215));
#63431=CARTESIAN_POINT('Ctrl Pts',(-0.583275116725225,-1.65894838175102,
62.2258716165825));
#63432=CARTESIAN_POINT('Ctrl Pts',(-0.736417081706063,-1.59492671578796,
62.0687636727456));
#63433=CARTESIAN_POINT('Ctrl Pts',(-0.849635873494022,-1.53689456816766,
61.8870852321429));
#63434=CARTESIAN_POINT('Ctrl Pts',(-0.919766275354451,-1.49486469045067,
61.6780476559334));
#63435=CARTESIAN_POINT('Ctrl Pts',(-0.935227410421504,-1.48505040008624,
61.5312111364096));
#63436=CARTESIAN_POINT('Ctrl Pts',(-0.935227410421504,-1.48505040008624,
61.4601776313845));
#63437=CARTESIAN_POINT('Ctrl Pts',(-0.891818273614336,-1.55986263178064,
61.4601776313845));
#63438=CARTESIAN_POINT('Ctrl Pts',(-0.891818273614336,-1.55986263178064,
61.3951284615141));
#63439=CARTESIAN_POINT('Ctrl Pts',(-0.877744688906537,-1.56849750781793,
61.2606215699825));
#63440=CARTESIAN_POINT('Ctrl Pts',(-0.813799731091216,-1.60578900068647,
61.0666402243125));
#63441=CARTESIAN_POINT('Ctrl Pts',(-0.70816041514642,-1.65818502178782,
60.8940616379229));
#63442=CARTESIAN_POINT('Ctrl Pts',(-0.578021741472897,-1.71056879712429,
60.7580300263371));
#63443=CARTESIAN_POINT('Ctrl Pts',(-0.434686640643755,-1.75314130539658,
60.6621866866951));
#63444=CARTESIAN_POINT('Ctrl Pts',(-0.32265618707681,-1.77601059240704,
60.6141022029886));
#63445=CARTESIAN_POINT('Ctrl Pts',(-0.264331980636356,-1.78535838340448,
60.5948182695924));
#63446=CARTESIAN_POINT('Ctrl Pts',(-0.230589683070617,-1.79001281129946,
60.585317478617));
#63447=CARTESIAN_POINT('Ctrl Pts',(-0.0768991900276076,-1.8089236687873,
60.5469930291481));
#63448=CARTESIAN_POINT('Ctrl Pts',(0.0740287221081122,-1.80895102721411,
60.5469534448937));
#63449=CARTESIAN_POINT('Ctrl Pts',(0.222067318628145,-1.79110012631182,
60.5831123928036));
#63450=CARTESIAN_POINT('Ctrl Pts',(0.244658308810622,-1.78814794047804,
60.5891243889555));
#63451=CARTESIAN_POINT('Ctrl Pts',(0.283904295083939,-1.78245099890452,
60.6007819234622));
#63452=CARTESIAN_POINT('Ctrl Pts',(0.360767972306015,-1.76899704119178,
60.6287231584559));
#63453=CARTESIAN_POINT('Ctrl Pts',(0.463978823988154,-1.7448203980967,60.6805097909023));
#63454=CARTESIAN_POINT('Ctrl Pts',(0.574112430572595,-1.71048215605517,
60.7598502334435));
#63455=CARTESIAN_POINT('Ctrl Pts',(0.695680975640035,-1.66408640779924,
60.8780352498123));
#63456=CARTESIAN_POINT('Ctrl Pts',(0.781805858564989,-1.6221390249812,61.0075932553954));
#63457=CARTESIAN_POINT('Ctrl Pts',(0.833613079412961,-1.59385921572437,
61.1323587545323));
#63458=CARTESIAN_POINT('Ctrl Pts',(0.862072495872827,-1.57772634548218,
61.2176672311318));
#63459=CARTESIAN_POINT('Ctrl Pts',(0.895009775933105,-1.55789844255671,
61.373753949522));
#63460=CARTESIAN_POINT('Ctrl Pts',(0.894856619732835,-1.55796819614332,
61.5251376909164));
#63461=CARTESIAN_POINT('Ctrl Pts',(0.863683914665523,-1.57677134969902,
61.7026244669316));
#63462=CARTESIAN_POINT('Ctrl Pts',(0.820835411334987,-1.60159600839885,
61.8318004513303));
#63463=CARTESIAN_POINT('Ctrl Pts',(0.744933623620128,-1.64028625542469,
61.9687681386248));
#63464=CARTESIAN_POINT('Ctrl Pts',(0.665475763530155,-1.67576108720713,
62.0719971623455));
#63465=CARTESIAN_POINT('Ctrl Pts',(0.57442728941605,-1.7105169688379,62.160574523964));
#63466=CARTESIAN_POINT('Ctrl Pts',(0.427934605144566,-1.75626706312665,
62.266178371631));
#63467=CARTESIAN_POINT('Ctrl Pts',(0.25300223677069,-1.79138357718446,62.3378865426985));
#63468=CARTESIAN_POINT('Ctrl Pts',(0.0673494918380112,-1.80542289158326,
62.365969662501));
#63469=CARTESIAN_POINT('Ctrl Pts',(-0.113085827426488,-1.80561147465042,
62.3661013522531));
#63470=CARTESIAN_POINT('Ctrl Pts',(-0.346407983829098,-1.77819658625783,
62.312460591346));
#63471=CARTESIAN_POINT('Ctrl Pts',(-0.563841388541595,-1.7165160210848,
62.1779743621097));
#63472=CARTESIAN_POINT('Ctrl Pts',(-0.708642961553554,-1.6581402336975,
62.0261579496237));
#63473=CARTESIAN_POINT('Ctrl Pts',(-0.813969536493406,-1.60581191306522,
61.8538230221461));
#63474=CARTESIAN_POINT('Ctrl Pts',(-0.877889851198672,-1.56848592986011,
61.6597004901767));
#63475=CARTESIAN_POINT('Ctrl Pts',(-0.891818273614336,-1.55986263178064,
61.5252268012549));
#63476=CARTESIAN_POINT('Ctrl Pts',(-0.891818273614336,-1.55986263178064,
61.4601776313845));
#63477=CARTESIAN_POINT('Ctrl Pts',(-0.848409136807168,-1.63467486347503,
61.4601776313845));
#63478=CARTESIAN_POINT('Ctrl Pts',(-0.848409136807168,-1.63467486347503,
61.4011127966688));
#63479=CARTESIAN_POINT('Ctrl Pts',(-0.835873728727449,-1.6421175524257,
61.2789699801313));
#63480=CARTESIAN_POINT('Ctrl Pts',(-0.778131023604341,-1.67470987886071,
61.0998924550167));
#63481=CARTESIAN_POINT('Ctrl Pts',(-0.680405972237307,-1.72139371696459,
60.9366734646713));
#63482=CARTESIAN_POINT('Ctrl Pts',(-0.55773316916124,-1.76871658988833,
60.8053590410978));
#63483=CARTESIAN_POINT('Ctrl Pts',(-0.420670150999641,-1.80751232563214,
60.7113495415097));
#63484=CARTESIAN_POINT('Ctrl Pts',(-0.312671148385052,-1.82843314522552,
60.6637666641482));
#63485=CARTESIAN_POINT('Ctrl Pts',(-0.256298978478621,-1.83699300362762,
60.6446332049876));
#63486=CARTESIAN_POINT('Ctrl Pts',(-0.223647684943777,-1.84125743022868,
60.635192649533));
#63487=CARTESIAN_POINT('Ctrl Pts',(-0.0748282502152587,-1.85858993296325,
60.5970717126801));
#63488=CARTESIAN_POINT('Ctrl Pts',(0.0720379834352672,-1.85861492833947,
60.5970304442487));
#63489=CARTESIAN_POINT('Ctrl Pts',(0.215399155209435,-1.84225344495817,
60.6329998731868));
#63490=CARTESIAN_POINT('Ctrl Pts',(0.237266742579102,-1.83954832484572,
60.6389757683761));
#63491=CARTESIAN_POINT('Ctrl Pts',(0.275230382797404,-1.83432930073327,
60.6505554682802));
#63492=CARTESIAN_POINT('Ctrl Pts',(0.349460256109143,-1.82201400844044,
60.6782522580532));
#63493=CARTESIAN_POINT('Ctrl Pts',(0.448733619483891,-1.7999182486566,60.7293729813747));
#63494=CARTESIAN_POINT('Ctrl Pts',(0.553830888920974,-1.76867699779014,
60.8069495986068));
#63495=CARTESIAN_POINT('Ctrl Pts',(0.6687681021421,-1.72670029882925,60.9212870818265));
#63496=CARTESIAN_POINT('Ctrl Pts',(0.748652497434435,-1.68922774791666,
61.0443618094534));
#63497=CARTESIAN_POINT('Ctrl Pts',(0.795934797069171,-1.66431472204868,
61.1604236002446));
#63498=CARTESIAN_POINT('Ctrl Pts',(0.821751347677819,-1.65017092158383,
61.2392343416956));
#63499=CARTESIAN_POINT('Ctrl Pts',(0.851284485290922,-1.63295464228727,
61.3820110971857));
#63500=CARTESIAN_POINT('Ctrl Pts',(0.851130705097898,-1.63302766320586,
61.5189471789355));
#63501=CARTESIAN_POINT('Ctrl Pts',(0.823192659694048,-1.64934577915535,
61.6809889009));
#63502=CARTESIAN_POINT('Ctrl Pts',(0.784457963728185,-1.67105795896445,
61.8002310334381));
#63503=CARTESIAN_POINT('Ctrl Pts',(0.714485776070854,-1.70542910985115,
61.9291779047919));
#63504=CARTESIAN_POINT('Ctrl Pts',(0.640213139799511,-1.73726994740321,
62.0277814812822));
#63505=CARTESIAN_POINT('Ctrl Pts',(0.554140327852861,-1.76870826554519,
62.113467030071));
#63506=CARTESIAN_POINT('Ctrl Pts',(0.414349035149039,-1.81033824533686,
62.216738198333));
#63507=CARTESIAN_POINT('Ctrl Pts',(0.245514559456612,-1.84251314539175,
62.2879801823955));
#63508=CARTESIAN_POINT('Ctrl Pts',(0.0654035159846756,-1.855388395807,62.3159704702932));
#63509=CARTESIAN_POINT('Ctrl Pts',(-0.109808912133848,-1.85556751632333,
62.3161359900777));
#63510=CARTESIAN_POINT('Ctrl Pts',(-0.336042723342318,-1.8303950626289,
62.2625110064705));
#63511=CARTESIAN_POINT('Ctrl Pts',(-0.544407660357965,-1.77408366041858,
62.130077107637));
#63512=CARTESIAN_POINT('Ctrl Pts',(-0.680868841401045,-1.72135375160704,
61.9835522265018));
#63513=CARTESIAN_POINT('Ctrl Pts',(-0.778303199492791,-1.67472925796279,
61.8205608121493));
#63514=CARTESIAN_POINT('Ctrl Pts',(-0.836013427042894,-1.64210716926955,
61.6413533244201));
#63515=CARTESIAN_POINT('Ctrl Pts',(-0.848409136807168,-1.63467486347503,
61.5192424661002));
#63516=CARTESIAN_POINT('Ctrl Pts',(-0.848409136807168,-1.63467486347503,
61.4601776313845));
#63517=CARTESIAN_POINT('Ctrl Pts',(-0.805,-1.70948709516943,61.4601776313845));
#63518=CARTESIAN_POINT('Ctrl Pts',(-0.805,-1.70948709516943,61.4070971318236));
#63519=CARTESIAN_POINT('Ctrl Pts',(-0.794002768548361,-1.71573759703348,
61.29731839028));
#63520=CARTESIAN_POINT('Ctrl Pts',(-0.742462316117465,-1.74363075703495,
61.133144685721));
#63521=CARTESIAN_POINT('Ctrl Pts',(-0.652651529328193,-1.78460241214137,
60.9792852914198));
#63522=CARTESIAN_POINT('Ctrl Pts',(-0.537444596849582,-1.82686438265237,
60.8526880558586));
#63523=CARTESIAN_POINT('Ctrl Pts',(-0.406653661355526,-1.8618833458677,
60.7605123963243));
#63524=CARTESIAN_POINT('Ctrl Pts',(-0.302686109693293,-1.880855698044,60.7134311253077));
#63525=CARTESIAN_POINT('Ctrl Pts',(-0.248265976320886,-1.88862762385075,
60.6944481403828));
#63526=CARTESIAN_POINT('Ctrl Pts',(-0.216705686816935,-1.8925020491579,
60.685067820449));
#63527=CARTESIAN_POINT('Ctrl Pts',(-0.0727573104029104,-1.9082561971392,
60.6471503962121));
#63528=CARTESIAN_POINT('Ctrl Pts',(0.0700472447624226,-1.90827882946482,
60.6471074436038));
#63529=CARTESIAN_POINT('Ctrl Pts',(0.208730991790726,-1.89340676360453,
60.68288735357));
#63530=CARTESIAN_POINT('Ctrl Pts',(0.229875176347581,-1.8909487092134,60.6888271477967));
#63531=CARTESIAN_POINT('Ctrl Pts',(0.266556470510869,-1.88620760256202,
60.7003290130983));
#63532=CARTESIAN_POINT('Ctrl Pts',(0.33815253991227,-1.8750309756891,60.7277813576505));
#63533=CARTESIAN_POINT('Ctrl Pts',(0.433488414979626,-1.8550160992165,60.7782361718472));
#63534=CARTESIAN_POINT('Ctrl Pts',(0.533549347269353,-1.82687183952511,
60.8540489637702));
#63535=CARTESIAN_POINT('Ctrl Pts',(0.641855228644165,-1.78931418985927,
60.9645389138408));
#63536=CARTESIAN_POINT('Ctrl Pts',(0.715499136303881,-1.75631647085212,
61.0811303635114));
#63537=CARTESIAN_POINT('Ctrl Pts',(0.75825651472538,-1.73477022837298,61.1884884459569));
#63538=CARTESIAN_POINT('Ctrl Pts',(0.781430199482811,-1.72261549768548,
61.2608014522594));
#63539=CARTESIAN_POINT('Ctrl Pts',(0.807559194648739,-1.70801084201783,
61.3902682448495));
#63540=CARTESIAN_POINT('Ctrl Pts',(0.80740479046296,-1.70808713026841,61.5127566669546));
#63541=CARTESIAN_POINT('Ctrl Pts',(0.782701404722573,-1.72192020861167,
61.6593533348685));
#63542=CARTESIAN_POINT('Ctrl Pts',(0.748080516121382,-1.74051990953005,
61.7686616155459));
#63543=CARTESIAN_POINT('Ctrl Pts',(0.684037928521579,-1.7705719642776,61.889587670959));
#63544=CARTESIAN_POINT('Ctrl Pts',(0.614950516068867,-1.79877880759929,
61.9835658002188));
#63545=CARTESIAN_POINT('Ctrl Pts',(0.533853366289671,-1.82689956225249,
62.0663595361779));
#63546=CARTESIAN_POINT('Ctrl Pts',(0.400763465153512,-1.86440942754707,
62.1672980250349));
#63547=CARTESIAN_POINT('Ctrl Pts',(0.238026882142535,-1.89364271359903,
62.2380738220926));
#63548=CARTESIAN_POINT('Ctrl Pts',(0.0634575401313399,-1.90535390003075,
62.2659712780854));
#63549=CARTESIAN_POINT('Ctrl Pts',(-0.106531996841207,-1.90552355799623,
62.2661706279024));
#63550=CARTESIAN_POINT('Ctrl Pts',(-0.325677462855537,-1.88259353899996,
62.2125614215949));
#63551=CARTESIAN_POINT('Ctrl Pts',(-0.524973932174335,-1.83165129975237,
62.0821798531642));
#63552=CARTESIAN_POINT('Ctrl Pts',(-0.653094721248536,-1.78456726951658,
61.9409465033799));
#63553=CARTESIAN_POINT('Ctrl Pts',(-0.742636862492175,-1.74364660286035,
61.7872986021525));
#63554=CARTESIAN_POINT('Ctrl Pts',(-0.794137002887115,-1.71572840867899,
61.6230061586634));
#63555=CARTESIAN_POINT('Ctrl Pts',(-0.805,-1.70948709516943,61.5132581309454));
#63556=CARTESIAN_POINT('Ctrl Pts',(-0.805,-1.70948709516943,61.4601776313845));
#63557=CARTESIAN_POINT('',(-0.935227410421504,-1.48505040008624,61.4601776313845));
#63558=CARTESIAN_POINT('',(-0.805,-1.70948709516943,61.4601776313845));
#63559=CARTESIAN_POINT('',(-0.935227410421504,-1.48505040008624,61.4601776313845));
#63560=CARTESIAN_POINT('',(-3.66463531352099E-6,-1.90497281869116,60.6550571401644));
#63561=CARTESIAN_POINT('Ctrl Pts',(-0.805,-1.70948709516943,61.4601776313845));
#63562=CARTESIAN_POINT('Ctrl Pts',(-0.805,-1.70948709516943,61.4070971318236));
#63563=CARTESIAN_POINT('Ctrl Pts',(-0.794002768548361,-1.71573759703348,
61.29731839028));
#63564=CARTESIAN_POINT('Ctrl Pts',(-0.742462316117465,-1.74363075703495,
61.133144685721));
#63565=CARTESIAN_POINT('Ctrl Pts',(-0.652651529328193,-1.78460241214137,
60.9792852914198));
#63566=CARTESIAN_POINT('Ctrl Pts',(-0.537444596849582,-1.82686438265237,
60.8526880558586));
#63567=CARTESIAN_POINT('Ctrl Pts',(-0.406653661355526,-1.8618833458677,
60.7605123963243));
#63568=CARTESIAN_POINT('Ctrl Pts',(-0.302686109693293,-1.880855698044,60.7134311253077));
#63569=CARTESIAN_POINT('Ctrl Pts',(-0.248265976320886,-1.88862762385075,
60.6944481403828));
#63570=CARTESIAN_POINT('Ctrl Pts',(-0.216705686816935,-1.8925020491579,
60.685067820449));
#63571=CARTESIAN_POINT('Ctrl Pts',(-0.136734366586922,-1.90125435359195,
60.6640025847618));
#63572=CARTESIAN_POINT('Ctrl Pts',(-0.0643497242950811,-1.90496731588625,
60.6550692535498));
#63573=CARTESIAN_POINT('Ctrl Pts',(-3.66463531351058E-6,-1.90497281869116,
60.6550571401644));
#63574=CARTESIAN_POINT('Ctrl Pts',(-3.66463531351058E-6,-1.90497281869116,
60.6550571401644));
#63575=CARTESIAN_POINT('Ctrl Pts',(0.0643423950244553,-1.90497832149607,
60.655045026779));
#63576=CARTESIAN_POINT('Ctrl Pts',(0.134055128006254,-1.90141479906776,
60.6636212482036));
#63577=CARTESIAN_POINT('Ctrl Pts',(0.208730991790726,-1.89340676360453,
60.68288735357));
#63578=CARTESIAN_POINT('Ctrl Pts',(0.229875176347581,-1.8909487092134,60.6888271477967));
#63579=CARTESIAN_POINT('Ctrl Pts',(0.266556470510869,-1.88620760256202,
60.7003290130983));
#63580=CARTESIAN_POINT('Ctrl Pts',(0.33815253991227,-1.8750309756891,60.7277813576505));
#63581=CARTESIAN_POINT('Ctrl Pts',(0.433488414979626,-1.8550160992165,60.7782361718472));
#63582=CARTESIAN_POINT('Ctrl Pts',(0.533549347269353,-1.82687183952511,
60.8540489637702));
#63583=CARTESIAN_POINT('Ctrl Pts',(0.641855228644165,-1.78931418985927,
60.9645389138408));
#63584=CARTESIAN_POINT('Ctrl Pts',(0.715499136303881,-1.75631647085212,
61.0811303635114));
#63585=CARTESIAN_POINT('Ctrl Pts',(0.75825651472538,-1.73477022837298,61.1884884459569));
#63586=CARTESIAN_POINT('Ctrl Pts',(0.781430199482811,-1.72261549768548,
61.2608014522594));
#63587=CARTESIAN_POINT('Ctrl Pts',(0.807559194648739,-1.70801084201783,
61.3902682448495));
#63588=CARTESIAN_POINT('Ctrl Pts',(0.80740479046296,-1.70808713026841,61.5127566669546));
#63589=CARTESIAN_POINT('Ctrl Pts',(0.782701404722573,-1.72192020861167,
61.6593533348685));
#63590=CARTESIAN_POINT('Ctrl Pts',(0.748080516121382,-1.74051990953005,
61.7686616155459));
#63591=CARTESIAN_POINT('Ctrl Pts',(0.684037928521579,-1.7705719642776,61.889587670959));
#63592=CARTESIAN_POINT('Ctrl Pts',(0.614950516068867,-1.79877880759929,
61.9835658002188));
#63593=CARTESIAN_POINT('Ctrl Pts',(0.533853366289671,-1.82689956225249,
62.0663595361779));
#63594=CARTESIAN_POINT('Ctrl Pts',(0.400763465153512,-1.86440942754707,
62.1672980250349));
#63595=CARTESIAN_POINT('Ctrl Pts',(0.238026882142535,-1.89364271359903,
62.2380738220926));
#63596=CARTESIAN_POINT('Ctrl Pts',(0.0634575401313399,-1.90535390003075,
62.2659712780854));
#63597=CARTESIAN_POINT('Ctrl Pts',(-0.106531996841207,-1.90552355799623,
62.2661706279024));
#63598=CARTESIAN_POINT('Ctrl Pts',(-0.325677462855537,-1.88259353899996,
62.2125614215949));
#63599=CARTESIAN_POINT('Ctrl Pts',(-0.524973932174335,-1.83165129975237,
62.0821798531642));
#63600=CARTESIAN_POINT('Ctrl Pts',(-0.653094721248536,-1.78456726951658,
61.9409465033799));
#63601=CARTESIAN_POINT('Ctrl Pts',(-0.742636862492175,-1.74364660286035,
61.7872986021525));
#63602=CARTESIAN_POINT('Ctrl Pts',(-0.794137002887115,-1.71572840867899,
61.6230061586634));
#63603=CARTESIAN_POINT('Ctrl Pts',(-0.805,-1.70948709516943,61.5132581309454));
#63604=CARTESIAN_POINT('Ctrl Pts',(-0.805,-1.70948709516943,61.4601776313845));
#63605=CARTESIAN_POINT('Ctrl Pts',(-0.935227410421504,-1.48505040008624,
61.4601776313845));
#63606=CARTESIAN_POINT('Ctrl Pts',(-0.935227410421504,-1.48505040008624,
61.5312111364096));
#63607=CARTESIAN_POINT('Ctrl Pts',(-0.919766275354451,-1.49486469045067,
61.6780476559334));
#63608=CARTESIAN_POINT('Ctrl Pts',(-0.849635873494022,-1.53689456816766,
61.8870852321429));
#63609=CARTESIAN_POINT('Ctrl Pts',(-0.736417081706063,-1.59492671578796,
62.0687636727456));
#63610=CARTESIAN_POINT('Ctrl Pts',(-0.583275116725225,-1.65894838175102,
62.2258716165825));
#63611=CARTESIAN_POINT('Ctrl Pts',(-0.356773244315879,-1.72599810988677,
62.3624101762215));
#63612=CARTESIAN_POINT('Ctrl Pts',(-0.116362742719129,-1.75565543297752,
62.4160667144284));
#63613=CARTESIAN_POINT('Ctrl Pts',(0.0692954676913469,-1.75545738735951,
62.4159688547089));
#63614=CARTESIAN_POINT('Ctrl Pts',(0.260489914084767,-1.74025400897717,
62.3877929030015));
#63615=CARTESIAN_POINT('Ctrl Pts',(0.441520175140093,-1.70219588091644,
62.3156185449291));
#63616=CARTESIAN_POINT('Ctrl Pts',(0.59471425097924,-1.6523256721306,62.2076820178571));
#63617=CARTESIAN_POINT('Ctrl Pts',(0.690738387260799,-1.61425222701105,
62.1162128434089));
#63618=CARTESIAN_POINT('Ctrl Pts',(0.775381471169404,-1.57514340099823,
62.0083583724577));
#63619=CARTESIAN_POINT('Ctrl Pts',(0.85721285894179,-1.53213405783326,61.8633698692225));
#63620=CARTESIAN_POINT('Ctrl Pts',(0.904175169636998,-1.50419692024269,
61.7242600329632));
#63621=CARTESIAN_POINT('Ctrl Pts',(0.938582534367773,-1.48290872908077,
61.5313282028974));
#63622=CARTESIAN_POINT('Ctrl Pts',(0.938735066575289,-1.48284224282614,
61.3654968018582));
#63623=CARTESIAN_POINT('Ctrl Pts',(0.902393644067836,-1.50528176938052,
61.196100120568));
#63624=CARTESIAN_POINT('Ctrl Pts',(0.871291361756753,-1.52340370940006,
61.10429390882));
#63625=CARTESIAN_POINT('Ctrl Pts',(0.814959219695543,-1.55505030204574,
60.9708247013374));
#63626=CARTESIAN_POINT('Ctrl Pts',(0.722593849137971,-1.60147251676923,
60.834783417798));
#63627=CARTESIAN_POINT('Ctrl Pts',(0.594393972224216,-1.6522873143202,60.7127508682801));
#63628=CARTESIAN_POINT('Ctrl Pts',(0.479224028492418,-1.6897225475368,60.6316466004299));
#63629=CARTESIAN_POINT('Ctrl Pts',(0.372075688502887,-1.71598007394311,
60.5791940588586));
#63630=CARTESIAN_POINT('Ctrl Pts',(0.292578207370474,-1.73057269707577,
60.5510083786442));
#63631=CARTESIAN_POINT('Ctrl Pts',(0.252049875042143,-1.73674755611036,
60.5392730095349));
#63632=CARTESIAN_POINT('Ctrl Pts',(0.228735482046854,-1.73994680766547,
60.5332249124204));
#63633=CARTESIAN_POINT('Ctrl Pts',(0.0760194607809564,-1.75928712608876,
60.4968764455387));
#63634=CARTESIAN_POINT('Ctrl Pts',(-0.0789701298399566,-1.75925740461135,
60.4969143456161));
#63635=CARTESIAN_POINT('Ctrl Pts',(-0.237531681197459,-1.73876819237024,
60.5354423077009));
#63636=CARTESIAN_POINT('Ctrl Pts',(-0.272364982794092,-1.73372376318135,
60.5450033341972));
#63637=CARTESIAN_POINT('Ctrl Pts',(-0.33264122576857,-1.72358803958856,
60.564437741829));
#63638=CARTESIAN_POINT('Ctrl Pts',(-0.448703130287871,-1.69877028516103,
60.6130238318804));
#63639=CARTESIAN_POINT('Ctrl Pts',(-0.598310313784555,-1.65242100436025,
60.7107010115764));
#63640=CARTESIAN_POINT('Ctrl Pts',(-0.735914858055534,-1.59497632661104,
60.8514498111743));
#63641=CARTESIAN_POINT('Ctrl Pts',(-0.849468438578091,-1.53686812251223,
61.0333879936081));
#63642=CARTESIAN_POINT('Ctrl Pts',(-0.919615649085625,-1.49487746321015,
61.2422731598338));
#63643=CARTESIAN_POINT('Ctrl Pts',(-0.935227410421504,-1.48505040008624,
61.3891441263593));
#63644=CARTESIAN_POINT('Ctrl Pts',(-0.935227410421504,-1.48505040008624,
61.4601776313845));
#63645=CARTESIAN_POINT('Origin',(0.,-2.865,61.4601776313845));
#63646=CARTESIAN_POINT('',(-9.85840673313619E-17,-4.4,60.6551776313845));
#63647=CARTESIAN_POINT('Origin',(0.,-4.4,61.4601776313845));
#63648=CARTESIAN_POINT('',(-9.85840673313619E-17,-2.865,60.6551776313845));
#63649=CARTESIAN_POINT('Origin',(0.,0.,64.4451776313845));
#63650=CARTESIAN_POINT('',(-1.755,-2.1492551325036E-16,59.6101776313845));
#63651=CARTESIAN_POINT('Origin',(0.,0.,59.6101776313845));
#63652=CARTESIAN_POINT('',(-1.755,-2.1492551325036E-16,69.4601776313845));
#63653=CARTESIAN_POINT('',(-1.755,-2.1492551325036E-16,64.4451776313845));
#63654=CARTESIAN_POINT('Origin',(0.,0.,69.4601776313845));
#63655=CARTESIAN_POINT('Origin',(0.,-4.45,61.4601776313845));
#63656=CARTESIAN_POINT('',(1.04707301327099E-16,-4.45,60.6051776313845));
#63657=CARTESIAN_POINT('Origin',(0.,0.,59.5351776313845));
#63658=CARTESIAN_POINT('',(-1.83,2.24110364243966E-16,59.5351776313845));
#63659=CARTESIAN_POINT('Origin',(0.,0.,69.4601776313845));
#63660=CARTESIAN_POINT('',(0.,0.,70.5146880177779));
#63661=CARTESIAN_POINT('',(-1.755,-2.1492551325036E-16,69.4601776313845));
#63662=CARTESIAN_POINT('Origin',(4.425,4.425,59.4601776313845));
#63663=CARTESIAN_POINT('',(4.5,4.35,59.7601776313845));
#63664=CARTESIAN_POINT('',(4.5,4.35,59.4601776313845));
#63665=CARTESIAN_POINT('',(5.47500000000001,3.37499999999999,60.7351776313845));
#63666=CARTESIAN_POINT('Origin',(4.425,4.425,59.4601776313845));
#63667=CARTESIAN_POINT('',(4.5,4.35,59.4601776313845));
#63668=CARTESIAN_POINT('Origin',(4.5,-4.5,59.4601776313845));
#63669=CARTESIAN_POINT('',(4.5,-4.35,59.7601776313845));
#63670=CARTESIAN_POINT('',(4.5,-4.35,59.4601776313845));
#63671=CARTESIAN_POINT('',(4.5,-2.25,59.7601776313845));
#63672=CARTESIAN_POINT('Origin',(4.5,-4.5,59.4601776313845));
#63673=CARTESIAN_POINT('Origin',(4.5,-4.5,59.4601776313845));
#63674=CARTESIAN_POINT('Origin',(4.5,-4.5,59.4601776313845));
#63675=CARTESIAN_POINT('Origin',(4.5,-4.5,59.4601776313845));
#63676=CARTESIAN_POINT('Origin',(4.5,-4.5,59.4601776313845));
#63677=CARTESIAN_POINT('Origin',(4.5,-4.5,59.4601776313845));
#63678=CARTESIAN_POINT('Origin',(4.425,-4.425,59.4601776313845));
#63679=CARTESIAN_POINT('',(4.725,-4.125,59.9851776313845));
#63680=CARTESIAN_POINT('Origin',(4.425,-4.425,59.4601776313845));
#63681=CARTESIAN_POINT('Origin',(4.425,-4.425,59.4601776313845));
#63682=CARTESIAN_POINT('Origin',(4.425,-4.425,59.4601776313845));
#63683=CARTESIAN_POINT('Origin',(2.25,4.35,144.810177631385));
#63684=CARTESIAN_POINT('',(4.2,4.2,144.960177631385));
#63685=CARTESIAN_POINT('',(2.25,4.2,144.960177631385));
#63686=CARTESIAN_POINT('',(4.2,4.2,144.960177631385));
#63687=CARTESIAN_POINT('Origin',(4.35,-2.25,59.6101776313845));
#63688=CARTESIAN_POINT('',(4.2,4.2,59.4601776313845));
#63689=CARTESIAN_POINT('Origin',(4.35,-2.25,144.810177631385));
#63690=CARTESIAN_POINT('',(4.2,-2.25,144.960177631385));
#63691=CARTESIAN_POINT('Origin',(2.25,4.35,59.6101776313845));
#63692=CARTESIAN_POINT('Origin',(0.,0.,144.960177631385));
#63693=CARTESIAN_POINT('Origin',(-4.5,4.5,59.4601776313845));
#63694=CARTESIAN_POINT('',(0.,0.,0.));
#63695=CARTESIAN_POINT('Origin',(1.51164990307781,-1.90362339303322,56.979171306613));
#63696=CARTESIAN_POINT('',(1.46950013062437,-2.02251560342435,56.6));
#63697=CARTESIAN_POINT('',(1.55379967553124,-1.78473118264209,56.6));
#63698=CARTESIAN_POINT('',(1.54374745319659,-1.81308556899211,56.6));
#63699=CARTESIAN_POINT('',(1.55379967553124,-1.78473118264209,57.55834261));
#63700=CARTESIAN_POINT('',(1.55379967553124,-1.78473118264209,56.979171306613));
#63701=CARTESIAN_POINT('',(1.46950013062437,-2.02251560342435,57.55834261));
#63702=CARTESIAN_POINT('',(1.54374745319659,-1.81308556899211,57.55834261));
#63703=CARTESIAN_POINT('',(1.46950013062437,-2.02251560342435,56.979171306613));
#63704=CARTESIAN_POINT('Origin',(1.8031222920257,-1.8031222920257,56.6));
#63705=CARTESIAN_POINT('',(1.78473118264209,-1.55379967553124,56.6));
#63706=CARTESIAN_POINT('Origin',(1.8031222920257,-1.8031222920257,56.6));
#63707=CARTESIAN_POINT('',(1.78473118264209,-1.55379967553124,57.55834261));
#63708=CARTESIAN_POINT('',(1.78473118264209,-1.55379967553124,56.979171306613));
#63709=CARTESIAN_POINT('Origin',(1.8031222920257,-1.8031222920257,57.55834261));
#63710=CARTESIAN_POINT('Origin',(1.90362339303322,-1.51164990307781,56.979171306613));
#63711=CARTESIAN_POINT('',(2.02251560342435,-1.46950013062437,57.55834261));
#63712=CARTESIAN_POINT('',(1.81308556899211,-1.54374745319659,57.55834261));
#63713=CARTESIAN_POINT('',(2.02251560342435,-1.46950013062437,56.6));
#63714=CARTESIAN_POINT('',(1.81308556899211,-1.54374745319659,56.6));
#63715=CARTESIAN_POINT('',(2.02251560342435,-1.46950013062437,56.979171306613));
#63716=CARTESIAN_POINT('Origin',(-1.51164990307781,-1.90362339303322,56.979171306613));
#63717=CARTESIAN_POINT('',(-1.46950013062437,-2.02251560342435,57.55834261));
#63718=CARTESIAN_POINT('',(-1.55379967553124,-1.78473118264209,57.55834261));
#63719=CARTESIAN_POINT('',(-1.54374745319659,-1.81308556899211,57.55834261));
#63720=CARTESIAN_POINT('',(-1.55379967553124,-1.78473118264209,56.6));
#63721=CARTESIAN_POINT('',(-1.55379967553124,-1.78473118264209,56.979171306613));
#63722=CARTESIAN_POINT('',(-1.46950013062437,-2.02251560342435,56.6));
#63723=CARTESIAN_POINT('',(-1.54374745319659,-1.81308556899211,56.6));
#63724=CARTESIAN_POINT('',(-1.46950013062437,-2.02251560342435,56.979171306613));
#63725=CARTESIAN_POINT('Origin',(-1.8031222920257,-1.8031222920257,56.6));
#63726=CARTESIAN_POINT('',(-1.78473118264209,-1.55379967553124,57.55834261));
#63727=CARTESIAN_POINT('Origin',(-1.8031222920257,-1.8031222920257,57.55834261));
#63728=CARTESIAN_POINT('',(-1.78473118264209,-1.55379967553124,56.6));
#63729=CARTESIAN_POINT('',(-1.78473118264209,-1.55379967553124,56.979171306613));
#63730=CARTESIAN_POINT('Origin',(-1.8031222920257,-1.8031222920257,56.6));
#63731=CARTESIAN_POINT('Origin',(-1.90362339303322,-1.51164990307781,56.979171306613));
#63732=CARTESIAN_POINT('',(-2.02251560342435,-1.46950013062437,56.6));
#63733=CARTESIAN_POINT('',(-1.81308556899211,-1.54374745319659,56.6));
#63734=CARTESIAN_POINT('',(-2.02251560342435,-1.46950013062437,57.55834261));
#63735=CARTESIAN_POINT('',(-1.81308556899211,-1.54374745319659,57.55834261));
#63736=CARTESIAN_POINT('',(-2.02251560342435,-1.46950013062437,56.979171306613));
#63737=CARTESIAN_POINT('Origin',(2.41496290728544,-0.277167112792829,56.979171306613));
#63738=CARTESIAN_POINT('',(2.46922800555597,-0.391040990917948,56.6));
#63739=CARTESIAN_POINT('',(2.36069780901491,-0.16329323466771,56.6));
#63740=CARTESIAN_POINT('',(2.37363939330056,-0.190450808111023,56.6));
#63741=CARTESIAN_POINT('',(2.36069780901491,-0.16329323466771,57.55834261));
#63742=CARTESIAN_POINT('',(2.36069780901491,-0.16329323466771,56.979171306613));
#63743=CARTESIAN_POINT('',(2.46922800555597,-0.391040990917948,57.55834261));
#63744=CARTESIAN_POINT('',(2.37363939330056,-0.190450808111023,57.55834261));
#63745=CARTESIAN_POINT('',(2.46922800555597,-0.391040990917948,56.979171306613));
#63746=CARTESIAN_POINT('Origin',(2.55,0.,56.6));
#63747=CARTESIAN_POINT('',(2.36069780901491,0.16329323466771,56.6));
#63748=CARTESIAN_POINT('Origin',(2.55,0.,56.6));
#63749=CARTESIAN_POINT('',(2.36069780901491,0.16329323466771,57.55834261));
#63750=CARTESIAN_POINT('',(2.36069780901491,0.16329323466771,56.979171306613));
#63751=CARTESIAN_POINT('Origin',(2.55,0.,57.55834261));
#63752=CARTESIAN_POINT('Origin',(2.41496290728544,0.277167112792829,56.979171306613));
#63753=CARTESIAN_POINT('',(2.46922800555597,0.391040990917948,57.55834261));
#63754=CARTESIAN_POINT('',(2.37363939330056,0.190450808111023,57.55834261));
#63755=CARTESIAN_POINT('',(2.46922800555597,0.391040990917948,56.6));
#63756=CARTESIAN_POINT('',(2.37363939330056,0.190450808111023,56.6));
#63757=CARTESIAN_POINT('',(2.46922800555597,0.391040990917948,56.979171306613));
#63758=CARTESIAN_POINT('Origin',(-0.277167112792829,2.41496290728544,56.979171306613));
#63759=CARTESIAN_POINT('',(-0.391040990917948,2.46922800555597,57.55834261));
#63760=CARTESIAN_POINT('',(-0.16329323466771,2.36069780901491,57.55834261));
#63761=CARTESIAN_POINT('',(-0.190450808111023,2.37363939330056,57.55834261));
#63762=CARTESIAN_POINT('',(-0.16329323466771,2.36069780901491,56.6));
#63763=CARTESIAN_POINT('',(-0.16329323466771,2.36069780901491,56.979171306613));
#63764=CARTESIAN_POINT('',(-0.391040990917948,2.46922800555597,56.6));
#63765=CARTESIAN_POINT('',(-0.190450808111023,2.37363939330056,56.6));
#63766=CARTESIAN_POINT('',(-0.391040990917948,2.46922800555597,56.979171306613));
#63767=CARTESIAN_POINT('Origin',(1.56142466891288E-16,2.55,56.6));
#63768=CARTESIAN_POINT('',(0.163293234667711,2.36069780901491,57.55834261));
#63769=CARTESIAN_POINT('Origin',(1.56142466891288E-16,2.55,57.55834261));
#63770=CARTESIAN_POINT('',(0.163293234667711,2.36069780901491,56.6));
#63771=CARTESIAN_POINT('',(0.163293234667711,2.36069780901491,56.979171306613));
#63772=CARTESIAN_POINT('Origin',(1.56142466891288E-16,2.55,56.6));
#63773=CARTESIAN_POINT('Origin',(0.277167112792829,2.41496290728544,56.979171306613));
#63774=CARTESIAN_POINT('',(0.391040990917948,2.46922800555597,56.6));
#63775=CARTESIAN_POINT('',(0.190450808111023,2.37363939330056,56.6));
#63776=CARTESIAN_POINT('',(0.391040990917948,2.46922800555597,57.55834261));
#63777=CARTESIAN_POINT('',(0.190450808111023,2.37363939330056,57.55834261));
#63778=CARTESIAN_POINT('',(0.391040990917948,2.46922800555597,56.979171306613));
#63779=CARTESIAN_POINT('Origin',(1.90362339303322,1.51164990307781,56.979171306613));
#63780=CARTESIAN_POINT('',(2.02251560342435,1.46950013062437,56.6));
#63781=CARTESIAN_POINT('',(1.78473118264209,1.55379967553124,56.6));
#63782=CARTESIAN_POINT('',(1.81308556899211,1.54374745319659,56.6));
#63783=CARTESIAN_POINT('',(1.78473118264209,1.55379967553124,57.55834261));
#63784=CARTESIAN_POINT('',(1.78473118264209,1.55379967553124,56.979171306613));
#63785=CARTESIAN_POINT('',(2.02251560342435,1.46950013062437,57.55834261));
#63786=CARTESIAN_POINT('',(1.81308556899211,1.54374745319659,57.55834261));
#63787=CARTESIAN_POINT('',(2.02251560342435,1.46950013062437,56.979171306613));
#63788=CARTESIAN_POINT('Origin',(1.8031222920257,1.8031222920257,56.6));
#63789=CARTESIAN_POINT('',(1.55379967553124,1.78473118264209,56.6));
#63790=CARTESIAN_POINT('Origin',(1.8031222920257,1.8031222920257,56.6));
#63791=CARTESIAN_POINT('',(1.55379967553124,1.78473118264209,57.55834261));
#63792=CARTESIAN_POINT('',(1.55379967553124,1.78473118264209,56.979171306613));
#63793=CARTESIAN_POINT('Origin',(1.8031222920257,1.8031222920257,57.55834261));
#63794=CARTESIAN_POINT('Origin',(1.51164990307781,1.90362339303322,56.979171306613));
#63795=CARTESIAN_POINT('',(1.46950013062437,2.02251560342435,57.55834261));
#63796=CARTESIAN_POINT('',(1.54374745319659,1.81308556899211,57.55834261));
#63797=CARTESIAN_POINT('',(1.46950013062437,2.02251560342435,56.6));
#63798=CARTESIAN_POINT('',(1.54374745319659,1.81308556899211,56.6));
#63799=CARTESIAN_POINT('',(1.46950013062437,2.02251560342435,56.979171306613));
#63800=CARTESIAN_POINT('Origin',(-1.90362339303322,1.51164990307781,56.979171306613));
#63801=CARTESIAN_POINT('',(-2.02251560342435,1.46950013062437,57.55834261));
#63802=CARTESIAN_POINT('',(-1.78473118264209,1.55379967553124,57.55834261));
#63803=CARTESIAN_POINT('',(-1.81308556899211,1.54374745319659,57.55834261));
#63804=CARTESIAN_POINT('',(-1.78473118264209,1.55379967553124,56.6));
#63805=CARTESIAN_POINT('',(-1.78473118264209,1.55379967553124,56.979171306613));
#63806=CARTESIAN_POINT('',(-2.02251560342435,1.46950013062437,56.6));
#63807=CARTESIAN_POINT('',(-1.81308556899211,1.54374745319659,56.6));
#63808=CARTESIAN_POINT('',(-2.02251560342435,1.46950013062437,56.979171306613));
#63809=CARTESIAN_POINT('Origin',(-1.8031222920257,1.8031222920257,56.6));
#63810=CARTESIAN_POINT('',(-1.55379967553124,1.78473118264209,57.55834261));
#63811=CARTESIAN_POINT('Origin',(-1.8031222920257,1.8031222920257,57.55834261));
#63812=CARTESIAN_POINT('',(-1.55379967553124,1.78473118264209,56.6));
#63813=CARTESIAN_POINT('',(-1.55379967553124,1.78473118264209,56.979171306613));
#63814=CARTESIAN_POINT('Origin',(-1.8031222920257,1.8031222920257,56.6));
#63815=CARTESIAN_POINT('Origin',(-1.51164990307781,1.90362339303322,56.979171306613));
#63816=CARTESIAN_POINT('',(-1.46950013062437,2.02251560342435,56.6));
#63817=CARTESIAN_POINT('',(-1.54374745319659,1.81308556899211,56.6));
#63818=CARTESIAN_POINT('',(-1.46950013062437,2.02251560342435,57.55834261));
#63819=CARTESIAN_POINT('',(-1.54374745319659,1.81308556899211,57.55834261));
#63820=CARTESIAN_POINT('',(-1.46950013062437,2.02251560342435,56.979171306613));
#63821=CARTESIAN_POINT('Origin',(-2.41496290728544,-0.277167112792829,56.979171306613));
#63822=CARTESIAN_POINT('',(-2.46922800555597,-0.391040990917948,57.55834261));
#63823=CARTESIAN_POINT('',(-2.36069780901491,-0.16329323466771,57.55834261));
#63824=CARTESIAN_POINT('',(-2.37363939330056,-0.190450808111022,57.55834261));
#63825=CARTESIAN_POINT('',(-2.36069780901491,-0.16329323466771,56.6));
#63826=CARTESIAN_POINT('',(-2.36069780901491,-0.16329323466771,56.979171306613));
#63827=CARTESIAN_POINT('',(-2.46922800555597,-0.391040990917948,56.6));
#63828=CARTESIAN_POINT('',(-2.37363939330056,-0.190450808111022,56.6));
#63829=CARTESIAN_POINT('',(-2.46922800555597,-0.391040990917948,56.979171306613));
#63830=CARTESIAN_POINT('Origin',(-2.55,3.12284933782575E-16,56.6));
#63831=CARTESIAN_POINT('',(-2.36069780901491,0.163293234667711,57.55834261));
#63832=CARTESIAN_POINT('Origin',(-2.55,3.12284933782575E-16,57.55834261));
#63833=CARTESIAN_POINT('',(-2.36069780901491,0.163293234667711,56.6));
#63834=CARTESIAN_POINT('',(-2.36069780901491,0.163293234667711,56.979171306613));
#63835=CARTESIAN_POINT('Origin',(-2.55,3.12284933782575E-16,56.6));
#63836=CARTESIAN_POINT('Origin',(-2.41496290728544,0.27716711279283,56.979171306613));
#63837=CARTESIAN_POINT('',(-2.46922800555597,0.391040990917948,56.6));
#63838=CARTESIAN_POINT('',(-2.37363939330056,0.190450808111023,56.6));
#63839=CARTESIAN_POINT('',(-2.46922800555597,0.391040990917948,57.55834261));
#63840=CARTESIAN_POINT('',(-2.37363939330056,0.190450808111023,57.55834261));
#63841=CARTESIAN_POINT('',(-2.46922800555597,0.391040990917948,56.979171306613));
#63842=CARTESIAN_POINT('Origin',(0.277167112792829,-2.41496290728544,56.979171306613));
#63843=CARTESIAN_POINT('',(0.391040990917948,-2.46922800555597,57.55834261));
#63844=CARTESIAN_POINT('',(0.16329323466771,-2.36069780901491,57.55834261));
#63845=CARTESIAN_POINT('',(0.190450808111022,-2.37363939330056,57.55834261));
#63846=CARTESIAN_POINT('',(0.16329323466771,-2.36069780901491,56.6));
#63847=CARTESIAN_POINT('',(0.16329323466771,-2.36069780901491,56.979171306613));
#63848=CARTESIAN_POINT('',(0.391040990917948,-2.46922800555597,56.6));
#63849=CARTESIAN_POINT('',(0.190450808111022,-2.37363939330056,56.6));
#63850=CARTESIAN_POINT('',(0.391040990917948,-2.46922800555597,56.979171306613));
#63851=CARTESIAN_POINT('Origin',(-4.68427400673863E-16,-2.55,56.6));
#63852=CARTESIAN_POINT('',(-0.163293234667711,-2.36069780901491,57.55834261));
#63853=CARTESIAN_POINT('Origin',(-4.68427400673863E-16,-2.55,57.55834261));
#63854=CARTESIAN_POINT('',(-0.163293234667711,-2.36069780901491,56.6));
#63855=CARTESIAN_POINT('',(-0.163293234667711,-2.36069780901491,56.979171306613));
#63856=CARTESIAN_POINT('Origin',(-4.68427400673863E-16,-2.55,56.6));
#63857=CARTESIAN_POINT('Origin',(-0.27716711279283,-2.41496290728544,56.979171306613));
#63858=CARTESIAN_POINT('',(-0.391040990917949,-2.46922800555597,56.6));
#63859=CARTESIAN_POINT('',(-0.190450808111023,-2.37363939330056,56.6));
#63860=CARTESIAN_POINT('',(-0.391040990917949,-2.46922800555597,57.55834261));
#63861=CARTESIAN_POINT('',(-0.190450808111023,-2.37363939330056,57.55834261));
#63862=CARTESIAN_POINT('',(-0.391040990917949,-2.46922800555597,56.979171306613));
#63863=CARTESIAN_POINT('Origin',(-4.44089209850063E-16,-2.55,57.55834261));
#63864=CARTESIAN_POINT('Origin',(0.,0.,57.55834261));
#63865=CARTESIAN_POINT('Origin',(-4.44089209850063E-16,-2.55,56.6));
#63866=CARTESIAN_POINT('Origin',(0.,0.,56.6));
#63867=CARTESIAN_POINT('Origin',(-2.55,3.19189119579733E-16,57.55834261));
#63868=CARTESIAN_POINT('',(-2.5,-3.06161699786838E-16,57.55834261));
#63869=CARTESIAN_POINT('Origin',(0.,0.,57.55834261));
#63870=CARTESIAN_POINT('Origin',(0.,0.,57.55834261));
#63871=CARTESIAN_POINT('Origin',(-2.55,3.19189119579733E-16,56.6));
#63872=CARTESIAN_POINT('',(-2.5,-3.06161699786838E-16,56.6));
#63873=CARTESIAN_POINT('Origin',(0.,0.,56.6));
#63874=CARTESIAN_POINT('Origin',(0.,0.,56.6));
#63875=CARTESIAN_POINT('Origin',(-1.8031222920257,1.8031222920257,57.55834261));
#63876=CARTESIAN_POINT('Origin',(0.,0.,57.55834261));
#63877=CARTESIAN_POINT('Origin',(-1.8031222920257,1.8031222920257,56.6));
#63878=CARTESIAN_POINT('Origin',(0.,0.,56.6));
#63879=CARTESIAN_POINT('Origin',(1.8031222920257,1.8031222920257,56.6));
#63880=CARTESIAN_POINT('Origin',(0.,0.,56.6));
#63881=CARTESIAN_POINT('Origin',(1.8031222920257,1.8031222920257,57.55834261));
#63882=CARTESIAN_POINT('Origin',(0.,0.,57.55834261));
#63883=CARTESIAN_POINT('Origin',(1.66533453693773E-16,2.55,57.55834261));
#63884=CARTESIAN_POINT('Origin',(0.,0.,57.55834261));
#63885=CARTESIAN_POINT('Origin',(1.66533453693773E-16,2.55,56.6));
#63886=CARTESIAN_POINT('Origin',(0.,0.,56.6));
#63887=CARTESIAN_POINT('Origin',(2.55,0.,56.6));
#63888=CARTESIAN_POINT('Origin',(0.,0.,56.6));
#63889=CARTESIAN_POINT('Origin',(2.55,0.,57.55834261));
#63890=CARTESIAN_POINT('Origin',(0.,0.,57.55834261));
#63891=CARTESIAN_POINT('Origin',(-1.8031222920257,-1.8031222920257,57.55834261));
#63892=CARTESIAN_POINT('Origin',(0.,0.,57.55834261));
#63893=CARTESIAN_POINT('Origin',(-1.8031222920257,-1.8031222920257,56.6));
#63894=CARTESIAN_POINT('Origin',(0.,0.,56.6));
#63895=CARTESIAN_POINT('Origin',(1.8031222920257,-1.8031222920257,56.6));
#63896=CARTESIAN_POINT('Origin',(0.,0.,56.6));
#63897=CARTESIAN_POINT('Origin',(1.8031222920257,-1.8031222920257,57.55834261));
#63898=CARTESIAN_POINT('Origin',(0.,0.,57.55834261));
#63899=CARTESIAN_POINT('Origin',(0.,0.,56.035));
#63900=CARTESIAN_POINT('',(-1.3,-1.59204083889156E-16,56.));
#63901=CARTESIAN_POINT('Origin',(0.,0.,56.));
#63902=CARTESIAN_POINT('',(-1.3,-1.59204083889156E-16,56.1));
#63903=CARTESIAN_POINT('',(-1.3,-1.59204083889156E-16,56.035));
#63904=CARTESIAN_POINT('Origin',(0.,0.,56.1));
#63905=CARTESIAN_POINT('Origin',(1.205,0.,56.1));
#63906=CARTESIAN_POINT('',(-1.205,-1.47569939297256E-16,56.1));
#63907=CARTESIAN_POINT('Origin',(0.,0.,56.1));
#63908=CARTESIAN_POINT('Origin',(0.,0.,58.3));
#63909=CARTESIAN_POINT('',(-1.205,-1.47569939297256E-16,60.5));
#63910=CARTESIAN_POINT('',(-1.205,-1.47569939297256E-16,58.3));
#63911=CARTESIAN_POINT('Origin',(0.,0.,60.5));
#63912=CARTESIAN_POINT('Origin',(0.,0.,60.5));
#63913=CARTESIAN_POINT('',(0.,0.,61.2240370459282));
#63914=CARTESIAN_POINT('',(-1.205,-1.47569939297256E-16,60.5));
#63915=CARTESIAN_POINT('Origin',(2.3,0.,56.));
#63916=CARTESIAN_POINT('',(-2.3,-2.81668763803891E-16,56.));
#63917=CARTESIAN_POINT('Origin',(0.,0.,56.));
#63918=CARTESIAN_POINT('Origin',(0.,0.,56.1));
#63919=CARTESIAN_POINT('',(-2.5,-3.06161699786838E-16,56.2));
#63920=CARTESIAN_POINT('Origin',(0.,0.,56.2));
#63921=CARTESIAN_POINT('',(-2.4,-2.93915231795365E-16,56.1));
#63922=CARTESIAN_POINT('Origin',(0.,0.,56.979171306613));
#63923=CARTESIAN_POINT('',(-2.5,-3.06161699786838E-16,57.7583426132261));
#63924=CARTESIAN_POINT('Origin',(0.,0.,57.7583426132261));
#63925=CARTESIAN_POINT('',(-2.5,-3.06161699786838E-16,56.979171306613));
#63926=CARTESIAN_POINT('',(-2.5,-3.06161699786838E-16,56.979171306613));
#63927=CARTESIAN_POINT('Origin',(4.44089209850063E-16,0.,61.5));
#63928=CARTESIAN_POINT('',(1.68543680041908E-16,-3.37445951098918E-32,66.));
#63929=CARTESIAN_POINT('Origin',(4.44089209850063E-16,0.,61.5));
#63930=CARTESIAN_POINT('',(0.,0.,0.));
#63931=CARTESIAN_POINT('Origin',(9.31,4.82,78.));
#63932=CARTESIAN_POINT('',(5.02549199084668,4.82,73.4428061134618));
#63933=CARTESIAN_POINT('',(3.055,4.82,78.));
#63934=CARTESIAN_POINT('Origin',(9.31,4.82,78.));
#63935=CARTESIAN_POINT('',(5.02549199084668,4.82,82.5571938865382));
#63936=CARTESIAN_POINT('Origin',(9.31,4.82,78.));
#63937=CARTESIAN_POINT('',(4.60618911786999,4.52,82.565324543245));
#63938=CARTESIAN_POINT('Ctrl Pts',(5.02549199084668,4.82,82.5571938865382));
#63939=CARTESIAN_POINT('Ctrl Pts',(5.02530843195014,4.81974208420639,82.5570213111372));
#63940=CARTESIAN_POINT('Ctrl Pts',(5.02512465556946,4.81948416828985,82.556848966888));
#63941=CARTESIAN_POINT('Ctrl Pts',(4.98582218891929,4.76439138566817,82.5200843217974));
#63942=CARTESIAN_POINT('Ctrl Pts',(4.93753334401095,4.71048862403654,82.4945375858532));
#63943=CARTESIAN_POINT('Ctrl Pts',(4.84464785310685,4.6276739222328,82.4739443292949));
#63944=CARTESIAN_POINT('Ctrl Pts',(4.80287073114975,4.59679810761626,82.4733979122501));
#63945=CARTESIAN_POINT('Ctrl Pts',(4.73196607374269,4.55526307036662,82.4873225644575));
#63946=CARTESIAN_POINT('Ctrl Pts',(4.70113087228767,4.54073321204008,82.4982082535911));
#63947=CARTESIAN_POINT('Ctrl Pts',(4.64789443637829,4.52392737915209,82.5285504834486));
#63948=CARTESIAN_POINT('Ctrl Pts',(4.62586036645017,4.52,82.5453381759243));
#63949=CARTESIAN_POINT('Ctrl Pts',(4.60618911787,4.52,82.565324543245));
#63950=CARTESIAN_POINT('',(4.60618911786999,4.52,73.434675456755));
#63951=CARTESIAN_POINT('Origin',(9.31,4.52,78.));
#63952=CARTESIAN_POINT('Ctrl Pts',(4.60618911787001,4.52,73.434675456755));
#63953=CARTESIAN_POINT('Ctrl Pts',(4.62582177000828,4.52,73.4546226093476));
#63954=CARTESIAN_POINT('Ctrl Pts',(4.64779152745104,4.52391160862118,73.4713675032503));
#63955=CARTESIAN_POINT('Ctrl Pts',(4.69786840426422,4.53968449182505,73.4999585882815));
#63956=CARTESIAN_POINT('Ctrl Pts',(4.72544220605375,4.55223271719695,73.5103111906513));
#63957=CARTESIAN_POINT('Ctrl Pts',(4.78901185813479,4.58789763273166,73.5249530214543));
#63958=CARTESIAN_POINT('Ctrl Pts',(4.82447324095024,4.61297821285604,73.5260203885605));
#63959=CARTESIAN_POINT('Ctrl Pts',(4.88969454090697,4.66653559525648,73.5178493906711));
#63960=CARTESIAN_POINT('Ctrl Pts',(4.92001482640919,4.69535645684422,73.5086915524274));
#63961=CARTESIAN_POINT('Ctrl Pts',(4.97624170572235,4.75557099156908,73.4823061485807));
#63962=CARTESIAN_POINT('Ctrl Pts',(5.002315693931,4.78751138710799,73.4644871845292));
#63963=CARTESIAN_POINT('Ctrl Pts',(5.0251246555687,4.8194841682894,73.4431510331127));
#63964=CARTESIAN_POINT('Ctrl Pts',(5.02530843195051,4.81974208420691,73.4429786888625));
#63965=CARTESIAN_POINT('Ctrl Pts',(5.02549199084668,4.82,73.4428061134618));
#63966=CARTESIAN_POINT('Origin',(4.82,0.,82.7757643367319));
#63967=CARTESIAN_POINT('',(4.52,-4.52,82.7757643367319));
#63968=CARTESIAN_POINT('',(4.52,4.52,82.7757643367319));
#63969=CARTESIAN_POINT('',(4.52,0.,82.7757643367319));
#63970=CARTESIAN_POINT('Origin',(4.82,4.52,82.7757643367319));
#63971=CARTESIAN_POINT('',(5.02549199084668,-4.82,82.5571938865382));
#63972=CARTESIAN_POINT('',(5.02549199084668,0.,82.5571938865382));
#63973=CARTESIAN_POINT('',(4.60618911786999,-4.52,82.565324543245));
#63974=CARTESIAN_POINT('Ctrl Pts',(5.02549199084668,-4.82,82.5571938865382));
#63975=CARTESIAN_POINT('Ctrl Pts',(5.02530843195014,-4.81974208420639,82.5570213111372));
#63976=CARTESIAN_POINT('Ctrl Pts',(5.02512465556946,-4.81948416828985,82.556848966888));
#63977=CARTESIAN_POINT('Ctrl Pts',(4.98582218891934,-4.76439138566824,82.5200843217975));
#63978=CARTESIAN_POINT('Ctrl Pts',(4.93753334401101,-4.7104886240366,82.4945375858533));
#63979=CARTESIAN_POINT('Ctrl Pts',(4.8446478531067,-4.62767392223266,82.4739443292949));
#63980=CARTESIAN_POINT('Ctrl Pts',(4.80287073114959,-4.59679810761617,82.4733979122501));
#63981=CARTESIAN_POINT('Ctrl Pts',(4.73196607374269,-4.55526307036662,82.4873225644575));
#63982=CARTESIAN_POINT('Ctrl Pts',(4.70113087228767,-4.54073321204007,82.4982082535911));
#63983=CARTESIAN_POINT('Ctrl Pts',(4.64789443637828,-4.52392737915208,82.5285504834486));
#63984=CARTESIAN_POINT('Ctrl Pts',(4.62586036645016,-4.52,82.5453381759243));
#63985=CARTESIAN_POINT('Ctrl Pts',(4.60618911786998,-4.52,82.565324543245));
#63986=CARTESIAN_POINT('Origin',(4.82,-4.52,82.7757643367319));
#63987=CARTESIAN_POINT('Origin',(4.82,0.,73.2242356632681));
#63988=CARTESIAN_POINT('',(5.02549199084668,-4.82,73.4428061134618));
#63989=CARTESIAN_POINT('',(5.02549199084668,0.,73.4428061134618));
#63990=CARTESIAN_POINT('',(4.52,4.52,73.2242356632681));
#63991=CARTESIAN_POINT('Origin',(4.82,4.52,73.2242356632681));
#63992=CARTESIAN_POINT('',(4.52,-4.52,73.2242356632681));
#63993=CARTESIAN_POINT('',(4.52,0.,73.2242356632681));
#63994=CARTESIAN_POINT('',(4.60618911786999,-4.52,73.434675456755));
#63995=CARTESIAN_POINT('Origin',(4.82,-4.52,73.2242356632681));
#63996=CARTESIAN_POINT('Ctrl Pts',(4.60618911787,-4.52,73.434675456755));
#63997=CARTESIAN_POINT('Ctrl Pts',(4.62582177000827,-4.52,73.4546226093476));
#63998=CARTESIAN_POINT('Ctrl Pts',(4.64779152745104,-4.52391160862118,73.4713675032503));
#63999=CARTESIAN_POINT('Ctrl Pts',(4.69786840426422,-4.53968449182505,73.4999585882815));
#64000=CARTESIAN_POINT('Ctrl Pts',(4.72544220605375,-4.55223271719695,73.5103111906513));
#64001=CARTESIAN_POINT('Ctrl Pts',(4.78901185813476,-4.58789763273165,73.5249530214543));
#64002=CARTESIAN_POINT('Ctrl Pts',(4.82447324095018,-4.612978212856,73.5260203885605));
#64003=CARTESIAN_POINT('Ctrl Pts',(4.88969454090694,-4.66653559525646,73.5178493906711));
#64004=CARTESIAN_POINT('Ctrl Pts',(4.92001482640915,-4.69535645684417,73.5086915524274));
#64005=CARTESIAN_POINT('Ctrl Pts',(4.9762417057226,-4.75557099156931,73.4823061485806));
#64006=CARTESIAN_POINT('Ctrl Pts',(5.00231569392393,-4.78751138711695,73.4644871845359));
#64007=CARTESIAN_POINT('Ctrl Pts',(5.02512465556945,-4.81948416828983,73.443151033112));
#64008=CARTESIAN_POINT('Ctrl Pts',(5.02530843194999,-4.81974208420617,73.442978688863));
#64009=CARTESIAN_POINT('Ctrl Pts',(5.02549199084668,-4.82,73.4428061134618));
#64010=CARTESIAN_POINT('Origin',(9.31,-4.82,78.));
#64011=CARTESIAN_POINT('',(3.055,-4.82,78.));
#64012=CARTESIAN_POINT('Origin',(9.31,-4.82,78.));
#64013=CARTESIAN_POINT('Origin',(9.31,-4.82,78.));
#64014=CARTESIAN_POINT('Origin',(9.31,-4.52,78.));
#64015=CARTESIAN_POINT('Origin',(4.52,-4.52,62.));
#64016=CARTESIAN_POINT('',(4.52,4.52,64.2));
#64017=CARTESIAN_POINT('',(4.52,4.52,62.));
#64018=CARTESIAN_POINT('',(4.52,-4.52,64.2));
#64019=CARTESIAN_POINT('',(4.52,-2.26,64.2));
#64020=CARTESIAN_POINT('',(4.52,-4.52,62.));
#64021=CARTESIAN_POINT('Origin',(4.52,4.52,62.));
#64022=CARTESIAN_POINT('',(4.52,4.52,91.8));
#64023=CARTESIAN_POINT('',(4.52,4.52,62.));
#64024=CARTESIAN_POINT('',(-6.1,4.52,91.8));
#64025=CARTESIAN_POINT('',(-0.74,4.52,91.8));
#64026=CARTESIAN_POINT('',(-6.1,4.52,64.3216946934853));
#64027=CARTESIAN_POINT('',(-6.1,4.52,62.));
#64028=CARTESIAN_POINT('',(-6.1257913174651,4.52,64.2));
#64029=CARTESIAN_POINT('Origin',(-6.4,4.52,64.3216946934853));
#64030=CARTESIAN_POINT('',(14.26,4.52,64.2));
#64031=CARTESIAN_POINT('Origin',(9.31,0.,78.));
#64032=CARTESIAN_POINT('',(3.055,-13.8,78.));
#64033=CARTESIAN_POINT('Origin',(9.31,-13.8,78.));
#64034=CARTESIAN_POINT('',(3.055,0.,78.));
#64035=CARTESIAN_POINT('',(3.055,13.8,78.));
#64036=CARTESIAN_POINT('',(3.055,0.,78.));
#64037=CARTESIAN_POINT('Origin',(9.31,13.8,78.));
#64038=CARTESIAN_POINT('Origin',(-11.7,-4.3,5.5));
#64039=CARTESIAN_POINT('',(-11.9,-4.07639320225002,0.100000000000002));
#64040=CARTESIAN_POINT('',(-12.,-4.3,0.2));
#64041=CARTESIAN_POINT('Origin',(-11.7,-4.3,-0.0999999999999988));
#64042=CARTESIAN_POINT('',(-12.,-4.3,10.7));
#64043=CARTESIAN_POINT('',(-12.,-4.3,5.5));
#64044=CARTESIAN_POINT('',(-11.7,-4.,11.));
#64045=CARTESIAN_POINT('Origin',(-11.7,-4.3,11.));
#64046=CARTESIAN_POINT('',(-11.7,-4.,0.300000000000001));
#64047=CARTESIAN_POINT('',(-11.7,-4.,5.5));
#64048=CARTESIAN_POINT('Origin',(-11.7,-4.3,0.300000000000001));
#64049=CARTESIAN_POINT('Origin',(0.,-4.,11.));
#64050=CARTESIAN_POINT('',(0.,-4.,11.));
#64051=CARTESIAN_POINT('',(11.75,-4.,11.));
#64052=CARTESIAN_POINT('',(0.,-4.,5.3));
#64053=CARTESIAN_POINT('',(0.,-4.,11.));
#64054=CARTESIAN_POINT('',(-6.3,-4.,5.3));
#64055=CARTESIAN_POINT('',(10.5,-4.,5.3));
#64056=CARTESIAN_POINT('',(-6.3,-4.,0.300000000000001));
#64057=CARTESIAN_POINT('',(-6.3,-4.,5.5));
#64058=CARTESIAN_POINT('',(11.75,-4.,0.300000000000001));
#64059=CARTESIAN_POINT('Origin',(-11.85,9.5,10.85));
#64060=CARTESIAN_POINT('',(-12.,-17.5,10.7));
#64061=CARTESIAN_POINT('',(-12.,9.5,10.7));
#64062=CARTESIAN_POINT('',(-11.7,-17.5,11.));
#64063=CARTESIAN_POINT('',(-11.7,-17.5,11.));
#64064=CARTESIAN_POINT('',(-11.7,9.5,11.));
#64065=CARTESIAN_POINT('Origin',(-12.,19.,0.));
#64066=CARTESIAN_POINT('',(-12.,-17.5,0.2));
#64067=CARTESIAN_POINT('',(-12.,9.5,0.2));
#64068=CARTESIAN_POINT('',(-12.,-17.5,0.));
#64069=CARTESIAN_POINT('Origin',(-11.7,4.3,5.5));
#64070=CARTESIAN_POINT('',(-11.7,4.,11.));
#64071=CARTESIAN_POINT('',(-12.,4.3,10.7));
#64072=CARTESIAN_POINT('Origin',(-11.7,4.3,11.));
#64073=CARTESIAN_POINT('',(-12.,4.3,0.2));
#64074=CARTESIAN_POINT('',(-12.,4.3,5.5));
#64075=CARTESIAN_POINT('',(-11.9,4.07639320225002,0.1));
#64076=CARTESIAN_POINT('Origin',(-11.7,4.3,-0.0999999999999988));
#64077=CARTESIAN_POINT('',(-11.7,4.,0.300000000000001));
#64078=CARTESIAN_POINT('Origin',(-11.7,4.3,0.300000000000001));
#64079=CARTESIAN_POINT('',(-11.7,4.,5.5));
#64080=CARTESIAN_POINT('Origin',(-11.85,9.5,10.85));
#64081=CARTESIAN_POINT('',(-11.7,17.5,11.));
#64082=CARTESIAN_POINT('',(-11.7,9.5,11.));
#64083=CARTESIAN_POINT('',(-12.,17.5,10.7));
#64084=CARTESIAN_POINT('',(-11.7,17.5,11.));
#64085=CARTESIAN_POINT('',(-12.,9.5,10.7));
#64086=CARTESIAN_POINT('Origin',(-12.5,4.,11.));
#64087=CARTESIAN_POINT('',(-6.3,4.,0.300000000000001));
#64088=CARTESIAN_POINT('',(5.5,4.,0.300000000000001));
#64089=CARTESIAN_POINT('',(-6.3,4.,5.3));
#64090=CARTESIAN_POINT('',(-6.3,4.,5.5));
#64091=CARTESIAN_POINT('',(0.,4.,5.3));
#64092=CARTESIAN_POINT('',(4.25,4.,5.3));
#64093=CARTESIAN_POINT('',(0.,4.,11.));
#64094=CARTESIAN_POINT('',(0.,4.,11.));
#64095=CARTESIAN_POINT('',(5.5,4.,11.));
#64096=CARTESIAN_POINT('Origin',(5.5,4.3,0.300000000000001));
#64097=CARTESIAN_POINT('',(-11.8,4.3,0.));
#64098=CARTESIAN_POINT('Origin',(-12.1,4.3,0.300000000000001));
#64099=CARTESIAN_POINT('',(-6.3,4.3,0.));
#64100=CARTESIAN_POINT('',(5.5,4.3,0.));
#64101=CARTESIAN_POINT('Origin',(-6.3,4.3,0.300000000000001));
#64102=CARTESIAN_POINT('Origin',(-6.3,-4.3,0.3));
#64103=CARTESIAN_POINT('',(-6.3,-4.3,0.));
#64104=CARTESIAN_POINT('Origin',(-6.3,-4.3,0.300000000000001));
#64105=CARTESIAN_POINT('',(-6.,-4.3,0.3));
#64106=CARTESIAN_POINT('Origin',(-6.3,-4.3,0.3));
#64107=CARTESIAN_POINT('Origin',(-6.3,-4.3,0.3));
#64108=CARTESIAN_POINT('Origin',(-6.3,-4.3,5.5));
#64109=CARTESIAN_POINT('',(-6.,-4.3,5.));
#64110=CARTESIAN_POINT('',(-6.,-4.3,5.5));
#64111=CARTESIAN_POINT('Origin',(-6.3,-4.3,5.3));
#64112=CARTESIAN_POINT('Origin',(-6.3,4.3,0.300000000000001));
#64113=CARTESIAN_POINT('',(-6.,4.3,0.3));
#64114=CARTESIAN_POINT('Origin',(-6.3,4.3,0.300000000000001));
#64115=CARTESIAN_POINT('Origin',(-6.3,4.3,0.3));
#64116=CARTESIAN_POINT('Origin',(35.75,11.3,0.3));
#64117=CARTESIAN_POINT('',(48.,11.,0.3));
#64118=CARTESIAN_POINT('',(-6.,11.,0.3));
#64119=CARTESIAN_POINT('',(35.75,11.,0.3));
#64120=CARTESIAN_POINT('',(-6.3,11.3,0.));
#64121=CARTESIAN_POINT('Origin',(-6.3,11.3,0.3));
#64122=CARTESIAN_POINT('',(48.3,11.3,0.));
#64123=CARTESIAN_POINT('',(35.75,11.3,0.));
#64124=CARTESIAN_POINT('Origin',(48.3,11.3,0.3));
#64125=CARTESIAN_POINT('Origin',(-6.3,5.5,0.3));
#64126=CARTESIAN_POINT('',(-6.,5.5,0.3));
#64127=CARTESIAN_POINT('',(-6.3,5.5,0.));
#64128=CARTESIAN_POINT('Origin',(-6.3,4.3,5.5));
#64129=CARTESIAN_POINT('',(-6.,4.3,5.));
#64130=CARTESIAN_POINT('',(-6.,4.3,5.5));
#64131=CARTESIAN_POINT('Origin',(-6.3,4.3,5.3));
#64132=CARTESIAN_POINT('Origin',(48.3,-5.5,0.3));
#64133=CARTESIAN_POINT('',(48.,-11.,0.3));
#64134=CARTESIAN_POINT('',(48.,-5.5,0.3));
#64135=CARTESIAN_POINT('',(48.3,-11.3,0.));
#64136=CARTESIAN_POINT('',(48.3,-5.5,0.));
#64137=CARTESIAN_POINT('Origin',(48.3,-11.3,0.3));
#64138=CARTESIAN_POINT('Origin',(4.25,4.3,5.3));
#64139=CARTESIAN_POINT('',(0.,4.3,5.));
#64140=CARTESIAN_POINT('',(4.25,4.3,5.));
#64141=CARTESIAN_POINT('Origin',(0.,4.3,5.3));
#64142=CARTESIAN_POINT('Origin',(0.,0.,5.3));
#64143=CARTESIAN_POINT('',(0.,-4.3,5.));
#64144=CARTESIAN_POINT('Origin',(0.,-4.3,5.3));
#64145=CARTESIAN_POINT('Origin',(0.,0.,5.3));
#64146=CARTESIAN_POINT('Origin',(0.,0.,5.));
#64147=CARTESIAN_POINT('Origin',(10.5,-4.3,5.3));
#64148=CARTESIAN_POINT('',(10.5,-4.3,5.));
#64149=CARTESIAN_POINT('Origin',(8.75,-11.3,0.3));
#64150=CARTESIAN_POINT('',(-6.,-11.,0.3));
#64151=CARTESIAN_POINT('',(8.75,-11.,0.3));
#64152=CARTESIAN_POINT('',(-6.3,-11.3,0.));
#64153=CARTESIAN_POINT('',(8.75,-11.3,0.));
#64154=CARTESIAN_POINT('Origin',(-6.3,-11.3,0.3));
#64155=CARTESIAN_POINT('Origin',(-6.3,5.5,0.3));
#64156=CARTESIAN_POINT('',(-6.3,5.5,0.));
#64157=CARTESIAN_POINT('',(-6.,5.5,0.3));
#64158=CARTESIAN_POINT('Origin',(11.75,-4.3,0.300000000000001));
#64159=CARTESIAN_POINT('',(-11.8,-4.3,0.));
#64160=CARTESIAN_POINT('',(11.75,-4.3,0.));
#64161=CARTESIAN_POINT('Origin',(-12.1,-4.3,0.300000000000001));
#64162=CARTESIAN_POINT('Origin',(-11.9,9.5,0.1));
#64163=CARTESIAN_POINT('',(-11.8,-17.5,0.));
#64164=CARTESIAN_POINT('',(-11.8,9.5,0.));
#64165=CARTESIAN_POINT('',(-11.8,-17.5,0.));
#64166=CARTESIAN_POINT('Origin',(23.5,0.,0.));
#64167=CARTESIAN_POINT('',(-11.8,17.5,0.));
#64168=CARTESIAN_POINT('',(-11.8,9.5,0.));
#64169=CARTESIAN_POINT('',(-10.5,18.8,0.));
#64170=CARTESIAN_POINT('Origin',(-10.5,17.5,0.));
#64171=CARTESIAN_POINT('',(57.5,18.8,0.));
#64172=CARTESIAN_POINT('',(41.25,18.8,0.));
#64173=CARTESIAN_POINT('',(58.8,17.5,0.));
#64174=CARTESIAN_POINT('Origin',(57.5,17.5,0.));
#64175=CARTESIAN_POINT('',(58.8,-17.5,0.));
#64176=CARTESIAN_POINT('',(58.8,-9.5,0.));
#64177=CARTESIAN_POINT('',(57.5,-18.8,0.));
#64178=CARTESIAN_POINT('Origin',(57.5,-17.5,0.));
#64179=CARTESIAN_POINT('',(-10.5,-18.8,0.));
#64180=CARTESIAN_POINT('',(5.75,-18.8,0.));
#64181=CARTESIAN_POINT('Origin',(-10.5,-17.5,0.));
#64182=CARTESIAN_POINT('',(-9.4,-15.,0.));
#64183=CARTESIAN_POINT('Origin',(-8.,-15.,0.));
#64184=CARTESIAN_POINT('',(52.6,-15.,0.));
#64185=CARTESIAN_POINT('Origin',(54.,-15.,0.));
#64186=CARTESIAN_POINT('',(52.6,15.,0.));
#64187=CARTESIAN_POINT('Origin',(54.,15.,0.));
#64188=CARTESIAN_POINT('',(-9.4,15.,0.));
#64189=CARTESIAN_POINT('Origin',(-8.,15.,0.));
#64190=CARTESIAN_POINT('Origin',(21.,0.,5.));
#64191=CARTESIAN_POINT('',(-6.,11.,5.));
#64192=CARTESIAN_POINT('',(-6.,11.,5.));
#64193=CARTESIAN_POINT('',(48.,11.,5.));
#64194=CARTESIAN_POINT('',(48.,11.,5.));
#64195=CARTESIAN_POINT('',(48.,-11.,5.));
#64196=CARTESIAN_POINT('',(48.,-11.,5.));
#64197=CARTESIAN_POINT('',(-6.,-11.,5.));
#64198=CARTESIAN_POINT('',(-6.,-11.,5.));
#64199=CARTESIAN_POINT('',(-6.,11.,5.));
#64200=CARTESIAN_POINT('',(5.2,-2.81668763803891E-16,5.));
#64201=CARTESIAN_POINT('Origin',(7.5,0.,5.));
#64202=CARTESIAN_POINT('Origin',(-6.,11.,0.));
#64203=CARTESIAN_POINT('',(-6.,11.,0.));
#64204=CARTESIAN_POINT('Origin',(48.,11.,0.));
#64205=CARTESIAN_POINT('',(48.,11.,0.));
#64206=CARTESIAN_POINT('Origin',(-8.,-15.,10.2));
#64207=CARTESIAN_POINT('',(-9.1,-15.,10.2));
#64208=CARTESIAN_POINT('Origin',(-8.,-15.,10.2));
#64209=CARTESIAN_POINT('',(-9.4,-15.,10.5));
#64210=CARTESIAN_POINT('Origin',(-9.4,-15.,10.2));
#64211=CARTESIAN_POINT('Origin',(-8.,-15.,10.5));
#64212=CARTESIAN_POINT('Origin',(-8.,-15.,5.235));
#64213=CARTESIAN_POINT('',(-9.1,-15.,0.3));
#64214=CARTESIAN_POINT('Origin',(-8.,-15.,0.3));
#64215=CARTESIAN_POINT('',(-9.1,-15.,5.235));
#64216=CARTESIAN_POINT('Origin',(-5.75,-15.,10.5));
#64217=CARTESIAN_POINT('',(-10.25,-15.,10.5));
#64218=CARTESIAN_POINT('Origin',(-8.,-15.,10.5));
#64219=CARTESIAN_POINT('Origin',(-8.,-15.,0.3));
#64220=CARTESIAN_POINT('Origin',(-9.4,-15.,0.3));
#64221=CARTESIAN_POINT('Origin',(-8.,15.,10.2));
#64222=CARTESIAN_POINT('',(-9.1,15.,10.2));
#64223=CARTESIAN_POINT('Origin',(-8.,15.,10.2));
#64224=CARTESIAN_POINT('',(-9.4,15.,10.5));
#64225=CARTESIAN_POINT('Origin',(-9.4,15.,10.2));
#64226=CARTESIAN_POINT('Origin',(-8.,15.,10.5));
#64227=CARTESIAN_POINT('Origin',(-8.,15.,5.235));
#64228=CARTESIAN_POINT('',(-9.1,15.,0.3));
#64229=CARTESIAN_POINT('Origin',(-8.,15.,0.3));
#64230=CARTESIAN_POINT('',(-9.1,15.,5.235));
#64231=CARTESIAN_POINT('Origin',(-5.75,15.,10.5));
#64232=CARTESIAN_POINT('',(-10.25,15.,10.5));
#64233=CARTESIAN_POINT('Origin',(-8.,15.,10.5));
#64234=CARTESIAN_POINT('Origin',(-8.,15.,0.3));
#64235=CARTESIAN_POINT('Origin',(-9.4,15.,0.3));
#64236=CARTESIAN_POINT('Origin',(54.,-15.,0.3));
#64237=CARTESIAN_POINT('',(52.9,-15.,0.3));
#64238=CARTESIAN_POINT('Origin',(52.6,-15.,0.3));
#64239=CARTESIAN_POINT('Origin',(54.,-15.,0.3));
#64240=CARTESIAN_POINT('Origin',(54.,-15.,5.235));
#64241=CARTESIAN_POINT('',(52.9,-15.,10.5));
#64242=CARTESIAN_POINT('',(52.9,-15.,5.235));
#64243=CARTESIAN_POINT('Origin',(54.,-15.,10.5));
#64244=CARTESIAN_POINT('Origin',(54.,15.,0.3));
#64245=CARTESIAN_POINT('',(52.9,15.,0.3));
#64246=CARTESIAN_POINT('Origin',(52.6,15.,0.3));
#64247=CARTESIAN_POINT('Origin',(54.,15.,0.3));
#64248=CARTESIAN_POINT('Origin',(54.,15.,5.235));
#64249=CARTESIAN_POINT('',(52.9,15.,10.5));
#64250=CARTESIAN_POINT('',(52.9,15.,5.235));
#64251=CARTESIAN_POINT('Origin',(54.,15.,10.5));
#64252=CARTESIAN_POINT('Origin',(25.3,11.7,15.8789502076511));
#64253=CARTESIAN_POINT('',(25.,11.7,15.8789502076511));
#64254=CARTESIAN_POINT('',(25.3,12.,15.8789502076511));
#64255=CARTESIAN_POINT('Origin',(25.3,11.7,15.8789502076511));
#64256=CARTESIAN_POINT('',(25.0836013169029,11.7,16.0867279974984));
#64257=CARTESIAN_POINT('Origin',(25.3,11.7,15.8789502076511));
#64258=CARTESIAN_POINT('Origin',(25.3,11.7,15.8789502076511));
#64259=CARTESIAN_POINT('Origin',(25.3,-11.7,15.8789502076511));
#64260=CARTESIAN_POINT('',(25.0836013169029,-11.7,16.0867279974984));
#64261=CARTESIAN_POINT('',(25.3,-12.,15.8789502076511));
#64262=CARTESIAN_POINT('Origin',(25.3,-11.7,15.8789502076511));
#64263=CARTESIAN_POINT('',(25.,-11.7,15.8789502076511));
#64264=CARTESIAN_POINT('Origin',(25.3,-11.7,15.8789502076511));
#64265=CARTESIAN_POINT('Origin',(25.3,-11.7,15.8789502076511));
#64266=CARTESIAN_POINT('Origin',(25.3,0.,15.8789502076511));
#64267=CARTESIAN_POINT('',(25.,0.,15.8789502076511));
#64268=CARTESIAN_POINT('',(25.0836013169029,0.,16.0867279974984));
#64269=CARTESIAN_POINT('Origin',(25.3,-11.7,15.1654284885127));
#64270=CARTESIAN_POINT('',(25.,-11.7,11.0627460668062));
#64271=CARTESIAN_POINT('',(25.3,-12.,11.1063316512536));
#64272=CARTESIAN_POINT('Ctrl Pts',(25.3,-12.,11.1063316512536));
#64273=CARTESIAN_POINT('Ctrl Pts',(25.2623920424744,-12.,11.1001380359884));
#64274=CARTESIAN_POINT('Ctrl Pts',(25.2221896898711,-11.9924955895806,11.0938216843788));
#64275=CARTESIAN_POINT('Ctrl Pts',(25.1480978181083,-11.9617896898647,11.0827230314705));
#64276=CARTESIAN_POINT('Ctrl Pts',(25.114212401788,-11.9385837288878,11.0779257180335));
#64277=CARTESIAN_POINT('Ctrl Pts',(25.0610047777006,-11.8851612194794,11.0706254416663));
#64278=CARTESIAN_POINT('Ctrl Pts',(25.0380212421969,-11.8515254269881,11.0676139543331));
#64279=CARTESIAN_POINT('Ctrl Pts',(25.0075180393908,-11.7777632812766,11.0636819697985));
#64280=CARTESIAN_POINT('Ctrl Pts',(25.,-11.7376370768973,11.0627460668062));
#64281=CARTESIAN_POINT('Ctrl Pts',(25.,-11.7,11.0627460668062));
#64282=CARTESIAN_POINT('',(25.3,-12.,15.1654284885127));
#64283=CARTESIAN_POINT('',(25.,-11.7,15.1654284885127));
#64284=CARTESIAN_POINT('Origin',(2.98958333333334,-11.7,37.3005642361111));
#64285=CARTESIAN_POINT('',(32.,-12.,26.5750822305795));
#64286=CARTESIAN_POINT('',(32.,-11.7,27.4736520332184));
#64287=CARTESIAN_POINT('Ctrl Pts',(32.,-12.,26.5750822305795));
#64288=CARTESIAN_POINT('Ctrl Pts',(32.,-12.,26.6950140675156));
#64289=CARTESIAN_POINT('Ctrl Pts',(32.,-11.9912295487024,26.8263190451688));
#64290=CARTESIAN_POINT('Ctrl Pts',(32.,-11.9602181513312,27.0190335202355));
#64291=CARTESIAN_POINT('Ctrl Pts',(32.,-11.9469632164437,27.0825245437305));
#64292=CARTESIAN_POINT('Ctrl Pts',(32.,-11.9132295457478,27.2045478171391));
#64293=CARTESIAN_POINT('Ctrl Pts',(32.,-11.8929743256761,27.2631417484441));
#64294=CARTESIAN_POINT('Ctrl Pts',(32.,-11.8446924251946,27.3623327659357));
#64295=CARTESIAN_POINT('Ctrl Pts',(32.,-11.8132217751365,27.4139121820562));
#64296=CARTESIAN_POINT('Ctrl Pts',(32.,-11.7626708395818,27.4537183942209));
#64297=CARTESIAN_POINT('Ctrl Pts',(32.,-11.748290736922,27.4623826653623));
#64298=CARTESIAN_POINT('Ctrl Pts',(32.,-11.7245725726024,27.471101807326));
#64299=CARTESIAN_POINT('Ctrl Pts',(32.,-11.7112795402592,27.4736520332184));
#64300=CARTESIAN_POINT('Ctrl Pts',(32.,-11.7,27.4736520332184));
#64301=CARTESIAN_POINT('Origin',(2.98958333333334,-11.7,37.3005642361111));
#64302=CARTESIAN_POINT('Origin',(2.98958333333334,-12.,37.3005642361111));
#64303=CARTESIAN_POINT('Origin',(2.98958333333334,11.7,37.3005642361111));
#64304=CARTESIAN_POINT('',(32.,11.7,27.4736520332184));
#64305=CARTESIAN_POINT('',(32.,12.,26.5750822305795));
#64306=CARTESIAN_POINT('Ctrl Pts',(32.,11.7,27.4736520332184));
#64307=CARTESIAN_POINT('Ctrl Pts',(32.,11.7112795402592,27.4736520332184));
#64308=CARTESIAN_POINT('Ctrl Pts',(32.,11.7245725726024,27.471101807326));
#64309=CARTESIAN_POINT('Ctrl Pts',(32.,11.748290736922,27.4623826653623));
#64310=CARTESIAN_POINT('Ctrl Pts',(32.,11.7626708395818,27.4537183942209));
#64311=CARTESIAN_POINT('Ctrl Pts',(32.,11.8132217751365,27.4139121820562));
#64312=CARTESIAN_POINT('Ctrl Pts',(32.,11.8446924251946,27.3623327659357));
#64313=CARTESIAN_POINT('Ctrl Pts',(32.,11.8929743256761,27.2631417484441));
#64314=CARTESIAN_POINT('Ctrl Pts',(32.,11.9132295457478,27.2045478171391));
#64315=CARTESIAN_POINT('Ctrl Pts',(32.,11.9469632164437,27.0825245437305));
#64316=CARTESIAN_POINT('Ctrl Pts',(32.,11.9602181513312,27.0190335202355));
#64317=CARTESIAN_POINT('Ctrl Pts',(32.,11.9912295487024,26.8263190451688));
#64318=CARTESIAN_POINT('Ctrl Pts',(32.,12.,26.6950140675156));
#64319=CARTESIAN_POINT('Ctrl Pts',(32.,12.,26.5750822305795));
#64320=CARTESIAN_POINT('Origin',(2.98958333333334,12.,37.3005642361111));
#64321=CARTESIAN_POINT('Origin',(2.98958333333334,11.7,37.3005642361111));
#64322=CARTESIAN_POINT('Origin',(25.3,11.7,15.1654284885127));
#64323=CARTESIAN_POINT('',(25.3,12.,11.1063316512536));
#64324=CARTESIAN_POINT('',(25.,11.7,11.0627460668062));
#64325=CARTESIAN_POINT('Ctrl Pts',(25.,11.7,11.0627460668062));
#64326=CARTESIAN_POINT('Ctrl Pts',(25.,11.7376370768973,11.0627460668062));
#64327=CARTESIAN_POINT('Ctrl Pts',(25.0075180393908,11.7777632812766,11.0636819697985));
#64328=CARTESIAN_POINT('Ctrl Pts',(25.0380212421969,11.8515254269881,11.0676139543331));
#64329=CARTESIAN_POINT('Ctrl Pts',(25.0610047777006,11.8851612194794,11.0706254416663));
#64330=CARTESIAN_POINT('Ctrl Pts',(25.114212401788,11.9385837288878,11.0779257180335));
#64331=CARTESIAN_POINT('Ctrl Pts',(25.1480978181083,11.9617896898647,11.0827230314705));
#64332=CARTESIAN_POINT('Ctrl Pts',(25.2221896898711,11.9924955895806,11.0938216843788));
#64333=CARTESIAN_POINT('Ctrl Pts',(25.2623920424744,12.,11.1001380359884));
#64334=CARTESIAN_POINT('Ctrl Pts',(25.3,12.,11.1063316512536));
#64335=CARTESIAN_POINT('',(25.,11.7,15.1654284885127));
#64336=CARTESIAN_POINT('',(25.3,12.,15.1654284885127));
#64337=CARTESIAN_POINT('Origin',(28.5000000077377,-12.,19.2681696700813));
#64338=CARTESIAN_POINT('',(26.1702534414211,-12.,11.3));
#64339=CARTESIAN_POINT('Origin',(24.,-12.,19.));
#64340=CARTESIAN_POINT('',(26.1706823007161,-12.,11.3));
#64341=CARTESIAN_POINT('',(26.1875000038689,-12.,11.3));
#64342=CARTESIAN_POINT('',(32.,-12.,19.));
#64343=CARTESIAN_POINT('Origin',(24.0004975859988,-12.,18.9995024140012));
#64344=CARTESIAN_POINT('',(32.,-12.,19.));
#64345=CARTESIAN_POINT('Origin',(25.,0.,11.0626873069442));
#64346=CARTESIAN_POINT('',(25.,-12.025,11.0627460668062));
#64347=CARTESIAN_POINT('',(25.,0.,11.0627460668062));
#64348=CARTESIAN_POINT('',(25.,12.025,11.0627460668062));
#64349=CARTESIAN_POINT('',(25.,0.,11.0627460668062));
#64350=CARTESIAN_POINT('',(25.,12.025,11.));
#64351=CARTESIAN_POINT('',(25.,12.025,11.));
#64352=CARTESIAN_POINT('',(25.,-12.025,11.));
#64353=CARTESIAN_POINT('',(25.,0.,11.));
#64354=CARTESIAN_POINT('',(25.,-12.025,11.));
#64355=CARTESIAN_POINT('Origin',(7.25,12.3,89.3));
#64356=CARTESIAN_POINT('',(-8.49857139617605,12.6,89.3));
#64357=CARTESIAN_POINT('',(-8.5,12.3,89.));
#64358=CARTESIAN_POINT('Ctrl Pts',(-8.49857139617605,12.6,89.3));
#64359=CARTESIAN_POINT('Ctrl Pts',(-8.49893015222796,12.6,89.2623323229503));
#64360=CARTESIAN_POINT('Ctrl Pts',(-8.4992383058263,12.592472261564,89.2221531517712));
#64361=CARTESIAN_POINT('Ctrl Pts',(-8.49967287208156,12.5618564029082,89.1482390701713));
#64362=CARTESIAN_POINT('Ctrl Pts',(-8.49980314675217,12.5387682604362,89.1145041917242));
#64363=CARTESIAN_POINT('Ctrl Pts',(-8.49995174729688,12.4854962982069,89.061232229495));
#64364=CARTESIAN_POINT('Ctrl Pts',(-8.49998062468412,12.4517619778622,89.0381442166394));
#64365=CARTESIAN_POINT('Ctrl Pts',(-8.50000282006993,12.37784817429,89.0075281022651));
#64366=CARTESIAN_POINT('Ctrl Pts',(-8.5,12.3376686925819,89.));
#64367=CARTESIAN_POINT('Ctrl Pts',(-8.5,12.3,89.));
#64368=CARTESIAN_POINT('',(-9.69862382425291,12.3,89.));
#64369=CARTESIAN_POINT('',(7.25,12.3,89.));
#64370=CARTESIAN_POINT('',(-9.69862382425291,12.6,89.3));
#64371=CARTESIAN_POINT('Origin',(-9.69862382425291,12.3,89.3));
#64372=CARTESIAN_POINT('',(7.25,12.6,89.3));
#64373=CARTESIAN_POINT('Origin',(-9.69862382425291,0.,89.3));
#64374=CARTESIAN_POINT('',(-9.69862382425291,11.8685749135175,88.999999999999));
#64375=CARTESIAN_POINT('',(-9.86042062850469,11.7000210181992,89.0473702429758));
#64376=CARTESIAN_POINT('Ctrl Pts',(-9.86042062850418,11.7000210181987,89.0473702429758));
#64377=CARTESIAN_POINT('Ctrl Pts',(-9.83339601165222,11.7306347273028,89.030062318944));
#64378=CARTESIAN_POINT('Ctrl Pts',(-9.80439864031728,11.7618204016055,89.0177472843307));
#64379=CARTESIAN_POINT('Ctrl Pts',(-9.75206287401563,11.8159965452229,89.0037464949648));
#64380=CARTESIAN_POINT('Ctrl Pts',(-9.72575618919431,11.8423829851573,89.));
#64381=CARTESIAN_POINT('Ctrl Pts',(-9.69862382425277,11.8685749135171,89.));
#64382=CARTESIAN_POINT('',(-9.86042062850543,12.,89.0473702429767));
#64383=CARTESIAN_POINT('',(-9.86042062850543,0.,89.0473702429767));
#64384=CARTESIAN_POINT('',(-9.99861119878734,12.,89.302752293578));
#64385=CARTESIAN_POINT('Origin',(-9.69862382425291,12.,89.3));
#64386=CARTESIAN_POINT('',(-9.99861119878734,12.3,89.302752293578));
#64387=CARTESIAN_POINT('',(-9.99861119878734,0.,89.302752293578));
#64388=CARTESIAN_POINT('Origin',(-9.69862382425291,12.3,89.3));
#64389=CARTESIAN_POINT('',(-9.69862382425291,0.,89.));
#64390=CARTESIAN_POINT('Origin',(-9.69862382425291,12.3,89.3));
#64391=CARTESIAN_POINT('Origin',(-9.69862382425291,12.3,89.3));
#64392=CARTESIAN_POINT('Origin',(23.,12.,89.));
#64393=CARTESIAN_POINT('',(54.5,12.6,89.));
#64394=CARTESIAN_POINT('Origin',(23.,12.6,89.));
#64395=CARTESIAN_POINT('',(54.5,12.,89.));
#64396=CARTESIAN_POINT('',(54.5,12.,89.));
#64397=CARTESIAN_POINT('',(44.873285764796,12.,111.667363539935));
#64398=CARTESIAN_POINT('Origin',(23.,12.,89.));
#64399=CARTESIAN_POINT('',(44.5360362332209,11.7,111.988021736578));
#64400=CARTESIAN_POINT('Ctrl Pts',(44.5360362332209,11.7,111.988021736578));
#64401=CARTESIAN_POINT('Ctrl Pts',(44.6032500460304,11.7599031326984,111.925053329613));
#64402=CARTESIAN_POINT('Ctrl Pts',(44.6704247023372,11.8197125550768,111.861567377855));
#64403=CARTESIAN_POINT('Ctrl Pts',(44.7828052847954,11.9196471425502,111.754413327953));
#64404=CARTESIAN_POINT('Ctrl Pts',(44.8281067726021,11.9598974683211,111.710959832247));
#64405=CARTESIAN_POINT('Ctrl Pts',(44.8732857647959,12.,111.667363539935));
#64406=CARTESIAN_POINT('',(44.5360362332209,12.,111.988021736578));
#64407=CARTESIAN_POINT('',(44.5360362332209,12.,111.988021736578));
#64408=CARTESIAN_POINT('',(-8.4243682746133,12.,91.1815312377953));
#64409=CARTESIAN_POINT('Origin',(23.,12.,89.));
#64410=CARTESIAN_POINT('',(-8.42436827451122,11.7000371816704,91.1815312379487));
#64411=CARTESIAN_POINT('',(-8.42436827461331,12.,91.1815312377953));
#64412=CARTESIAN_POINT('',(-8.45008814603704,12.,90.7725562350742));
#64413=CARTESIAN_POINT('Ctrl Pts',(-8.45008814603704,12.,90.7725562350742));
#64414=CARTESIAN_POINT('Ctrl Pts',(-8.44952770606724,11.9929198577654,90.782500002218));
#64415=CARTESIAN_POINT('Ctrl Pts',(-8.44896290115791,11.9858275744744,90.792437287118));
#64416=CARTESIAN_POINT('Ctrl Pts',(-8.44108102807065,11.8874474044361,90.9299630010769));
#64417=CARTESIAN_POINT('Ctrl Pts',(-8.4330514997603,11.7942613180871,91.0564517247953));
#64418=CARTESIAN_POINT('Ctrl Pts',(-8.42436827460622,11.7000371815935,91.1815312378974));
#64419=CARTESIAN_POINT('',(-8.5,12.,89.));
#64420=CARTESIAN_POINT('Origin',(23.,12.,89.));
#64421=CARTESIAN_POINT('',(-8.5,12.,89.));
#64422=CARTESIAN_POINT('Origin',(23.,12.6,67.75));
#64423=CARTESIAN_POINT('',(55.7,12.6,89.));
#64424=CARTESIAN_POINT('Origin',(23.,12.6,89.));
#64425=CARTESIAN_POINT('',(55.7,12.6,13.5));
#64426=CARTESIAN_POINT('',(55.7,12.6,83.875));
#64427=CARTESIAN_POINT('',(54.5,12.6,13.5));
#64428=CARTESIAN_POINT('',(56.,12.6,13.5));
#64429=CARTESIAN_POINT('',(54.5,12.6,13.5));
#64430=CARTESIAN_POINT('Origin',(23.,12.3,89.));
#64431=CARTESIAN_POINT('',(56.,12.3,89.));
#64432=CARTESIAN_POINT('Origin',(23.,12.3,89.));
#64433=CARTESIAN_POINT('Origin',(55.7,12.3,89.));
#64434=CARTESIAN_POINT('Origin',(23.,0.,89.));
#64435=CARTESIAN_POINT('',(-10.,12.,89.));
#64436=CARTESIAN_POINT('Origin',(23.,12.,89.));
#64437=CARTESIAN_POINT('',(-10.,-12.,89.));
#64438=CARTESIAN_POINT('',(-10.,0.,89.));
#64439=CARTESIAN_POINT('',(-9.99861119878734,-12.,89.302752293578));
#64440=CARTESIAN_POINT('Origin',(23.,-12.,89.));
#64441=CARTESIAN_POINT('',(-9.99861119878734,-12.3,89.302752293578));
#64442=CARTESIAN_POINT('',(-9.99861119878734,0.,89.302752293578));
#64443=CARTESIAN_POINT('',(56.,-12.3,89.));
#64444=CARTESIAN_POINT('Origin',(23.,-12.3,89.));
#64445=CARTESIAN_POINT('',(56.,0.,89.));
#64446=CARTESIAN_POINT('',(-6.6697247706422,-4.82,103.446710076496));
#64447=CARTESIAN_POINT('',(4.65321100917432,-4.82,116.429825623327));
#64448=CARTESIAN_POINT('Origin',(23.,-4.82,89.));
#64449=CARTESIAN_POINT('',(-6.6697247706422,4.82,103.446710076496));
#64450=CARTESIAN_POINT('',(-6.6697247706422,0.,103.446710076496));
#64451=CARTESIAN_POINT('',(4.65321100917432,4.82,116.429825623327));
#64452=CARTESIAN_POINT('Origin',(23.,4.82,89.));
#64453=CARTESIAN_POINT('',(4.65321100917432,0.,116.429825623327));
#64454=CARTESIAN_POINT('Origin',(-9.69862382425291,0.,89.3));
#64455=CARTESIAN_POINT('',(-9.69862382425291,-11.8685749135175,88.999999999999));
#64456=CARTESIAN_POINT('',(-9.86042062850469,-11.7000210181992,89.0473702429758));
#64457=CARTESIAN_POINT('Ctrl Pts',(-9.69862382425277,-11.8685749135171,
89.));
#64458=CARTESIAN_POINT('Ctrl Pts',(-9.72575618919431,-11.8423829851573,
89.));
#64459=CARTESIAN_POINT('Ctrl Pts',(-9.75206287401563,-11.8159965452229,
89.0037464949648));
#64460=CARTESIAN_POINT('Ctrl Pts',(-9.80439864031728,-11.7618204016055,
89.0177472843307));
#64461=CARTESIAN_POINT('Ctrl Pts',(-9.83339601165223,-11.7306347273028,
89.030062318944));
#64462=CARTESIAN_POINT('Ctrl Pts',(-9.86042062850418,-11.7000210181987,
89.0473702429759));
#64463=CARTESIAN_POINT('',(-9.69862382425291,-12.3,89.));
#64464=CARTESIAN_POINT('',(-9.69862382425291,0.,89.));
#64465=CARTESIAN_POINT('Origin',(-9.69862382425291,-12.3,89.3));
#64466=CARTESIAN_POINT('',(-9.86042062850543,-12.,89.0473702429767));
#64467=CARTESIAN_POINT('Origin',(-9.69862382425291,-12.,89.3));
#64468=CARTESIAN_POINT('',(-9.86042062850543,0.,89.0473702429767));
#64469=CARTESIAN_POINT('Origin',(7.25,-12.3,89.3));
#64470=CARTESIAN_POINT('',(-8.5,-12.3,89.));
#64471=CARTESIAN_POINT('',(-8.49857139617605,-12.6,89.3));
#64472=CARTESIAN_POINT('Ctrl Pts',(-8.5,-12.3,89.));
#64473=CARTESIAN_POINT('Ctrl Pts',(-8.5,-12.3376686925819,89.));
#64474=CARTESIAN_POINT('Ctrl Pts',(-8.50000282006993,-12.37784817429,89.0075281022651));
#64475=CARTESIAN_POINT('Ctrl Pts',(-8.49998062468412,-12.4517619778622,
89.0381442166394));
#64476=CARTESIAN_POINT('Ctrl Pts',(-8.49995174729688,-12.4854962982069,
89.061232229495));
#64477=CARTESIAN_POINT('Ctrl Pts',(-8.49980314675217,-12.5387682604362,
89.1145041917242));
#64478=CARTESIAN_POINT('Ctrl Pts',(-8.49967287208156,-12.5618564029082,
89.1482390701713));
#64479=CARTESIAN_POINT('Ctrl Pts',(-8.4992383058263,-12.592472261564,89.2221531517712));
#64480=CARTESIAN_POINT('Ctrl Pts',(-8.49893015222796,-12.6,89.2623323229503));
#64481=CARTESIAN_POINT('Ctrl Pts',(-8.49857139617605,-12.6,89.3));
#64482=CARTESIAN_POINT('',(-9.69862382425291,-12.6,89.3));
#64483=CARTESIAN_POINT('',(7.25,-12.6,89.3));
#64484=CARTESIAN_POINT('Origin',(-9.69862382425291,-12.3,89.3));
#64485=CARTESIAN_POINT('',(7.25,-12.3,89.));
#64486=CARTESIAN_POINT('Origin',(-9.69862382425291,-12.3,89.3));
#64487=CARTESIAN_POINT('Origin',(-9.69862382425291,-12.3,89.3));
#64488=CARTESIAN_POINT('Origin',(23.,-12.3,89.));
#64489=CARTESIAN_POINT('',(55.7,-12.6,89.));
#64490=CARTESIAN_POINT('Origin',(23.,-12.6,89.));
#64491=CARTESIAN_POINT('Origin',(55.7,-12.3,89.));
#64492=CARTESIAN_POINT('Origin',(23.,-12.6,67.75));
#64493=CARTESIAN_POINT('',(54.5,-12.6,89.));
#64494=CARTESIAN_POINT('Origin',(23.,-12.6,89.));
#64495=CARTESIAN_POINT('',(54.5,-12.6,13.5));
#64496=CARTESIAN_POINT('',(54.5,-12.6,13.5));
#64497=CARTESIAN_POINT('',(55.7,-12.6,13.5));
#64498=CARTESIAN_POINT('',(56.,-12.6,13.5));
#64499=CARTESIAN_POINT('',(55.7,-12.6,83.875));
#64500=CARTESIAN_POINT('Origin',(23.,-12.,89.));
#64501=CARTESIAN_POINT('',(-8.5,-12.,89.));
#64502=CARTESIAN_POINT('',(-8.5,-12.,89.));
#64503=CARTESIAN_POINT('',(-8.45008814603704,-12.,90.7725562350742));
#64504=CARTESIAN_POINT('Origin',(23.,-12.,89.));
#64505=CARTESIAN_POINT('',(-8.4243682745111,-11.7000371816705,91.1815312379489));
#64506=CARTESIAN_POINT('Ctrl Pts',(-8.42436827460621,-11.7000371815934,
91.1815312378975));
#64507=CARTESIAN_POINT('Ctrl Pts',(-8.43305149973544,-11.7942613178173,
91.0564517251533));
#64508=CARTESIAN_POINT('Ctrl Pts',(-8.44108102802452,-11.8874474039008,
90.9299630018033));
#64509=CARTESIAN_POINT('Ctrl Pts',(-8.44896290111612,-11.9858275739497,
90.7924372878531));
#64510=CARTESIAN_POINT('Ctrl Pts',(-8.44952770604651,-11.9929198575035,
90.7825000025858));
#64511=CARTESIAN_POINT('Ctrl Pts',(-8.45008814603704,-12.,90.7725562350742));
#64512=CARTESIAN_POINT('',(-8.4243682746133,-12.,91.1815312377953));
#64513=CARTESIAN_POINT('',(-8.42436827461331,-12.,91.1815312377953));
#64514=CARTESIAN_POINT('',(44.5360362332209,-12.,111.988021736578));
#64515=CARTESIAN_POINT('Origin',(23.,-12.,89.));
#64516=CARTESIAN_POINT('',(44.5360362332209,-11.7,111.988021736578));
#64517=CARTESIAN_POINT('',(44.5360362332209,-12.,111.988021736578));
#64518=CARTESIAN_POINT('',(44.873285764796,-12.,111.667363539935));
#64519=CARTESIAN_POINT('Ctrl Pts',(44.873285764796,-12.,111.667363539935));
#64520=CARTESIAN_POINT('Ctrl Pts',(44.8281067726021,-11.9598974683211,111.710959832247));
#64521=CARTESIAN_POINT('Ctrl Pts',(44.7828052847954,-11.9196471425502,111.754413327953));
#64522=CARTESIAN_POINT('Ctrl Pts',(44.6704247023372,-11.8197125550768,111.861567377855));
#64523=CARTESIAN_POINT('Ctrl Pts',(44.6032500460304,-11.7599031326984,111.925053329613));
#64524=CARTESIAN_POINT('Ctrl Pts',(44.5360362332209,-11.7,111.988021736578));
#64525=CARTESIAN_POINT('',(54.5,-12.,89.));
#64526=CARTESIAN_POINT('Origin',(23.,-12.,89.));
#64527=CARTESIAN_POINT('',(54.5,-12.,89.));
#64528=CARTESIAN_POINT('Origin',(4.82,0.,116.180463572206));
#64529=CARTESIAN_POINT('',(4.52,4.57127326170559,116.180463572206));
#64530=CARTESIAN_POINT('Ctrl Pts',(4.52,4.57127326170559,116.180463572206));
#64531=CARTESIAN_POINT('Ctrl Pts',(4.52,4.59032279673937,116.214621871278));
#64532=CARTESIAN_POINT('Ctrl Pts',(4.52581302559788,4.61305103487801,116.246803205237));
#64533=CARTESIAN_POINT('Ctrl Pts',(4.54680207258012,4.66516558526338,116.309299708264));
#64534=CARTESIAN_POINT('Ctrl Pts',(4.56333143461808,4.69541449500085,116.339164914641));
#64535=CARTESIAN_POINT('Ctrl Pts',(4.60315123270544,4.75667572971404,116.390247753154));
#64536=CARTESIAN_POINT('Ctrl Pts',(4.62660338914075,4.78808658725471,116.411941289625));
#64537=CARTESIAN_POINT('Ctrl Pts',(4.65282998347464,4.81954351280017,116.429570453179));
#64538=CARTESIAN_POINT('Ctrl Pts',(4.65302042328646,4.81977175643649,116.429698147523));
#64539=CARTESIAN_POINT('Ctrl Pts',(4.65321100917433,4.82,116.429825623327));
#64540=CARTESIAN_POINT('',(4.52,-4.57127326170559,116.180463572206));
#64541=CARTESIAN_POINT('',(4.52,0.,116.180463572206));
#64542=CARTESIAN_POINT('Ctrl Pts',(4.65321100917432,-4.82,116.429825623327));
#64543=CARTESIAN_POINT('Ctrl Pts',(4.65302042470636,-4.81977175813695,116.429698148473));
#64544=CARTESIAN_POINT('Ctrl Pts',(4.65282998631353,-4.81954351619801,116.429570455082));
#64545=CARTESIAN_POINT('Ctrl Pts',(4.62660209328677,-4.78808503348141,116.411940419215));
#64546=CARTESIAN_POINT('Ctrl Pts',(4.60314888688512,-4.75667258912483,116.390245585618));
#64547=CARTESIAN_POINT('Ctrl Pts',(4.56332857524287,-4.69540962032475,116.339160391622));
#64548=CARTESIAN_POINT('Ctrl Pts',(4.54679946880003,-4.66516046552692,116.309294367754));
#64549=CARTESIAN_POINT('Ctrl Pts',(4.52581220928109,-4.61304783029562,116.246798662654));
#64550=CARTESIAN_POINT('Ctrl Pts',(4.52,-4.59032144835482,116.214619453449));
#64551=CARTESIAN_POINT('Ctrl Pts',(4.52,-4.57127326170558,116.180463572206));
#64552=CARTESIAN_POINT('Origin',(4.52,-4.52,62.));
#64553=CARTESIAN_POINT('',(4.52,4.52,115.977390533556));
#64554=CARTESIAN_POINT('Ctrl Pts',(4.52,4.57127326170559,116.180463572206));
#64555=CARTESIAN_POINT('Ctrl Pts',(4.52,4.56121444363019,116.162426800414));
#64556=CARTESIAN_POINT('Ctrl Pts',(4.52,4.5527871400801,116.143675769804));
#64557=CARTESIAN_POINT('Ctrl Pts',(4.52,4.52968731714536,116.081272993969));
#64558=CARTESIAN_POINT('Ctrl Pts',(4.52,4.52,116.024985987463));
#64559=CARTESIAN_POINT('Ctrl Pts',(4.52,4.52,115.977390533556));
#64560=CARTESIAN_POINT('',(4.52,4.52,92.));
#64561=CARTESIAN_POINT('',(4.52,4.52,62.));
#64562=CARTESIAN_POINT('',(4.52,-4.52,92.));
#64563=CARTESIAN_POINT('',(4.52,-2.26,92.));
#64564=CARTESIAN_POINT('',(4.52,-4.52,115.977390533556));
#64565=CARTESIAN_POINT('',(4.52,-4.52,62.));
#64566=CARTESIAN_POINT('Ctrl Pts',(4.52,-4.52,115.977390533556));
#64567=CARTESIAN_POINT('Ctrl Pts',(4.52,-4.52,116.024985987463));
#64568=CARTESIAN_POINT('Ctrl Pts',(4.52,-4.52968731714536,116.081272993969));
#64569=CARTESIAN_POINT('Ctrl Pts',(4.52,-4.5527871400801,116.143675769804));
#64570=CARTESIAN_POINT('Ctrl Pts',(4.52,-4.56121444363017,116.162426800414));
#64571=CARTESIAN_POINT('Ctrl Pts',(4.52,-4.57127326170558,116.180463572206));
#64572=CARTESIAN_POINT('Origin',(-9.7,0.,87.));
#64573=CARTESIAN_POINT('',(-10.,-1.35323471305783E-16,88.105));
#64574=CARTESIAN_POINT('Origin',(-10.,0.,87.));
#64575=CARTESIAN_POINT('',(-9.7,-9.85840673313618E-17,87.805));
#64576=CARTESIAN_POINT('Origin',(-9.7,-1.35323471305782E-16,88.105));
#64577=CARTESIAN_POINT('',(-9.7,9.8584067331361E-17,86.195));
#64578=CARTESIAN_POINT('Origin',(-9.7,0.,87.));
#64579=CARTESIAN_POINT('Origin',(-9.7,0.,87.));
#64580=CARTESIAN_POINT('Origin',(-10.,0.,68.));
#64581=CARTESIAN_POINT('',(-9.99999999942964,-0.470126090455401,68.0000190309882));
#64582=CARTESIAN_POINT('',(-10.,-1.35323471305783E-16,70.105));
#64583=CARTESIAN_POINT('Origin',(-10.,0.,69.));
#64584=CARTESIAN_POINT('',(-10.,-11.7,68.));
#64585=CARTESIAN_POINT('',(-10.,0.,68.));
#64586=CARTESIAN_POINT('',(-10.,-11.7,88.));
#64587=CARTESIAN_POINT('',(-10.,-11.7,64.75));
#64588=CARTESIAN_POINT('',(-10.,-12.,88.));
#64589=CARTESIAN_POINT('',(-10.,0.,88.));
#64590=CARTESIAN_POINT('',(-10.,-12.,68.));
#64591=CARTESIAN_POINT('',(-10.,12.,88.));
#64592=CARTESIAN_POINT('',(-10.,12.,68.));
#64593=CARTESIAN_POINT('',(-10.,11.7,88.));
#64594=CARTESIAN_POINT('',(-10.,0.,88.));
#64595=CARTESIAN_POINT('',(-10.,11.7,68.));
#64596=CARTESIAN_POINT('',(-10.,11.7,64.75));
#64597=CARTESIAN_POINT('',(-9.99999999942964,0.4701260904554,68.0000190309882));
#64598=CARTESIAN_POINT('',(-10.,0.,68.));
#64599=CARTESIAN_POINT('Origin',(-10.,0.,69.));
#64600=CARTESIAN_POINT('',(-10.,-1.35323471305783E-16,83.105));
#64601=CARTESIAN_POINT('Origin',(-10.,0.,82.));
#64602=CARTESIAN_POINT('',(-10.,-1.35323471305783E-16,75.105));
#64603=CARTESIAN_POINT('Origin',(-10.,0.,74.));
#64604=CARTESIAN_POINT('Origin',(-8.05,0.,87.));
#64605=CARTESIAN_POINT('',(-6.4,-9.8584067331361E-17,86.195));
#64606=CARTESIAN_POINT('Origin',(-6.4,0.,87.));
#64607=CARTESIAN_POINT('',(-8.05,-9.8584067331361E-17,86.195));
#64608=CARTESIAN_POINT('Origin',(-9.7,0.,82.));
#64609=CARTESIAN_POINT('',(-9.7,-9.85840673313618E-17,82.805));
#64610=CARTESIAN_POINT('Origin',(-9.7,-1.35323471305782E-16,83.105));
#64611=CARTESIAN_POINT('',(-9.7,9.8584067331361E-17,81.195));
#64612=CARTESIAN_POINT('Origin',(-9.7,0.,82.));
#64613=CARTESIAN_POINT('Origin',(-9.7,0.,82.));
#64614=CARTESIAN_POINT('Origin',(-8.05,0.,82.));
#64615=CARTESIAN_POINT('',(-6.4,-9.8584067331361E-17,81.195));
#64616=CARTESIAN_POINT('Origin',(-6.4,0.,82.));
#64617=CARTESIAN_POINT('',(-8.05,-9.8584067331361E-17,81.195));
#64618=CARTESIAN_POINT('Origin',(-9.7,0.,74.));
#64619=CARTESIAN_POINT('',(-9.7,-9.85840673313618E-17,74.805));
#64620=CARTESIAN_POINT('Origin',(-9.7,-1.35323471305782E-16,75.105));
#64621=CARTESIAN_POINT('',(-9.7,9.8584067331361E-17,73.195));
#64622=CARTESIAN_POINT('Origin',(-9.7,0.,74.));
#64623=CARTESIAN_POINT('Origin',(-9.7,0.,74.));
#64624=CARTESIAN_POINT('Origin',(-8.05,0.,74.));
#64625=CARTESIAN_POINT('',(-6.4,-9.8584067331361E-17,73.195));
#64626=CARTESIAN_POINT('Origin',(-6.4,0.,74.));
#64627=CARTESIAN_POINT('',(-8.05,-9.8584067331361E-17,73.195));
#64628=CARTESIAN_POINT('Origin',(-9.7,0.,69.));
#64629=CARTESIAN_POINT('Ctrl Pts',(-9.99999999942964,0.470126090455401,
68.0000190309882));
#64630=CARTESIAN_POINT('Ctrl Pts',(-9.99999998813253,0.468118427919553,
67.9992943413484));
#64631=CARTESIAN_POINT('Ctrl Pts',(-9.99999980855369,0.466342204530572,
67.9986571434586));
#64632=CARTESIAN_POINT('Ctrl Pts',(-9.99996282245433,0.273581519871146,
67.9300626849876));
#64633=CARTESIAN_POINT('Ctrl Pts',(-9.99914891965457,0.112578315718402,
67.9175814939608));
#64634=CARTESIAN_POINT('Ctrl Pts',(-9.99914891965457,-0.112578315316757,
67.9175814939608));
#64635=CARTESIAN_POINT('Ctrl Pts',(-9.99996282245425,-0.273581519475881,
67.9300626848471));
#64636=CARTESIAN_POINT('Ctrl Pts',(-9.99999980855369,-0.466342204533258,
67.9986571434596));
#64637=CARTESIAN_POINT('Ctrl Pts',(-9.99999998813253,-0.468118427917354,
67.9992943413476));
#64638=CARTESIAN_POINT('Ctrl Pts',(-9.99999999942964,-0.47012609045541,
68.0000190309882));
#64639=CARTESIAN_POINT('',(-9.7,-9.85840673313618E-17,69.805));
#64640=CARTESIAN_POINT('Origin',(-9.7,-1.35323471305782E-16,70.105));
#64641=CARTESIAN_POINT('',(-9.7,9.8584067331361E-17,68.195));
#64642=CARTESIAN_POINT('Origin',(-9.7,0.,69.));
#64643=CARTESIAN_POINT('Origin',(-9.7,0.,69.));
#64644=CARTESIAN_POINT('Origin',(-5.9999073877354,0.,68.0000926122646));
#64645=CARTESIAN_POINT('',(-6.,11.7,64.));
#64646=CARTESIAN_POINT('Ctrl Pts',(-6.,11.7,64.));
#64647=CARTESIAN_POINT('Ctrl Pts',(-6.25112253076429,11.700005814122,64.0000058141219));
#64648=CARTESIAN_POINT('Ctrl Pts',(-6.51082246976745,11.700011270506,64.0240405917389));
#64649=CARTESIAN_POINT('Ctrl Pts',(-7.02743037635765,11.7000208877413,64.1252738553641));
#64650=CARTESIAN_POINT('Ctrl Pts',(-7.28434258369625,11.7000250491913,64.2024507041098));
#64651=CARTESIAN_POINT('Ctrl Pts',(-7.7770960960606,11.7000317321778,64.4065625747948));
#64652=CARTESIAN_POINT('Ctrl Pts',(-8.01332979059301,11.7000342590358,64.5336601351113));
#64653=CARTESIAN_POINT('Ctrl Pts',(-8.45020267146997,11.7000375733931,64.8273844766965));
#64654=CARTESIAN_POINT('Ctrl Pts',(-8.65082955549268,11.7000383601839,64.9940295554927));
#64655=CARTESIAN_POINT('Ctrl Pts',(-9.00597044450735,11.7000383601839,65.3491704445074));
#64656=CARTESIAN_POINT('Ctrl Pts',(-9.17261552330358,11.7000375733931,65.5497973285301));
#64657=CARTESIAN_POINT('Ctrl Pts',(-9.46633986488873,11.7000342590358,65.986670209407));
#64658=CARTESIAN_POINT('Ctrl Pts',(-9.59343742520522,11.7000317321777,66.2229039039394));
#64659=CARTESIAN_POINT('Ctrl Pts',(-9.79754929589018,11.7000250491913,66.7156574163038));
#64660=CARTESIAN_POINT('Ctrl Pts',(-9.87472614463586,11.7000208877412,66.9725696236423));
#64661=CARTESIAN_POINT('Ctrl Pts',(-9.97595940826116,11.700011270506,67.4891775302326));
#64662=CARTESIAN_POINT('Ctrl Pts',(-9.99999418587806,11.7000058141219,67.7488774692357));
#64663=CARTESIAN_POINT('Ctrl Pts',(-10.,11.7,68.));
#64664=CARTESIAN_POINT('',(-6.,4.72,64.));
#64665=CARTESIAN_POINT('',(-6.,0.,64.));
#64666=CARTESIAN_POINT('',(-6.43243912956307,4.69654632125481,64.0234536787452));
#64667=CARTESIAN_POINT('Origin',(-5.9999073877354,0.719907387735438,68.0000926122646));
#64668=CARTESIAN_POINT('',(-6.43243912956307,-4.69654632125481,64.0234536787452));
#64669=CARTESIAN_POINT('',(-6.43243912956307,0.,64.0234536787452));
#64670=CARTESIAN_POINT('',(-6.,-4.72,64.));
#64671=CARTESIAN_POINT('Origin',(-5.9999073877354,-0.719907387735438,68.0000926122646));
#64672=CARTESIAN_POINT('',(-6.,-11.7,64.));
#64673=CARTESIAN_POINT('',(-6.,0.,64.));
#64674=CARTESIAN_POINT('Ctrl Pts',(-10.,-11.7,68.));
#64675=CARTESIAN_POINT('Ctrl Pts',(-9.9999941870305,-11.7000058129695,67.7489272452332));
#64676=CARTESIAN_POINT('Ctrl Pts',(-9.97596913895641,-11.700011268298,67.4892826274773));
#64677=CARTESIAN_POINT('Ctrl Pts',(-9.87476627167497,-11.7000208852123,
66.9727189780775));
#64678=CARTESIAN_POINT('Ctrl Pts',(-9.79759683635832,-11.7000250470742,
66.7157963928911));
#64679=CARTESIAN_POINT('Ctrl Pts',(-9.59349620678922,-11.7000317308133,
66.2230216156946));
#64680=CARTESIAN_POINT('Ctrl Pts',(-9.46640247476706,-11.7000342580129,
65.9867769970987));
#64681=CARTESIAN_POINT('Ctrl Pts',(-9.17268217075586,-11.7000375729573,
65.5498827986129));
#64682=CARTESIAN_POINT('Ctrl Pts',(-9.00603729816346,-11.7000383599935,
65.3492455223435));
#64683=CARTESIAN_POINT('Ctrl Pts',(-8.65089367384098,-11.7000383603743,
64.9940854526933));
#64684=CARTESIAN_POINT('Ctrl Pts',(-8.45026411428748,-11.7000375737319,
64.8274312897584));
#64685=CARTESIAN_POINT('Ctrl Pts',(-8.01338351700647,-11.7000342595708,
64.53369075565));
#64686=CARTESIAN_POINT('Ctrl Pts',(-7.7771447837467,-11.7000317327607,64.4065860844428));
#64687=CARTESIAN_POINT('Ctrl Pts',(-7.28437945797041,-11.7000250497688,
64.2024626371268));
#64688=CARTESIAN_POINT('Ctrl Pts',(-7.02746044639484,-11.700020888265,64.1252813050771));
#64689=CARTESIAN_POINT('Ctrl Pts',(-6.5108379773071,-11.7000112708308,64.0240420734374));
#64690=CARTESIAN_POINT('Ctrl Pts',(-6.25113027928763,-11.7000058143014,
64.0000058143013));
#64691=CARTESIAN_POINT('Ctrl Pts',(-6.,-11.7,64.));
#64692=CARTESIAN_POINT('Origin',(-8.05,0.,69.));
#64693=CARTESIAN_POINT('',(-6.4,-9.8584067331361E-17,68.195));
#64694=CARTESIAN_POINT('Origin',(-6.4,0.,69.));
#64695=CARTESIAN_POINT('',(-8.05,-9.8584067331361E-17,68.195));
#64696=CARTESIAN_POINT('Origin',(-6.4,0.,103.315376348528));
#64697=CARTESIAN_POINT('',(-6.26743038421116,4.52,103.584495833088));
#64698=CARTESIAN_POINT('Ctrl Pts',(-6.6697247706422,4.82,103.446710076496));
#64699=CARTESIAN_POINT('Ctrl Pts',(-6.6696252575399,4.81977372209222,103.446914450111));
#64700=CARTESIAN_POINT('Ctrl Pts',(-6.6695255121209,4.81954744411124,103.447118710688));
#64701=CARTESIAN_POINT('Ctrl Pts',(-6.65517755554285,4.78707393638485,103.476416233538));
#64702=CARTESIAN_POINT('Ctrl Pts',(-6.63612325427058,4.75462574198187,103.503393613814));
#64703=CARTESIAN_POINT('Ctrl Pts',(-6.58988824959697,4.6928359313211,103.5498694845));
#64704=CARTESIAN_POINT('Ctrl Pts',(-6.56262383483166,4.66300885428511,103.56987026714));
#64705=CARTESIAN_POINT('Ctrl Pts',(-6.50176857960494,4.60981011685317,103.599492331102));
#64706=CARTESIAN_POINT('Ctrl Pts',(-6.46823886939747,4.58584069575979,103.609814075921));
#64707=CARTESIAN_POINT('Ctrl Pts',(-6.40390283804146,4.55140125451023,103.61665065922));
#64708=CARTESIAN_POINT('Ctrl Pts',(-6.37449937904038,4.5391620652867,103.615845514477));
#64709=CARTESIAN_POINT('Ctrl Pts',(-6.31820829087247,4.52382192841078,103.605248291869));
#64710=CARTESIAN_POINT('Ctrl Pts',(-6.29224369239987,4.52,103.596718993883));
#64711=CARTESIAN_POINT('Ctrl Pts',(-6.26743038421117,4.52,103.584495833088));
#64712=CARTESIAN_POINT('',(-6.26743038421116,-4.52,103.584495833088));
#64713=CARTESIAN_POINT('Ctrl Pts',(-6.26743038421116,-4.52,103.584495833088));
#64714=CARTESIAN_POINT('Ctrl Pts',(-6.2922436925302,-4.52,103.596718993948));
#64715=CARTESIAN_POINT('Ctrl Pts',(-6.31820829113994,-4.52382192845083,
103.605248291956));
#64716=CARTESIAN_POINT('Ctrl Pts',(-6.37449937946708,-4.53916206544046,
103.615845514515));
#64717=CARTESIAN_POINT('Ctrl Pts',(-6.40390283848748,-4.55140125471072,
103.616650659215));
#64718=CARTESIAN_POINT('Ctrl Pts',(-6.46823886988568,-4.58584069607141,
103.609814075813));
#64719=CARTESIAN_POINT('Ctrl Pts',(-6.50176858011075,-4.60981011723393,
103.599492330925));
#64720=CARTESIAN_POINT('Ctrl Pts',(-6.5626238352147,-4.6630088546851,103.56987026688));
#64721=CARTESIAN_POINT('Ctrl Pts',(-6.58988824987319,-4.69283593165289,
103.549869484264));
#64722=CARTESIAN_POINT('Ctrl Pts',(-6.63612325437506,-4.7546257421599,103.503393613666));
#64723=CARTESIAN_POINT('Ctrl Pts',(-6.65517755560667,-4.78707393641448,
103.476416233408));
#64724=CARTESIAN_POINT('Ctrl Pts',(-6.66952551212043,-4.81954744411345,
103.447118710689));
#64725=CARTESIAN_POINT('Ctrl Pts',(-6.66962525753937,-4.819773722091,103.446914450112));
#64726=CARTESIAN_POINT('Ctrl Pts',(-6.6697247706422,-4.82,103.446710076496));
#64727=CARTESIAN_POINT('',(-6.1,-4.52,103.315376348528));
#64728=CARTESIAN_POINT('Origin',(-6.4,-4.52,103.315376348528));
#64729=CARTESIAN_POINT('',(-6.1,4.52,103.315376348528));
#64730=CARTESIAN_POINT('',(-6.1,0.,103.315376348528));
#64731=CARTESIAN_POINT('Origin',(-6.4,4.52,103.315376348528));
#64732=CARTESIAN_POINT('Origin',(-6.1,4.52,62.));
#64733=CARTESIAN_POINT('',(-6.1,-4.52,91.9987475176032));
#64734=CARTESIAN_POINT('',(-6.1,-4.52,62.));
#64735=CARTESIAN_POINT('',(-6.1,-4.71874751760316,91.9987475176032));
#64736=CARTESIAN_POINT('',(-6.1,0.,91.9987475176032));
#64737=CARTESIAN_POINT('',(-6.1,-4.52,91.8));
#64738=CARTESIAN_POINT('',(-6.1,5.14000000000013,82.1400000000004));
#64739=CARTESIAN_POINT('',(-6.1,-4.52,64.3216946934853));
#64740=CARTESIAN_POINT('',(-6.1,-4.52,62.));
#64741=CARTESIAN_POINT('',(-6.1,0.,64.3216946934853));
#64742=CARTESIAN_POINT('',(-6.1,4.71874751760317,91.9987475176032));
#64743=CARTESIAN_POINT('',(-6.1,-2.88,84.4000000000004));
#64744=CARTESIAN_POINT('',(-6.1,4.52,91.9987475176032));
#64745=CARTESIAN_POINT('',(-6.1,0.,91.9987475176032));
#64746=CARTESIAN_POINT('',(-6.1,4.52,62.));
#64747=CARTESIAN_POINT('',(-6.1,1.35323471305782E-16,67.895));
#64748=CARTESIAN_POINT('Origin',(-6.1,0.,69.));
#64749=CARTESIAN_POINT('',(-6.1,1.35323471305782E-16,80.895));
#64750=CARTESIAN_POINT('Origin',(-6.1,0.,82.));
#64751=CARTESIAN_POINT('',(-6.1,1.35323471305782E-16,85.895));
#64752=CARTESIAN_POINT('Origin',(-6.1,0.,87.));
#64753=CARTESIAN_POINT('',(-6.1,1.35323471305782E-16,72.895));
#64754=CARTESIAN_POINT('Origin',(-6.1,0.,74.));
#64755=CARTESIAN_POINT('Origin',(7.5,0.,5.3));
#64756=CARTESIAN_POINT('',(5.5,-2.44929359829471E-16,5.3));
#64757=CARTESIAN_POINT('Origin',(5.2,-2.81668763803891E-16,5.3));
#64758=CARTESIAN_POINT('Origin',(7.5,0.,5.3));
#64759=CARTESIAN_POINT('Origin',(7.5,0.,8.015));
#64760=CARTESIAN_POINT('',(5.5,2.44929359829471E-16,10.7));
#64761=CARTESIAN_POINT('',(5.5,-2.44929359829471E-16,8.015));
#64762=CARTESIAN_POINT('',(9.5,-2.44929359829471E-16,10.7));
#64763=CARTESIAN_POINT('Origin',(7.5,0.,10.7));
#64764=CARTESIAN_POINT('Origin',(7.5,0.,10.7));
#64765=CARTESIAN_POINT('Origin',(2.98958333333334,11.7,37.3005642361111));
#64766=CARTESIAN_POINT('',(18.,11.7,64.));
#64767=CARTESIAN_POINT('',(18.6030508954915,12.,64.));
#64768=CARTESIAN_POINT('Ctrl Pts',(18.,11.7,64.));
#64769=CARTESIAN_POINT('Ctrl Pts',(18.,11.713619465494,64.));
#64770=CARTESIAN_POINT('Ctrl Pts',(18.0024287979856,11.7297813438019,64.));
#64771=CARTESIAN_POINT('Ctrl Pts',(18.0106135791545,11.7575865944757,64.));
#64772=CARTESIAN_POINT('Ctrl Pts',(18.0184092824072,11.7742960137653,64.));
#64773=CARTESIAN_POINT('Ctrl Pts',(18.0495162615657,11.8244485505029,64.));
#64774=CARTESIAN_POINT('Ctrl Pts',(18.0890723943383,11.8587863834563,64.));
#64775=CARTESIAN_POINT('Ctrl Pts',(18.1815113443949,11.9183072782496,64.));
#64776=CARTESIAN_POINT('Ctrl Pts',(18.2556738060324,11.9470895942332,64.));
#64777=CARTESIAN_POINT('Ctrl Pts',(18.3630495042082,11.97583451019,64.));
#64778=CARTESIAN_POINT('Ctrl Pts',(18.411396622125,11.9852271561232,64.));
#64779=CARTESIAN_POINT('Ctrl Pts',(18.5089669840554,11.9972984211227,64.));
#64780=CARTESIAN_POINT('Ctrl Pts',(18.5581873861427,12.,64.));
#64781=CARTESIAN_POINT('Ctrl Pts',(18.6030508954915,12.,64.));
#64782=CARTESIAN_POINT('',(32.,12.,48.0260462416427));
#64783=CARTESIAN_POINT('Origin',(2.98958333333334,12.,37.3005642361111));
#64784=CARTESIAN_POINT('',(32.,11.7,47.1274764390038));
#64785=CARTESIAN_POINT('Ctrl Pts',(32.,12.,48.0260462416427));
#64786=CARTESIAN_POINT('Ctrl Pts',(32.,12.,47.9061144047066));
#64787=CARTESIAN_POINT('Ctrl Pts',(32.,11.9912295487024,47.7748094270535));
#64788=CARTESIAN_POINT('Ctrl Pts',(32.,11.9602181513312,47.5820949519867));
#64789=CARTESIAN_POINT('Ctrl Pts',(32.,11.9469632164437,47.5186039284917));
#64790=CARTESIAN_POINT('Ctrl Pts',(32.,11.9132295457478,47.3965806550831));
#64791=CARTESIAN_POINT('Ctrl Pts',(32.,11.8929743256761,47.3379867237781));
#64792=CARTESIAN_POINT('Ctrl Pts',(32.,11.8446924251946,47.2387957062865));
#64793=CARTESIAN_POINT('Ctrl Pts',(32.,11.8132217751365,47.187216290166));
#64794=CARTESIAN_POINT('Ctrl Pts',(32.,11.7626708395818,47.1474100780013));
#64795=CARTESIAN_POINT('Ctrl Pts',(32.,11.748290736922,47.1387458068599));
#64796=CARTESIAN_POINT('Ctrl Pts',(32.,11.7245725726024,47.1300266648962));
#64797=CARTESIAN_POINT('Ctrl Pts',(32.,11.7112795402592,47.1274764390039));
#64798=CARTESIAN_POINT('Ctrl Pts',(32.,11.7,47.1274764390039));
#64799=CARTESIAN_POINT('Origin',(2.98958333333334,11.7,37.3005642361111));
#64800=CARTESIAN_POINT('Origin',(2.98958333333334,0.,37.3005642361111));
#64801=CARTESIAN_POINT('',(32.,-11.7,47.1274764390038));
#64802=CARTESIAN_POINT('',(32.,0.,47.1274764390038));
#64803=CARTESIAN_POINT('',(18.,-11.7,64.));
#64804=CARTESIAN_POINT('Origin',(2.98958333333334,-11.7,37.3005642361111));
#64805=CARTESIAN_POINT('',(18.,0.,64.));
#64806=CARTESIAN_POINT('Origin',(32.,0.,56.));
#64807=CARTESIAN_POINT('',(32.,12.,56.));
#64808=CARTESIAN_POINT('',(32.,12.,19.));
#64809=CARTESIAN_POINT('',(32.,11.7,56.));
#64810=CARTESIAN_POINT('',(32.,0.,56.));
#64811=CARTESIAN_POINT('',(32.,11.7,40.25));
#64812=CARTESIAN_POINT('Origin',(2.98958333333334,-11.7,37.3005642361111));
#64813=CARTESIAN_POINT('',(32.,-12.,48.0260462416427));
#64814=CARTESIAN_POINT('Ctrl Pts',(32.,-11.7,47.1274764390039));
#64815=CARTESIAN_POINT('Ctrl Pts',(32.,-11.7112795402592,47.1274764390039));
#64816=CARTESIAN_POINT('Ctrl Pts',(32.,-11.7245725726024,47.1300266648962));
#64817=CARTESIAN_POINT('Ctrl Pts',(32.,-11.748290736922,47.1387458068599));
#64818=CARTESIAN_POINT('Ctrl Pts',(32.,-11.7626708395818,47.1474100780013));
#64819=CARTESIAN_POINT('Ctrl Pts',(32.,-11.8132217751365,47.187216290166));
#64820=CARTESIAN_POINT('Ctrl Pts',(32.,-11.8446924251946,47.2387957062865));
#64821=CARTESIAN_POINT('Ctrl Pts',(32.,-11.8929743256761,47.3379867237781));
#64822=CARTESIAN_POINT('Ctrl Pts',(32.,-11.9132295457478,47.3965806550831));
#64823=CARTESIAN_POINT('Ctrl Pts',(32.,-11.9469632164437,47.5186039284917));
#64824=CARTESIAN_POINT('Ctrl Pts',(32.,-11.9602181513312,47.5820949519868));
#64825=CARTESIAN_POINT('Ctrl Pts',(32.,-11.9912295487024,47.7748094270535));
#64826=CARTESIAN_POINT('Ctrl Pts',(32.,-12.,47.9061144047066));
#64827=CARTESIAN_POINT('Ctrl Pts',(32.,-12.,48.0260462416428));
#64828=CARTESIAN_POINT('',(18.6030508954915,-12.,64.));
#64829=CARTESIAN_POINT('Origin',(2.98958333333334,-12.,37.3005642361111));
#64830=CARTESIAN_POINT('Ctrl Pts',(18.6030508954915,-12.,64.));
#64831=CARTESIAN_POINT('Ctrl Pts',(18.5581873861427,-12.,64.));
#64832=CARTESIAN_POINT('Ctrl Pts',(18.5089669840554,-11.9972984211227,64.));
#64833=CARTESIAN_POINT('Ctrl Pts',(18.411396622125,-11.9852271561232,64.));
#64834=CARTESIAN_POINT('Ctrl Pts',(18.3630495042082,-11.97583451019,64.));
#64835=CARTESIAN_POINT('Ctrl Pts',(18.2556738060324,-11.9470895942332,64.));
#64836=CARTESIAN_POINT('Ctrl Pts',(18.1815113443949,-11.9183072782496,64.));
#64837=CARTESIAN_POINT('Ctrl Pts',(18.0890723943383,-11.8587863834563,64.));
#64838=CARTESIAN_POINT('Ctrl Pts',(18.0495162615657,-11.8244485505029,64.));
#64839=CARTESIAN_POINT('Ctrl Pts',(18.0184092824072,-11.7742960137653,64.));
#64840=CARTESIAN_POINT('Ctrl Pts',(18.0106135791545,-11.7575865944757,64.));
#64841=CARTESIAN_POINT('Ctrl Pts',(18.0024287979856,-11.7297813438019,64.));
#64842=CARTESIAN_POINT('Ctrl Pts',(18.,-11.713619465494,64.));
#64843=CARTESIAN_POINT('Ctrl Pts',(18.,-11.7,64.));
#64844=CARTESIAN_POINT('Origin',(25.0000000077377,-12.,55.5637382272397));
#64845=CARTESIAN_POINT('',(32.,-12.,56.));
#64846=CARTESIAN_POINT('',(32.,-12.,19.));
#64847=CARTESIAN_POINT('',(24.,-12.,64.));
#64848=CARTESIAN_POINT('Origin',(24.0004975859988,-12.,56.0004975859988));
#64849=CARTESIAN_POINT('',(24.,-12.,64.));
#64850=CARTESIAN_POINT('Origin',(32.,0.,56.));
#64851=CARTESIAN_POINT('',(32.,-11.7,56.));
#64852=CARTESIAN_POINT('',(32.,-11.7,40.25));
#64853=CARTESIAN_POINT('',(32.,0.,56.));
#64854=CARTESIAN_POINT('Origin',(7.5,0.,10.7));
#64855=CARTESIAN_POINT('',(9.8,-2.81668763803891E-16,11.));
#64856=CARTESIAN_POINT('Origin',(7.5,0.,11.));
#64857=CARTESIAN_POINT('Origin',(9.8,-2.81668763803891E-16,10.7));
#64858=CARTESIAN_POINT('Origin',(23.5,0.,11.));
#64859=CARTESIAN_POINT('Origin',(0.,0.,11.));
#64860=CARTESIAN_POINT('',(-10.5,-18.7,11.));
#64861=CARTESIAN_POINT('Origin',(-10.5,-17.5,11.));
#64862=CARTESIAN_POINT('',(57.5,-18.7,11.));
#64863=CARTESIAN_POINT('',(5.75,-18.7,11.));
#64864=CARTESIAN_POINT('',(58.7,-17.5,11.));
#64865=CARTESIAN_POINT('Origin',(57.5,-17.5,11.));
#64866=CARTESIAN_POINT('',(58.7,17.5,11.));
#64867=CARTESIAN_POINT('',(58.7,-9.5,11.));
#64868=CARTESIAN_POINT('',(57.5,18.7,11.));
#64869=CARTESIAN_POINT('Origin',(57.5,17.5,11.));
#64870=CARTESIAN_POINT('',(-10.5,18.7,11.));
#64871=CARTESIAN_POINT('',(41.25,18.7,11.));
#64872=CARTESIAN_POINT('Origin',(-10.5,17.5,11.));
#64873=CARTESIAN_POINT('',(-10.25,-15.,11.));
#64874=CARTESIAN_POINT('Origin',(-8.,-15.,11.));
#64875=CARTESIAN_POINT('',(51.75,-15.,11.));
#64876=CARTESIAN_POINT('Origin',(54.,-15.,11.));
#64877=CARTESIAN_POINT('',(-10.25,15.,11.));
#64878=CARTESIAN_POINT('Origin',(-8.,15.,11.));
#64879=CARTESIAN_POINT('',(51.75,15.,11.));
#64880=CARTESIAN_POINT('Origin',(54.,15.,11.));
#64881=CARTESIAN_POINT('',(24.,12.3,11.));
#64882=CARTESIAN_POINT('',(24.,12.025,11.));
#64883=CARTESIAN_POINT('',(24.,0.,11.));
#64884=CARTESIAN_POINT('',(58.5,12.3,11.));
#64885=CARTESIAN_POINT('',(23.875,12.3,11.));
#64886=CARTESIAN_POINT('',(58.5,12.025,11.));
#64887=CARTESIAN_POINT('',(58.5,0.,11.));
#64888=CARTESIAN_POINT('',(-20.,12.025,11.));
#64889=CARTESIAN_POINT('',(25.,0.,11.));
#64890=CARTESIAN_POINT('',(58.5,-12.025,11.));
#64891=CARTESIAN_POINT('',(-20.,-12.025,11.));
#64892=CARTESIAN_POINT('',(58.5,-12.3,11.));
#64893=CARTESIAN_POINT('',(58.5,0.,11.));
#64894=CARTESIAN_POINT('',(24.,-12.3,11.));
#64895=CARTESIAN_POINT('',(23.875,-12.3,11.));
#64896=CARTESIAN_POINT('',(24.,-12.025,11.));
#64897=CARTESIAN_POINT('',(24.,0.,11.));
#64898=CARTESIAN_POINT('',(-20.,-12.025,11.));
#64899=CARTESIAN_POINT('',(-20.,12.025,11.));
#64900=CARTESIAN_POINT('Origin',(-6.4,0.,64.3216946934853));
#64901=CARTESIAN_POINT('',(-6.1257913174651,-4.52,64.2));
#64902=CARTESIAN_POINT('Origin',(-6.4,-4.52,64.3216946934853));
#64903=CARTESIAN_POINT('Origin',(-6.4,-4.39830530651473,64.3216946934853));
#64904=CARTESIAN_POINT('Origin',(-6.4,4.39830530651473,64.3216946934853));
#64905=CARTESIAN_POINT('Origin',(-6.4,0.,69.));
#64906=CARTESIAN_POINT('Origin',(-6.4,-1.35323471305782E-16,67.895));
#64907=CARTESIAN_POINT('Origin',(-6.4,0.,74.));
#64908=CARTESIAN_POINT('Origin',(-6.4,-1.35323471305782E-16,72.895));
#64909=CARTESIAN_POINT('Origin',(-6.4,0.,82.));
#64910=CARTESIAN_POINT('Origin',(-6.4,-1.35323471305782E-16,80.895));
#64911=CARTESIAN_POINT('Origin',(-6.4,0.,87.));
#64912=CARTESIAN_POINT('Origin',(-6.4,-1.35323471305782E-16,85.895));
#64913=CARTESIAN_POINT('Origin',(55.7,0.,13.7767804169048));
#64914=CARTESIAN_POINT('',(55.8157264050162,12.5767804169048,13.5));
#64915=CARTESIAN_POINT('',(56.,12.3,13.7767804169048));
#64916=CARTESIAN_POINT('Origin',(55.7,12.3,13.7767804169048));
#64917=CARTESIAN_POINT('',(56.,-12.3,13.7767804169048));
#64918=CARTESIAN_POINT('',(56.,0.,13.7767804169048));
#64919=CARTESIAN_POINT('',(55.8157264050162,-12.5767804169048,13.5));
#64920=CARTESIAN_POINT('Origin',(55.7,-12.3,13.7767804169048));
#64921=CARTESIAN_POINT('',(55.8157264050162,-11.8842735949838,13.5));
#64922=CARTESIAN_POINT('',(55.8157264050162,0.,13.5));
#64923=CARTESIAN_POINT('',(55.7241152569761,-11.9759739037501,13.4777512304013));
#64924=CARTESIAN_POINT('Ctrl Pts',(55.8157264050162,-11.8842735949838,13.5));
#64925=CARTESIAN_POINT('Ctrl Pts',(55.8154916174147,-11.8845083825853,13.4999018314758));
#64926=CARTESIAN_POINT('Ctrl Pts',(55.8152567556258,-11.8847432497585,13.4998039828686));
#64927=CARTESIAN_POINT('Ctrl Pts',(55.7851007909116,-11.9149005830658,13.4872853308607));
#64928=CARTESIAN_POINT('Ctrl Pts',(55.7539530047584,-11.9461178286373,13.4801575003837));
#64929=CARTESIAN_POINT('Ctrl Pts',(55.7241152569761,-11.9759739037501,13.4777512304013));
#64930=CARTESIAN_POINT('',(55.7241152569761,11.9759739037501,13.4777512304013));
#64931=CARTESIAN_POINT('',(55.7241152569761,0.,13.4777512304013));
#64932=CARTESIAN_POINT('',(55.8157264050162,11.8842735949838,13.5));
#64933=CARTESIAN_POINT('Ctrl Pts',(55.7241152569761,11.9759739037501,13.4777512304013));
#64934=CARTESIAN_POINT('Ctrl Pts',(55.7539530047584,11.9461178286373,13.4801575003837));
#64935=CARTESIAN_POINT('Ctrl Pts',(55.7851007909116,11.9149005830658,13.4872853308607));
#64936=CARTESIAN_POINT('Ctrl Pts',(55.8152567556258,11.8847432497585,13.4998039828686));
#64937=CARTESIAN_POINT('Ctrl Pts',(55.8154916174147,11.8845083825853,13.4999018314758));
#64938=CARTESIAN_POINT('Ctrl Pts',(55.8157264050162,11.8842735949838,13.5));
#64939=CARTESIAN_POINT('',(55.8157264050162,0.,13.5));
#64940=CARTESIAN_POINT('Origin',(55.7,12.3,83.875));
#64941=CARTESIAN_POINT('Origin',(55.7,12.3,13.5));
#64942=CARTESIAN_POINT('',(56.,12.3,83.875));
#64943=CARTESIAN_POINT('Origin',(56.,12.,13.5));
#64944=CARTESIAN_POINT('',(55.7,12.,13.5));
#64945=CARTESIAN_POINT('',(56.,11.7,13.5));
#64946=CARTESIAN_POINT('',(54.5,12.,13.5));
#64947=CARTESIAN_POINT('',(40.125,12.,13.5));
#64948=CARTESIAN_POINT('',(54.5,12.,13.5));
#64949=CARTESIAN_POINT('Origin',(58.5,11.85,13.5));
#64950=CARTESIAN_POINT('',(55.7001044519953,12.,13.4758148751609));
#64951=CARTESIAN_POINT('Ctrl Pts',(55.7241152569761,11.9759739037501,13.4777512304013));
#64952=CARTESIAN_POINT('Ctrl Pts',(55.7121615840951,11.9879349189719,13.4767872245238));
#64953=CARTESIAN_POINT('Ctrl Pts',(55.7001044519953,12.,13.4758148751609));
#64954=CARTESIAN_POINT('Origin',(58.5,12.,13.5));
#64955=CARTESIAN_POINT('Origin',(25.,0.,11.));
#64956=CARTESIAN_POINT('',(55.7001044519953,-12.,13.4758148751609));
#64957=CARTESIAN_POINT('Ctrl Pts',(55.7001044519953,-12.,13.4758148751609));
#64958=CARTESIAN_POINT('Ctrl Pts',(55.7121615840951,-11.9879349189719,13.4767872245238));
#64959=CARTESIAN_POINT('Ctrl Pts',(55.7241152569761,-11.9759739037501,13.4777512304013));
#64960=CARTESIAN_POINT('',(32.44,-12.,11.6));
#64961=CARTESIAN_POINT('',(26.6505556991471,-12.,11.1331093305764));
#64962=CARTESIAN_POINT('',(31.6915937956643,-12.025,11.5396446609407));
#64963=CARTESIAN_POINT('',(24.7539493851376,-12.2567472907873,10.9801572084788));
#64964=CARTESIAN_POINT('',(56.,-12.025,13.5));
#64965=CARTESIAN_POINT('',(31.6915937956643,12.025,11.5396446609407));
#64966=CARTESIAN_POINT('',(56.,12.025,13.5));
#64967=CARTESIAN_POINT('',(32.44,12.,11.6));
#64968=CARTESIAN_POINT('',(24.7539493851376,12.2567472907873,10.9801572084788));
#64969=CARTESIAN_POINT('',(26.6505556991471,12.,11.1331093305764));
#64970=CARTESIAN_POINT('Origin',(56.,0.,100.));
#64971=CARTESIAN_POINT('',(56.,-12.3,83.875));
#64972=CARTESIAN_POINT('Origin',(23.,-4.82,89.));
#64973=CARTESIAN_POINT('Origin',(23.,-4.52,89.));
#64974=CARTESIAN_POINT('Origin',(-6.1,-4.52,62.));
#64975=CARTESIAN_POINT('',(-6.,-4.52,92.));
#64976=CARTESIAN_POINT('',(10.45,-4.52,92.));
#64977=CARTESIAN_POINT('Origin',(-5.9999073877354,-4.52,87.9999073877354));
#64978=CARTESIAN_POINT('Origin',(23.,4.82,89.));
#64979=CARTESIAN_POINT('Origin',(23.,4.52,89.));
#64980=CARTESIAN_POINT('Origin',(4.52,4.52,62.));
#64981=CARTESIAN_POINT('',(-6.,4.52,92.));
#64982=CARTESIAN_POINT('Origin',(-5.9999073877354,4.52,87.9999073877354));
#64983=CARTESIAN_POINT('',(15.76,4.52,92.));
#64984=CARTESIAN_POINT('Origin',(55.7,-12.3,83.875));
#64985=CARTESIAN_POINT('Origin',(55.7,-12.3,13.5));
#64986=CARTESIAN_POINT('Origin',(56.,-12.,13.5));
#64987=CARTESIAN_POINT('',(54.5,-12.,13.5));
#64988=CARTESIAN_POINT('',(54.5,-12.,13.5));
#64989=CARTESIAN_POINT('',(55.7,-12.,13.5));
#64990=CARTESIAN_POINT('',(40.125,-12.,13.5));
#64991=CARTESIAN_POINT('',(56.,-11.7,13.5));
#64992=CARTESIAN_POINT('Origin',(54.5,-12.,13.5));
#64993=CARTESIAN_POINT('',(54.5,-12.,37.5));
#64994=CARTESIAN_POINT('Origin',(-8.5,-12.,89.));
#64995=CARTESIAN_POINT('',(-9.56230262611138,-12.,89.));
#64996=CARTESIAN_POINT('Ctrl Pts',(-9.56230262611138,-12.,89.));
#64997=CARTESIAN_POINT('Ctrl Pts',(-9.62927380717335,-11.9355211853595,
88.9999999999994));
#64998=CARTESIAN_POINT('Ctrl Pts',(-9.69862382425291,-11.8685749135175,
88.999999999999));
#64999=CARTESIAN_POINT('',(7.875,-12.,89.));
#65000=CARTESIAN_POINT('Origin',(-5.99999999999999,-11.85,88.));
#65001=CARTESIAN_POINT('',(-9.87296247153814,-11.7000202118089,88.9999999999986));
#65002=CARTESIAN_POINT('Ctrl Pts',(-9.86042062850558,-11.7000210181973,
89.0473702429761));
#65003=CARTESIAN_POINT('Ctrl Pts',(-9.86470019847172,-11.7000207520943,
89.0315975247012));
#65004=CARTESIAN_POINT('Ctrl Pts',(-9.86888098571992,-11.700020483277,89.0158063555326));
#65005=CARTESIAN_POINT('Ctrl Pts',(-9.8729624715378,-11.7000202118089,88.9999999999985));
#65006=CARTESIAN_POINT('Ctrl Pts',(-9.87296247153813,-11.7000202118089,
88.9999999999972));
#65007=CARTESIAN_POINT('Ctrl Pts',(-9.8927585501957,-11.7000188951308,88.9233357969584));
#65008=CARTESIAN_POINT('Ctrl Pts',(-9.91021935852739,-11.7000175158046,
88.8463010263897));
#65009=CARTESIAN_POINT('Ctrl Pts',(-9.9759579265626,-11.7000112708308,88.5108379773071));
#65010=CARTESIAN_POINT('Ctrl Pts',(-9.99999418569865,-11.7000058143013,
88.2511302792877));
#65011=CARTESIAN_POINT('Ctrl Pts',(-10.,-11.7,88.));
#65012=CARTESIAN_POINT('',(-9.7,-12.,88.));
#65013=CARTESIAN_POINT('',(-10.,-11.7,88.));
#65014=CARTESIAN_POINT('Origin',(-5.99999999999999,-12.,88.));
#65015=CARTESIAN_POINT('Origin',(-5.99999999999999,-11.85,88.));
#65016=CARTESIAN_POINT('',(-6.,-12.,91.7));
#65017=CARTESIAN_POINT('Origin',(-5.99999999999999,-12.,88.));
#65018=CARTESIAN_POINT('',(-6.,-11.7,92.));
#65019=CARTESIAN_POINT('',(-6.,-11.7,92.));
#65020=CARTESIAN_POINT('Ctrl Pts',(-6.,-11.7,92.));
#65021=CARTESIAN_POINT('Ctrl Pts',(-6.25107275476676,-11.7000058129695,
91.9999941870305));
#65022=CARTESIAN_POINT('Ctrl Pts',(-6.51071737252271,-11.700011268298,91.9759691389564));
#65023=CARTESIAN_POINT('Ctrl Pts',(-7.02728102192247,-11.7000208852123,
91.874766271675));
#65024=CARTESIAN_POINT('Ctrl Pts',(-7.28420360710883,-11.7000250470743,
91.7975968363583));
#65025=CARTESIAN_POINT('Ctrl Pts',(-7.77697838430535,-11.7000317308133,
91.5934962067892));
#65026=CARTESIAN_POINT('Ctrl Pts',(-8.01322300290132,-11.7000342580129,
91.4664024747671));
#65027=CARTESIAN_POINT('Ctrl Pts',(-8.29756107931325,-11.7000364154344,
91.2752443716494));
#65028=CARTESIAN_POINT('Ctrl Pts',(-8.36185049180696,-11.7000368371963,
91.2291710362983));
#65029=CARTESIAN_POINT('Ctrl Pts',(-8.42436827442,-11.7000371816705,91.1815312379426));
#65030=CARTESIAN_POINT('Origin',(24.25,-12.,61.5));
#65031=CARTESIAN_POINT('',(-9.7,-12.,68.));
#65032=CARTESIAN_POINT('',(-9.7,-12.,64.75));
#65033=CARTESIAN_POINT('',(-6.,-12.,64.3));
#65034=CARTESIAN_POINT('Origin',(-5.99999999999999,-12.,68.));
#65035=CARTESIAN_POINT('',(24.,-12.,64.3));
#65036=CARTESIAN_POINT('',(24.125,-12.,64.3));
#65037=CARTESIAN_POINT('',(32.3,-12.,56.));
#65038=CARTESIAN_POINT('Origin',(24.,-12.,56.));
#65039=CARTESIAN_POINT('',(32.3,-12.,19.));
#65040=CARTESIAN_POINT('',(32.3,-12.,40.25));
#65041=CARTESIAN_POINT('',(27.7589892258425,-12.,11.6));
#65042=CARTESIAN_POINT('Origin',(24.,-12.,19.));
#65043=CARTESIAN_POINT('',(24.0625,-12.,11.6));
#65044=CARTESIAN_POINT('Origin',(58.5,-12.,13.5));
#65045=CARTESIAN_POINT('',(32.3,-12.,100.));
#65046=CARTESIAN_POINT('Origin',(44.,-12.,100.));
#65047=CARTESIAN_POINT('',(32.3,-12.,97.));
#65048=CARTESIAN_POINT('',(32.3,-12.,79.25));
#65049=CARTESIAN_POINT('',(27.,-12.,91.7));
#65050=CARTESIAN_POINT('Origin',(27.,-12.,97.));
#65051=CARTESIAN_POINT('',(9.125,-12.,91.7));
#65052=CARTESIAN_POINT('',(40.6103012561798,-12.,83.4957704544067));
#65053=CARTESIAN_POINT('',(41.4561398029327,-12.,85.8598899841309));
#65054=CARTESIAN_POINT('Ctrl Pts',(40.6103012561798,-12.,83.4957704544067));
#65055=CARTESIAN_POINT('Ctrl Pts',(40.6103012561798,-12.,85.0140514373779));
#65056=CARTESIAN_POINT('Ctrl Pts',(41.4561398029327,-12.,85.8598899841309));
#65057=CARTESIAN_POINT('',(43.8118011951447,-12.,86.7057290077209));
#65058=CARTESIAN_POINT('Ctrl Pts',(41.4561398029327,-12.,85.8598899841309));
#65059=CARTESIAN_POINT('Ctrl Pts',(42.3019783496857,-12.,86.7057290077209));
#65060=CARTESIAN_POINT('Ctrl Pts',(43.8118011951447,-12.,86.7057290077209));
#65061=CARTESIAN_POINT('',(46.1970684528351,-12.,85.874692440033));
#65062=CARTESIAN_POINT('Ctrl Pts',(43.8118011951447,-12.,86.7057290077209));
#65063=CARTESIAN_POINT('Ctrl Pts',(45.35968708992,-12.,86.7057290077209));
#65064=CARTESIAN_POINT('Ctrl Pts',(46.1970684528351,-12.,85.874692440033));
#65065=CARTESIAN_POINT('',(47.0344479084015,-12.,83.5465202331543));
#65066=CARTESIAN_POINT('Ctrl Pts',(46.1970684528351,-12.,85.874692440033));
#65067=CARTESIAN_POINT('Ctrl Pts',(47.0344479084015,-12.,85.0436553955078));
#65068=CARTESIAN_POINT('Ctrl Pts',(47.0344479084015,-12.,83.5465202331543));
#65069=CARTESIAN_POINT('',(46.6686222553253,-12.,81.7639150619507));
#65070=CARTESIAN_POINT('Ctrl Pts',(47.0344479084015,-12.,83.5465202331543));
#65071=CARTESIAN_POINT('Ctrl Pts',(47.0344479084015,-12.,82.4596176147461));
#65072=CARTESIAN_POINT('Ctrl Pts',(46.6686222553253,-12.,81.7639150619507));
#65073=CARTESIAN_POINT('',(45.611323595047,-12.,80.6812410354614));
#65074=CARTESIAN_POINT('Ctrl Pts',(46.6686222553253,-12.,81.7639150619507));
#65075=CARTESIAN_POINT('Ctrl Pts',(46.3027966022491,-12.,81.0682125091553));
#65076=CARTESIAN_POINT('Ctrl Pts',(45.611323595047,-12.,80.6812410354614));
#65077=CARTESIAN_POINT('',(43.8879272937775,-12.,80.2942695617676));
#65078=CARTESIAN_POINT('Ctrl Pts',(45.611323595047,-12.,80.6812410354614));
#65079=CARTESIAN_POINT('Ctrl Pts',(44.9198505878448,-12.,80.2942695617676));
#65080=CARTESIAN_POINT('Ctrl Pts',(43.8879272937775,-12.,80.2942695617676));
#65081=CARTESIAN_POINT('',(42.1518423557281,-12.,80.6283760070801));
#65082=CARTESIAN_POINT('Ctrl Pts',(43.8879272937775,-12.,80.2942695617676));
#65083=CARTESIAN_POINT('Ctrl Pts',(42.8390867710114,-12.,80.2942695617676));
#65084=CARTESIAN_POINT('Ctrl Pts',(42.1518423557281,-12.,80.6283760070801));
#65085=CARTESIAN_POINT('',(41.0374491214752,-12.,81.6856746673584));
#65086=CARTESIAN_POINT('Ctrl Pts',(42.1518423557281,-12.,80.6283760070801));
#65087=CARTESIAN_POINT('Ctrl Pts',(41.4645979404449,-12.,80.9624824523926));
#65088=CARTESIAN_POINT('Ctrl Pts',(41.0374491214752,-12.,81.6856746673584));
#65089=CARTESIAN_POINT('Ctrl Pts',(41.0374491214752,-12.,81.6856746673584));
#65090=CARTESIAN_POINT('Ctrl Pts',(40.6103012561798,-12.,82.4088668823242));
#65091=CARTESIAN_POINT('Ctrl Pts',(40.6103012561798,-12.,83.4957704544067));
#65092=CARTESIAN_POINT('',(47.7322647571564,-12.,82.1255111694336));
#65093=CARTESIAN_POINT('',(49.5719635486603,-12.,82.1255111694336));
#65094=CARTESIAN_POINT('',(36.9109817743301,-12.,82.1255111694336));
#65095=CARTESIAN_POINT('',(49.5719635486603,-12.,80.3999996185303));
#65096=CARTESIAN_POINT('',(49.5719635486603,-12.,70.9499998092651));
#65097=CARTESIAN_POINT('',(47.7322647571564,-12.,80.3999996185303));
#65098=CARTESIAN_POINT('',(35.9911323785782,-12.,80.3999996185303));
#65099=CARTESIAN_POINT('',(47.7322647571564,-12.,71.8127555847168));
#65100=CARTESIAN_POINT('',(-0.990000000000002,-12.,78.));
#65101=CARTESIAN_POINT('Origin',(9.31,-12.,78.));
#65102=CARTESIAN_POINT('',(33.6490461826324,-12.,86.5999994277954));
#65103=CARTESIAN_POINT('',(35.4379951953888,-12.,86.5999994277954));
#65104=CARTESIAN_POINT('',(29.8439975976944,-12.,86.5999994277954));
#65105=CARTESIAN_POINT('',(37.772510766983,-12.,83.1698579788208));
#65106=CARTESIAN_POINT('',(40.6718459545618,-12.,78.9098179420808));
#65107=CARTESIAN_POINT('',(37.772510766983,-12.,86.5999994277954));
#65108=CARTESIAN_POINT('',(37.772510766983,-12.,74.0499997138977));
#65109=CARTESIAN_POINT('',(39.5783770084381,-12.,86.5999994277954));
#65110=CARTESIAN_POINT('',(31.9141885042191,-12.,86.5999994277954));
#65111=CARTESIAN_POINT('',(39.5783770084381,-12.,80.3999996185303));
#65112=CARTESIAN_POINT('',(39.5783770084381,-12.,70.9499998092651));
#65113=CARTESIAN_POINT('',(37.772510766983,-12.,80.3999996185303));
#65114=CARTESIAN_POINT('',(31.0112553834915,-12.,80.3999996185303));
#65115=CARTESIAN_POINT('',(35.4506828784943,-12.,83.8042373657227));
#65116=CARTESIAN_POINT('',(38.8639403839799,-12.,78.7997578783887));
#65117=CARTESIAN_POINT('',(35.4506828784943,-12.,80.3999996185303));
#65118=CARTESIAN_POINT('',(35.4506828784943,-12.,70.9499998092651));
#65119=CARTESIAN_POINT('',(33.6490461826324,-12.,80.3999996185303));
#65120=CARTESIAN_POINT('',(28.9495230913162,-12.,80.3999996185303));
#65121=CARTESIAN_POINT('',(33.6490461826324,-12.,74.0499997138977));
#65122=CARTESIAN_POINT('',(54.3509571552277,-12.,86.7057294845581));
#65123=CARTESIAN_POINT('',(54.3509571552277,-12.,80.3999996185303));
#65124=CARTESIAN_POINT('',(54.3509571552277,-12.,70.9499998092651));
#65125=CARTESIAN_POINT('',(52.6085274219513,-12.,80.3999996185303));
#65126=CARTESIAN_POINT('',(38.4292637109756,-12.,80.3999996185303));
#65127=CARTESIAN_POINT('',(52.6085274219513,-12.,84.5319232940674));
#65128=CARTESIAN_POINT('',(52.6085274219513,-12.,73.0159616470337));
#65129=CARTESIAN_POINT('',(51.7901794910431,-12.,84.0117321014404));
#65130=CARTESIAN_POINT('Ctrl Pts',(52.6085274219513,-12.,84.5319232940674));
#65131=CARTESIAN_POINT('Ctrl Pts',(52.1856091022491,-12.,84.2105045318604));
#65132=CARTESIAN_POINT('Ctrl Pts',(51.7901794910431,-12.,84.0117321014404));
#65133=CARTESIAN_POINT('',(50.7984325885773,-12.,83.6311044692993));
#65134=CARTESIAN_POINT('Ctrl Pts',(51.7901794910431,-12.,84.0117321014404));
#65135=CARTESIAN_POINT('Ctrl Pts',(51.394749879837,-12.,83.8129596710205));
#65136=CARTESIAN_POINT('Ctrl Pts',(50.7984325885773,-12.,83.6311044692993));
#65137=CARTESIAN_POINT('',(50.7984325885773,-12.,85.0436553955078));
#65138=CARTESIAN_POINT('',(50.7984325885773,-12.,73.2718276977539));
#65139=CARTESIAN_POINT('',(52.1644623279572,-12.,85.7245559692383));
#65140=CARTESIAN_POINT('Ctrl Pts',(50.7984325885773,-12.,85.0436553955078));
#65141=CARTESIAN_POINT('Ctrl Pts',(51.6781055927277,-12.,85.3270111083984));
#65142=CARTESIAN_POINT('Ctrl Pts',(52.1644623279572,-12.,85.7245559692383));
#65143=CARTESIAN_POINT('',(52.9257175922394,-12.,86.7057294845581));
#65144=CARTESIAN_POINT('Ctrl Pts',(52.1644623279572,-12.,85.7245559692383));
#65145=CARTESIAN_POINT('Ctrl Pts',(52.6508209705353,-12.,86.122100353241));
#65146=CARTESIAN_POINT('Ctrl Pts',(52.9257175922394,-12.,86.7057294845581));
#65147=CARTESIAN_POINT('',(39.3004785776138,-12.,86.7057294845581));
#65148=CARTESIAN_POINT('Origin',(-5.9999073877354,0.,87.9999073877354));
#65149=CARTESIAN_POINT('Origin',(-5.9999073877354,-12.,87.9999073877354));
#65150=CARTESIAN_POINT('Origin',(18.5190608795662,-12.,105.));
#65151=CARTESIAN_POINT('Origin',(-8.5,12.,89.));
#65152=CARTESIAN_POINT('',(-9.56230262611138,12.,89.));
#65153=CARTESIAN_POINT('',(7.875,12.,89.));
#65154=CARTESIAN_POINT('Ctrl Pts',(-9.69862382425291,11.8685749135175,88.999999999999));
#65155=CARTESIAN_POINT('Ctrl Pts',(-9.62927380717316,11.9355211853597,88.9999999999994));
#65156=CARTESIAN_POINT('Ctrl Pts',(-9.56230262611138,12.,89.));
#65157=CARTESIAN_POINT('Origin',(54.5,12.,13.5));
#65158=CARTESIAN_POINT('',(54.5,12.,37.5));
#65159=CARTESIAN_POINT('Origin',(44.,0.,100.));
#65160=CARTESIAN_POINT('',(32.,11.7,100.));
#65161=CARTESIAN_POINT('Origin',(44.,11.7,100.));
#65162=CARTESIAN_POINT('',(32.,12.,100.));
#65163=CARTESIAN_POINT('',(32.,0.,100.));
#65164=CARTESIAN_POINT('Origin',(44.,12.,100.));
#65165=CARTESIAN_POINT('Origin',(44.,11.85,100.));
#65166=CARTESIAN_POINT('',(32.3,12.,100.));
#65167=CARTESIAN_POINT('Origin',(44.,12.,100.));
#65168=CARTESIAN_POINT('',(32.,11.7,100.));
#65169=CARTESIAN_POINT('Origin',(24.25,12.,61.5));
#65170=CARTESIAN_POINT('',(27.7589892258425,12.,11.6));
#65171=CARTESIAN_POINT('',(24.0625,12.,11.6));
#65172=CARTESIAN_POINT('',(32.3,12.,19.));
#65173=CARTESIAN_POINT('Origin',(24.,12.,19.));
#65174=CARTESIAN_POINT('',(32.3,12.,56.));
#65175=CARTESIAN_POINT('',(32.3,12.,40.25));
#65176=CARTESIAN_POINT('',(24.,12.,64.3));
#65177=CARTESIAN_POINT('Origin',(24.,12.,56.));
#65178=CARTESIAN_POINT('',(-6.,12.,64.3));
#65179=CARTESIAN_POINT('',(24.125,12.,64.3));
#65180=CARTESIAN_POINT('',(-9.70000000000001,12.,68.));
#65181=CARTESIAN_POINT('Origin',(-5.99999999999999,12.,68.));
#65182=CARTESIAN_POINT('',(-9.7,12.,88.));
#65183=CARTESIAN_POINT('',(-9.7,12.,64.75));
#65184=CARTESIAN_POINT('Origin',(-5.99999999999999,12.,88.));
#65185=CARTESIAN_POINT('',(-6.,12.,91.7));
#65186=CARTESIAN_POINT('Origin',(-5.99999999999999,12.,88.));
#65187=CARTESIAN_POINT('',(27.,12.,91.7));
#65188=CARTESIAN_POINT('',(9.125,12.,91.7));
#65189=CARTESIAN_POINT('',(32.3,12.,97.));
#65190=CARTESIAN_POINT('Origin',(27.,12.,97.));
#65191=CARTESIAN_POINT('',(32.3,12.,79.25));
#65192=CARTESIAN_POINT('',(-0.990000000000002,12.,78.));
#65193=CARTESIAN_POINT('Origin',(9.31,12.,78.));
#65194=CARTESIAN_POINT('Origin',(-5.99999999999999,11.85,88.));
#65195=CARTESIAN_POINT('',(-10.,11.7,88.));
#65196=CARTESIAN_POINT('',(-9.87296247153813,11.7000202118089,88.9999999999986));
#65197=CARTESIAN_POINT('Ctrl Pts',(-10.,11.7,88.));
#65198=CARTESIAN_POINT('Ctrl Pts',(-9.99999418587805,11.700005814122,88.2511225307642));
#65199=CARTESIAN_POINT('Ctrl Pts',(-9.97595940826116,11.700011270506,88.5108224697674));
#65200=CARTESIAN_POINT('Ctrl Pts',(-9.91022279769886,11.7000175155328,88.8462858496168));
#65201=CARTESIAN_POINT('Ctrl Pts',(-9.89276050036787,11.7000188950011,88.9233282445336));
#65202=CARTESIAN_POINT('Ctrl Pts',(-9.87296247153813,11.7000202118089,88.9999999999972));
#65203=CARTESIAN_POINT('Ctrl Pts',(-9.8729624715378,11.7000202118089,88.9999999999985));
#65204=CARTESIAN_POINT('Ctrl Pts',(-9.86888099751967,11.7000204832762,89.0158063098357));
#65205=CARTESIAN_POINT('Ctrl Pts',(-9.8647001926743,11.7000207520947,89.0315975460681));
#65206=CARTESIAN_POINT('Ctrl Pts',(-9.86042062850558,11.7000210181973,89.0473702429761));
#65207=CARTESIAN_POINT('Origin',(-5.9999073877354,0.,87.9999073877354));
#65208=CARTESIAN_POINT('Origin',(-5.9999073877354,12.,87.9999073877354));
#65209=CARTESIAN_POINT('Origin',(18.5190608795662,12.,105.));
#65210=CARTESIAN_POINT('Origin',(-5.9999073877354,0.,87.9999073877354));
#65211=CARTESIAN_POINT('',(-6.,-4.72,92.));
#65212=CARTESIAN_POINT('',(-6.,0.,92.));
#65213=CARTESIAN_POINT('Origin',(-5.9999073877354,-0.71990738773516,87.9999073877354));
#65214=CARTESIAN_POINT('Origin',(-5.9999073877354,0.,87.9999073877354));
#65215=CARTESIAN_POINT('',(-6.,4.72,92.));
#65216=CARTESIAN_POINT('Origin',(-5.9999073877354,0.71990738773516,87.9999073877354));
#65217=CARTESIAN_POINT('',(-6.,0.,92.));
#65218=CARTESIAN_POINT('Origin',(25.,-12.025,73.));
#65219=CARTESIAN_POINT('',(56.4658830061617,-12.025,11.5396446609407));
#65220=CARTESIAN_POINT('',(24.53125,-12.025,11.5396446609407));
#65221=CARTESIAN_POINT('',(56.7593104814471,-12.025,11.275));
#65222=CARTESIAN_POINT('Origin',(58.5,-12.025,13.5));
#65223=CARTESIAN_POINT('',(57.3600986884822,-12.025,11.275));
#65224=CARTESIAN_POINT('',(24.4375,-12.025,11.275));
#65225=CARTESIAN_POINT('Origin',(58.5,-12.025,13.5));
#65226=CARTESIAN_POINT('Origin',(25.,12.025,73.));
#65227=CARTESIAN_POINT('',(56.4658830061617,12.025,11.5396446609407));
#65228=CARTESIAN_POINT('',(24.53125,12.025,11.5396446609407));
#65229=CARTESIAN_POINT('',(57.3600986884822,12.025,11.275));
#65230=CARTESIAN_POINT('Origin',(58.5,12.025,13.5));
#65231=CARTESIAN_POINT('',(56.7593104814471,12.025,11.275));
#65232=CARTESIAN_POINT('',(24.4375,12.025,11.275));
#65233=CARTESIAN_POINT('Origin',(58.5,12.025,13.5));
#65234=CARTESIAN_POINT('Origin',(25.,12.025,73.));
#65235=CARTESIAN_POINT('Origin',(24.,12.025,19.));
#65236=CARTESIAN_POINT('Origin',(25.,-12.025,73.));
#65237=CARTESIAN_POINT('Origin',(24.,-12.025,19.));
#65238=CARTESIAN_POINT('Origin',(24.,0.,19.));
#65239=CARTESIAN_POINT('Origin',(24.,-4.29999999999991,19.));
#65240=CARTESIAN_POINT('Origin',(24.,0.,19.));
#65241=CARTESIAN_POINT('',(26.1702534414211,12.,11.3));
#65242=CARTESIAN_POINT('Origin',(24.,12.,19.));
#65243=CARTESIAN_POINT('Origin',(24.,4.29999999999991,19.));
#65244=CARTESIAN_POINT('Origin',(14.26,4.62,64.1));
#65245=CARTESIAN_POINT('',(4.72,4.72,64.));
#65246=CARTESIAN_POINT('',(14.26,4.72,64.));
#65247=CARTESIAN_POINT('',(4.72,4.72,64.));
#65248=CARTESIAN_POINT('Origin',(-5.99999999999999,11.85,68.));
#65249=CARTESIAN_POINT('',(-10.,11.7,68.));
#65250=CARTESIAN_POINT('',(-6.,11.7,64.));
#65251=CARTESIAN_POINT('Origin',(58.5,-11.85,13.5));
#65252=CARTESIAN_POINT('',(56.6959605211562,-12.212132034356,11.087867965644));
#65253=CARTESIAN_POINT('Origin',(58.5,-11.6298989873223,12.4935028842544));
#65254=CARTESIAN_POINT('Ctrl Pts',(56.7593104814471,-12.025,11.275));
#65255=CARTESIAN_POINT('Ctrl Pts',(56.7276355013012,-12.116893843234,11.183106156766));
#65256=CARTESIAN_POINT('Ctrl Pts',(56.6959605211562,-12.212132034356,11.087867965644));
#65257=CARTESIAN_POINT('Origin',(58.5,-11.85,13.5));
#65258=CARTESIAN_POINT('Origin',(24.0625,12.106066017178,11.343933982822));
#65259=CARTESIAN_POINT('',(56.6959605211562,12.212132034356,11.087867965644));
#65260=CARTESIAN_POINT('Origin',(58.5,11.6298989873223,12.4935028842544));
#65261=CARTESIAN_POINT('',(27.1391971013664,12.212132034356,11.087867965644));
#65262=CARTESIAN_POINT('',(24.0625,12.212132034356,11.087867965644));
#65263=CARTESIAN_POINT('Origin',(24.,10.0189862838483,16.3825901807804));
#65264=CARTESIAN_POINT('Origin',(58.5,0.,13.5));
#65265=CARTESIAN_POINT('Origin',(58.5,9.79999999999997,13.5));
#65266=CARTESIAN_POINT('Origin',(58.5,11.85,13.5));
#65267=CARTESIAN_POINT('Ctrl Pts',(56.6959605211562,12.212132034356,11.087867965644));
#65268=CARTESIAN_POINT('Ctrl Pts',(56.7276355013016,12.1168938432326,11.1831061567674));
#65269=CARTESIAN_POINT('Ctrl Pts',(56.7593104814471,12.025,11.275));
#65270=CARTESIAN_POINT('Origin',(18.,0.,64.));
#65271=CARTESIAN_POINT('',(24.,-11.7,64.));
#65272=CARTESIAN_POINT('',(24.,0.,64.));
#65273=CARTESIAN_POINT('',(24.125,-11.7,64.));
#65274=CARTESIAN_POINT('Origin',(18.,0.,64.));
#65275=CARTESIAN_POINT('',(24.,11.7,64.));
#65276=CARTESIAN_POINT('',(24.125,11.7,64.));
#65277=CARTESIAN_POINT('',(24.,12.,64.));
#65278=CARTESIAN_POINT('',(24.,0.,64.));
#65279=CARTESIAN_POINT('',(24.,12.,64.));
#65280=CARTESIAN_POINT('Origin',(24.0004975859988,0.,56.0004975859988));
#65281=CARTESIAN_POINT('Ctrl Pts',(24.,-11.7,64.));
#65282=CARTESIAN_POINT('Ctrl Pts',(24.5022176904815,-11.7000312390044,64.0000312390044));
#65283=CARTESIAN_POINT('Ctrl Pts',(25.0215928562724,-11.7000605560293,63.9520071546108));
#65284=CARTESIAN_POINT('Ctrl Pts',(26.0547668862757,-11.7001122298415,63.749634158072));
#65285=CARTESIAN_POINT('Ctrl Pts',(26.5685742270846,-11.7001345898519,63.5953285238635));
#65286=CARTESIAN_POINT('Ctrl Pts',(27.5540556052171,-11.7001704995408,63.1872005862129));
#65287=CARTESIAN_POINT('Ctrl Pts',(28.0265144414246,-11.7001840778188,62.9330532656189));
#65288=CARTESIAN_POINT('Ctrl Pts',(28.9002511996986,-11.7002018897492,62.345696912753));
#65289=CARTESIAN_POINT('Ctrl Pts',(29.3015045180536,-11.7002061195955,62.0124512814371));
#65290=CARTESIAN_POINT('Ctrl Pts',(30.0117917671937,-11.700206125091,61.3022523895444));
#65291=CARTESIAN_POINT('Ctrl Pts',(30.3450873135436,-11.7002019009279,60.901040531463));
#65292=CARTESIAN_POINT('Ctrl Pts',(30.9325523584188,-11.7001841003031,60.0273768495693));
#65293=CARTESIAN_POINT('Ctrl Pts',(31.1867584529271,-11.7001705276473,59.5549496340214));
#65294=CARTESIAN_POINT('Ctrl Pts',(31.5950089854782,-11.700134628742,58.5695190363596));
#65295=CARTESIAN_POINT('Ctrl Pts',(31.7493785383029,-11.7001122739014,58.0557308958014));
#65296=CARTESIAN_POINT('Ctrl Pts',(31.9518800645024,-11.7000606096502,57.0225820498513));
#65297=CARTESIAN_POINT('Ctrl Pts',(31.9999687609956,-11.7000312970161,56.5032128624791));
#65298=CARTESIAN_POINT('Ctrl Pts',(32.0000000206335,-11.7000000412671,56.0006634554817));
#65299=CARTESIAN_POINT('Ctrl Pts',(32.0000000206344,-11.7000000206344,56.0003317314806));
#65300=CARTESIAN_POINT('Ctrl Pts',(32.,-11.7,56.));
#65301=CARTESIAN_POINT('Origin',(24.0004975859988,0.,56.0004975859988));
#65302=CARTESIAN_POINT('Ctrl Pts',(32.,11.7,56.));
#65303=CARTESIAN_POINT('Ctrl Pts',(32.000031241594,11.700031241594,56.5022593219641));
#65304=CARTESIAN_POINT('Ctrl Pts',(31.9519992003628,11.7000605607168,57.0216761760518));
#65305=CARTESIAN_POINT('Ctrl Pts',(31.7495941438916,11.7001122374015,58.0549284493937));
#65306=CARTESIAN_POINT('Ctrl Pts',(31.5952644237359,11.7001345981877,58.5687723493041));
#65307=CARTESIAN_POINT('Ctrl Pts',(31.1870742898692,11.700170507956,59.5543172013999));
#65308=CARTESIAN_POINT('Ctrl Pts',(30.9328887646418,11.7001840855418,60.0268031112652));
#65309=CARTESIAN_POINT('Ctrl Pts',(30.3454454128867,11.7002018946398,60.9005813312616));
#65310=CARTESIAN_POINT('Ctrl Pts',(30.0121509738491,11.7002061223446,61.3018490261509));
#65311=CARTESIAN_POINT('Ctrl Pts',(29.3018490261509,11.7002061223446,62.0121509738491));
#65312=CARTESIAN_POINT('Ctrl Pts',(28.9005813312616,11.7002018946398,62.3454454128867));
#65313=CARTESIAN_POINT('Ctrl Pts',(28.0268031112652,11.7001840855418,62.9328887646418));
#65314=CARTESIAN_POINT('Ctrl Pts',(27.5543172013999,11.700170507956,63.1870742898692));
#65315=CARTESIAN_POINT('Ctrl Pts',(26.5687723493041,11.7001345981878,63.5952644237359));
#65316=CARTESIAN_POINT('Ctrl Pts',(26.0549284493937,11.7001122374015,63.7495941438916));
#65317=CARTESIAN_POINT('Ctrl Pts',(25.0216761760518,11.7000605607168,63.9519992003628));
#65318=CARTESIAN_POINT('Ctrl Pts',(24.5022593219641,11.700031241594,64.000031241594));
#65319=CARTESIAN_POINT('Ctrl Pts',(24.,11.7,64.));
#65320=CARTESIAN_POINT('Origin',(24.0004975859988,12.,56.0004975859988));
#65321=CARTESIAN_POINT('Origin',(25.0000000077377,12.,55.5637382272397));
#65322=CARTESIAN_POINT('Origin',(24.,0.,64.));
#65323=CARTESIAN_POINT('',(24.125,-11.7,64.));
#65324=CARTESIAN_POINT('',(4.72,-4.72,64.));
#65325=CARTESIAN_POINT('',(8.95,-4.72,64.));
#65326=CARTESIAN_POINT('',(4.72,-2.26,64.));
#65327=CARTESIAN_POINT('',(24.125,11.7,64.));
#65328=CARTESIAN_POINT('Origin',(24.,-11.85,56.));
#65329=CARTESIAN_POINT('',(32.,-11.7,56.));
#65330=CARTESIAN_POINT('',(24.,-11.7,64.));
#65331=CARTESIAN_POINT('Origin',(44.,0.,100.));
#65332=CARTESIAN_POINT('',(32.,-12.,100.));
#65333=CARTESIAN_POINT('Origin',(44.,-12.,100.));
#65334=CARTESIAN_POINT('',(32.,-11.7,100.));
#65335=CARTESIAN_POINT('',(32.,0.,100.));
#65336=CARTESIAN_POINT('Origin',(44.,-11.7,100.));
#65337=CARTESIAN_POINT('Origin',(32.,0.,100.));
#65338=CARTESIAN_POINT('',(32.,-11.7,97.));
#65339=CARTESIAN_POINT('',(32.,-11.7,79.25));
#65340=CARTESIAN_POINT('',(32.,-12.,97.));
#65341=CARTESIAN_POINT('',(32.,-12.,97.));
#65342=CARTESIAN_POINT('',(32.,0.,97.));
#65343=CARTESIAN_POINT('Origin',(32.,0.,100.));
#65344=CARTESIAN_POINT('',(32.,11.7,97.));
#65345=CARTESIAN_POINT('',(32.,11.7,79.25));
#65346=CARTESIAN_POINT('',(32.,12.,97.));
#65347=CARTESIAN_POINT('',(32.,0.,97.));
#65348=CARTESIAN_POINT('',(32.,12.,97.));
#65349=CARTESIAN_POINT('Origin',(27.,0.,92.));
#65350=CARTESIAN_POINT('',(4.72,4.72,92.));
#65351=CARTESIAN_POINT('',(-0.74,4.72,92.));
#65352=CARTESIAN_POINT('',(4.72,-4.72,92.));
#65353=CARTESIAN_POINT('',(4.72,-2.26,92.));
#65354=CARTESIAN_POINT('',(-6.05,-4.72,92.));
#65355=CARTESIAN_POINT('Origin',(27.,0.,92.));
#65356=CARTESIAN_POINT('',(27.,-11.7,92.));
#65357=CARTESIAN_POINT('',(9.125,-11.7,92.));
#65358=CARTESIAN_POINT('',(27.,-12.,92.));
#65359=CARTESIAN_POINT('',(27.,0.,92.));
#65360=CARTESIAN_POINT('',(-6.,-12.,92.));
#65361=CARTESIAN_POINT('',(-6.,-12.,92.));
#65362=CARTESIAN_POINT('',(-6.,0.,92.));
#65363=CARTESIAN_POINT('Origin',(27.,0.,92.));
#65364=CARTESIAN_POINT('',(-6.,11.7,92.));
#65365=CARTESIAN_POINT('',(27.,11.7,92.));
#65366=CARTESIAN_POINT('',(9.125,11.7,92.));
#65367=CARTESIAN_POINT('',(-6.,12.,92.));
#65368=CARTESIAN_POINT('',(-6.,0.,92.));
#65369=CARTESIAN_POINT('',(27.,12.,92.));
#65370=CARTESIAN_POINT('',(-6.,12.,92.));
#65371=CARTESIAN_POINT('',(27.,0.,92.));
#65372=CARTESIAN_POINT('Origin',(-5.9999073877354,0.,87.9999073877354));
#65373=CARTESIAN_POINT('Origin',(-5.9999073877354,-12.,87.9999073877354));
#65374=CARTESIAN_POINT('Origin',(18.5190608795662,-12.,105.));
#65375=CARTESIAN_POINT('Origin',(26.9998842346692,-12.,97.0001157653307));
#65376=CARTESIAN_POINT('Origin',(-5.9999073877354,0.,87.9999073877354));
#65377=CARTESIAN_POINT('Origin',(-5.9999073877354,12.,87.9999073877354));
#65378=CARTESIAN_POINT('Ctrl Pts',(-8.42436827442023,11.7000371816705,91.1815312379424));
#65379=CARTESIAN_POINT('Ctrl Pts',(-8.36188086740803,11.7000368373637,91.2291478894839));
#65380=CARTESIAN_POINT('Ctrl Pts',(-8.29762358003265,11.7000364158445,91.2751995818108));
#65381=CARTESIAN_POINT('Ctrl Pts',(-8.013329790593,11.7000342590358,91.4663398648887));
#65382=CARTESIAN_POINT('Ctrl Pts',(-7.77709609606059,11.7000317321777,91.5934374252052));
#65383=CARTESIAN_POINT('Ctrl Pts',(-7.28434258369623,11.7000250491913,91.7975492958902));
#65384=CARTESIAN_POINT('Ctrl Pts',(-7.02743037635763,11.7000208877413,91.8747261446359));
#65385=CARTESIAN_POINT('Ctrl Pts',(-6.51082246976743,11.700011270506,91.9759594082611));
#65386=CARTESIAN_POINT('Ctrl Pts',(-6.25112253076428,11.700005814122,91.999994185878));
#65387=CARTESIAN_POINT('Ctrl Pts',(-5.99999999999999,11.7,92.));
#65388=CARTESIAN_POINT('Origin',(26.9998842346692,0.,97.0001157653307));
#65389=CARTESIAN_POINT('',(27.,0.,92.));
#65390=CARTESIAN_POINT('Origin',(26.9998842346692,12.,97.0001157653307));
#65391=CARTESIAN_POINT('',(32.,0.,97.));
#65392=CARTESIAN_POINT('Origin',(18.5190608795662,12.,105.));
#65393=CARTESIAN_POINT('Origin',(-5.99999999999999,11.85,88.));
#65394=CARTESIAN_POINT('',(-6.,11.7,92.));
#65395=CARTESIAN_POINT('Origin',(-0.74,4.62,91.9));
#65396=CARTESIAN_POINT('',(4.52,4.52,91.8));
#65397=CARTESIAN_POINT('Origin',(32.,0.,27.4736520332184));
#65398=CARTESIAN_POINT('',(32.,-11.7,19.));
#65399=CARTESIAN_POINT('',(32.,0.,19.));
#65400=CARTESIAN_POINT('',(32.,-11.7,40.25));
#65401=CARTESIAN_POINT('Origin',(32.,0.,27.4736520332184));
#65402=CARTESIAN_POINT('',(32.,11.7,19.));
#65403=CARTESIAN_POINT('',(32.,11.7,40.25));
#65404=CARTESIAN_POINT('',(32.,12.,19.));
#65405=CARTESIAN_POINT('',(32.,0.,19.));
#65406=CARTESIAN_POINT('',(32.,12.,19.));
#65407=CARTESIAN_POINT('Origin',(24.0004975859988,0.,18.9995024140012));
#65408=CARTESIAN_POINT('',(27.0397667852433,-11.7001517572237,11.5998482427763));
#65409=CARTESIAN_POINT('Origin',(24.0004975859988,-4.3004975859987,18.9995024140012));
#65410=CARTESIAN_POINT('Ctrl Pts',(32.,-11.7,19.));
#65411=CARTESIAN_POINT('Ctrl Pts',(32.0000312390044,-11.7000312390044,18.4977823095185));
#65412=CARTESIAN_POINT('Ctrl Pts',(31.9520071546108,-11.7000605560293,17.9784071437276));
#65413=CARTESIAN_POINT('Ctrl Pts',(31.749634158072,-11.7001122298415,16.9452331137243));
#65414=CARTESIAN_POINT('Ctrl Pts',(31.5953285238635,-11.7001345898519,16.4314257729154));
#65415=CARTESIAN_POINT('Ctrl Pts',(31.1872005862129,-11.7001704995408,15.4459443947829));
#65416=CARTESIAN_POINT('Ctrl Pts',(30.9330532656189,-11.7001840778189,14.9734855585754));
#65417=CARTESIAN_POINT('Ctrl Pts',(30.345696912753,-11.7002018897492,14.0997488003014));
#65418=CARTESIAN_POINT('Ctrl Pts',(30.0124512814371,-11.7002061195955,13.6984954819464));
#65419=CARTESIAN_POINT('Ctrl Pts',(29.3022523895444,-11.700206125091,12.9882082328063));
#65420=CARTESIAN_POINT('Ctrl Pts',(28.901040531463,-11.7002019009279,12.6549126864564));
#65421=CARTESIAN_POINT('Ctrl Pts',(28.0273768495693,-11.7001841003031,12.0674476415812));
#65422=CARTESIAN_POINT('Ctrl Pts',(27.5549496340214,-11.7001705276473,11.8132415470729));
#65423=CARTESIAN_POINT('Ctrl Pts',(27.0547499335288,-11.7001523055404,11.6060155946897));
#65424=CARTESIAN_POINT('Ctrl Pts',(27.0472607306568,-11.7001520318827,11.6029262403352));
#65425=CARTESIAN_POINT('Ctrl Pts',(27.0397667852433,-11.7001517572237,11.5998482427763));
#65426=CARTESIAN_POINT('Origin',(24.0004975859988,0.,18.9995024140012));
#65427=CARTESIAN_POINT('',(26.1706823007161,12.,11.3));
#65428=CARTESIAN_POINT('',(27.0397667852433,11.7001517572237,11.5998482427763));
#65429=CARTESIAN_POINT('Origin',(24.0004975859988,4.3004975859987,18.9995024140012));
#65430=CARTESIAN_POINT('Origin',(24.0004975859988,12.,18.9995024140012));
#65431=CARTESIAN_POINT('Ctrl Pts',(27.0397667852433,11.7001517572237,11.5998482427763));
#65432=CARTESIAN_POINT('Ctrl Pts',(27.0470305895134,11.7001520234479,11.602831714176));
#65433=CARTESIAN_POINT('Ctrl Pts',(27.0542899373568,11.7001522887312,11.6058258552508));
#65434=CARTESIAN_POINT('Ctrl Pts',(27.5543172013999,11.700170507956,11.8129257101308));
#65435=CARTESIAN_POINT('Ctrl Pts',(28.0268031112652,11.7001840855418,12.0671112353582));
#65436=CARTESIAN_POINT('Ctrl Pts',(28.9005813312616,11.7002018946398,12.6545545871133));
#65437=CARTESIAN_POINT('Ctrl Pts',(29.3018490261509,11.7002061223446,12.9878490261509));
#65438=CARTESIAN_POINT('Ctrl Pts',(30.0121509738491,11.7002061223446,13.6981509738491));
#65439=CARTESIAN_POINT('Ctrl Pts',(30.3454454128867,11.7002018946398,14.0994186687384));
#65440=CARTESIAN_POINT('Ctrl Pts',(30.9328887646418,11.7001840855418,14.9731968887348));
#65441=CARTESIAN_POINT('Ctrl Pts',(31.1870742898692,11.700170507956,15.4456827986001));
#65442=CARTESIAN_POINT('Ctrl Pts',(31.5952644237359,11.7001345981877,16.4312276506959));
#65443=CARTESIAN_POINT('Ctrl Pts',(31.7495941438916,11.7001122374015,16.9450715506063));
#65444=CARTESIAN_POINT('Ctrl Pts',(31.9519992003628,11.7000605607168,17.9783238239482));
#65445=CARTESIAN_POINT('Ctrl Pts',(32.000031241594,11.700031241594,18.4977406780359));
#65446=CARTESIAN_POINT('Ctrl Pts',(32.,11.7,19.));
#65447=CARTESIAN_POINT('Origin',(2.98958333333334,0.,37.3005642361111));
#65448=CARTESIAN_POINT('',(32.,0.,27.4736520332184));
#65449=CARTESIAN_POINT('Origin',(28.5000000077377,12.,19.2681696700813));
#65450=CARTESIAN_POINT('',(26.1875000038689,12.,11.3));
#65451=CARTESIAN_POINT('Origin',(23.875,12.15,11.15));
#65452=CARTESIAN_POINT('',(27.0983866769659,12.,11.3));
#65453=CARTESIAN_POINT('Ctrl Pts',(27.0397667852433,11.7001517572237,11.5998482427763));
#65454=CARTESIAN_POINT('Ctrl Pts',(27.0690767311041,11.8486440903987,11.4513559096013));
#65455=CARTESIAN_POINT('Ctrl Pts',(27.0983866769659,12.,11.3));
#65456=CARTESIAN_POINT('Ctrl Pts',(27.0983866769659,12.,11.3));
#65457=CARTESIAN_POINT('Ctrl Pts',(27.1187918891661,12.1053720627028,11.1946279372972));
#65458=CARTESIAN_POINT('Ctrl Pts',(27.1391971013664,12.212132034356,11.087867965644));
#65459=CARTESIAN_POINT('Origin',(24.,11.85,19.));
#65460=CARTESIAN_POINT('',(32.,11.7,19.));
#65461=CARTESIAN_POINT('Origin',(32.,0.,19.));
#65462=CARTESIAN_POINT('',(32.,11.7,40.25));
#65463=CARTESIAN_POINT('',(32.,-11.7,40.25));
#65464=CARTESIAN_POINT('Origin',(54.3509571552277,-12.,80.3999996185303));
#65465=CARTESIAN_POINT('',(54.3509571552277,-12.4,86.7057294845581));
#65466=CARTESIAN_POINT('',(54.3509571552277,-12.,86.7057294845581));
#65467=CARTESIAN_POINT('',(54.3509571552277,-12.4,80.3999996185303));
#65468=CARTESIAN_POINT('',(54.3509571552277,-12.4,86.7057294845581));
#65469=CARTESIAN_POINT('',(54.3509571552277,-12.,80.3999996185303));
#65470=CARTESIAN_POINT('Origin',(52.6085274219513,-12.,80.3999996185303));
#65471=CARTESIAN_POINT('',(52.6085274219513,-12.4,80.3999996185303));
#65472=CARTESIAN_POINT('',(54.3509571552277,-12.4,80.3999996185303));
#65473=CARTESIAN_POINT('',(52.6085274219513,-12.,80.3999996185303));
#65474=CARTESIAN_POINT('Origin',(52.6085274219513,-12.,84.5319232940674));
#65475=CARTESIAN_POINT('',(52.6085274219513,-12.4,84.5319232940674));
#65476=CARTESIAN_POINT('',(52.6085274219513,-12.4,80.3999996185303));
#65477=CARTESIAN_POINT('',(52.6085274219513,-12.,84.5319232940674));
#65478=CARTESIAN_POINT('Ctrl Pts',(51.7901794910431,-12.,84.0117321014404));
#65479=CARTESIAN_POINT('Ctrl Pts',(51.7901794910431,-12.4,84.0117321014404));
#65480=CARTESIAN_POINT('Ctrl Pts',(52.1856091022491,-12.,84.2105045318604));
#65481=CARTESIAN_POINT('Ctrl Pts',(52.1856091022491,-12.4,84.2105045318604));
#65482=CARTESIAN_POINT('Ctrl Pts',(52.6085274219513,-12.,84.5319232940674));
#65483=CARTESIAN_POINT('Ctrl Pts',(52.6085274219513,-12.4,84.5319232940674));
#65484=CARTESIAN_POINT('',(51.7901794910431,-12.4,84.0117321014404));
#65485=CARTESIAN_POINT('Ctrl Pts',(51.7901794910431,-12.4,84.0117321014404));
#65486=CARTESIAN_POINT('Ctrl Pts',(52.1856091022491,-12.4,84.2105045318604));
#65487=CARTESIAN_POINT('Ctrl Pts',(52.6085274219513,-12.4,84.5319232940674));
#65488=CARTESIAN_POINT('',(51.7901794910431,-12.,84.0117321014404));
#65489=CARTESIAN_POINT('Ctrl Pts',(50.7984325885773,-12.,83.6311044692993));
#65490=CARTESIAN_POINT('Ctrl Pts',(50.7984325885773,-12.4,83.6311044692993));
#65491=CARTESIAN_POINT('Ctrl Pts',(51.394749879837,-12.,83.8129596710205));
#65492=CARTESIAN_POINT('Ctrl Pts',(51.394749879837,-12.4,83.8129596710205));
#65493=CARTESIAN_POINT('Ctrl Pts',(51.7901794910431,-12.,84.0117321014404));
#65494=CARTESIAN_POINT('Ctrl Pts',(51.7901794910431,-12.4,84.0117321014404));
#65495=CARTESIAN_POINT('',(50.7984325885773,-12.4,83.6311044692993));
#65496=CARTESIAN_POINT('Ctrl Pts',(50.7984325885773,-12.4,83.6311044692993));
#65497=CARTESIAN_POINT('Ctrl Pts',(51.394749879837,-12.4,83.8129596710205));
#65498=CARTESIAN_POINT('Ctrl Pts',(51.7901794910431,-12.4,84.0117321014404));
#65499=CARTESIAN_POINT('',(50.7984325885773,-12.,83.6311044692993));
#65500=CARTESIAN_POINT('Origin',(50.7984325885773,-12.,85.0436553955078));
#65501=CARTESIAN_POINT('',(50.7984325885773,-12.4,85.0436553955078));
#65502=CARTESIAN_POINT('',(50.7984325885773,-12.4,83.6311044692993));
#65503=CARTESIAN_POINT('',(50.7984325885773,-12.,85.0436553955078));
#65504=CARTESIAN_POINT('Ctrl Pts',(52.1644623279572,-12.,85.7245559692383));
#65505=CARTESIAN_POINT('Ctrl Pts',(52.1644623279572,-12.4,85.7245559692383));
#65506=CARTESIAN_POINT('Ctrl Pts',(51.6781055927277,-12.,85.3270111083984));
#65507=CARTESIAN_POINT('Ctrl Pts',(51.6781055927277,-12.4,85.3270111083984));
#65508=CARTESIAN_POINT('Ctrl Pts',(50.7984325885773,-12.,85.0436553955078));
#65509=CARTESIAN_POINT('Ctrl Pts',(50.7984325885773,-12.4,85.0436553955078));
#65510=CARTESIAN_POINT('',(52.1644623279572,-12.4,85.7245559692383));
#65511=CARTESIAN_POINT('Ctrl Pts',(52.1644623279572,-12.4,85.7245559692383));
#65512=CARTESIAN_POINT('Ctrl Pts',(51.6781055927277,-12.4,85.3270111083984));
#65513=CARTESIAN_POINT('Ctrl Pts',(50.7984325885773,-12.4,85.0436553955078));
#65514=CARTESIAN_POINT('',(52.1644623279572,-12.,85.7245559692383));
#65515=CARTESIAN_POINT('Ctrl Pts',(52.9257175922394,-12.,86.7057294845581));
#65516=CARTESIAN_POINT('Ctrl Pts',(52.9257175922394,-12.4,86.7057294845581));
#65517=CARTESIAN_POINT('Ctrl Pts',(52.6508209705353,-12.,86.122100353241));
#65518=CARTESIAN_POINT('Ctrl Pts',(52.6508209705353,-12.4,86.122100353241));
#65519=CARTESIAN_POINT('Ctrl Pts',(52.1644623279572,-12.,85.7245559692383));
#65520=CARTESIAN_POINT('Ctrl Pts',(52.1644623279572,-12.4,85.7245559692383));
#65521=CARTESIAN_POINT('',(52.9257175922394,-12.4,86.7057294845581));
#65522=CARTESIAN_POINT('Ctrl Pts',(52.9257175922394,-12.4,86.7057294845581));
#65523=CARTESIAN_POINT('Ctrl Pts',(52.6508209705353,-12.4,86.122100353241));
#65524=CARTESIAN_POINT('Ctrl Pts',(52.1644623279572,-12.4,85.7245559692383));
#65525=CARTESIAN_POINT('',(52.9257175922394,-12.,86.7057294845581));
#65526=CARTESIAN_POINT('Origin',(54.3509571552277,-12.,86.7057294845581));
#65527=CARTESIAN_POINT('',(52.9257175922394,-12.4,86.7057294845581));
#65528=CARTESIAN_POINT('Origin',(52.5746948719025,-12.4,83.5528645515442));
#65529=CARTESIAN_POINT('Origin',(35.4379951953888,-12.,86.5999994277954));
#65530=CARTESIAN_POINT('',(33.6490461826324,-12.4,86.5999994277954));
#65531=CARTESIAN_POINT('',(33.6490461826324,-12.,86.5999994277954));
#65532=CARTESIAN_POINT('',(35.4379951953888,-12.4,86.5999994277954));
#65533=CARTESIAN_POINT('',(33.6490461826324,-12.4,86.5999994277954));
#65534=CARTESIAN_POINT('',(35.4379951953888,-12.,86.5999994277954));
#65535=CARTESIAN_POINT('Origin',(37.772510766983,-12.,83.1698579788208));
#65536=CARTESIAN_POINT('',(37.772510766983,-12.4,83.1698579788208));
#65537=CARTESIAN_POINT('',(35.4379951953888,-12.4,86.5999994277954));
#65538=CARTESIAN_POINT('',(37.772510766983,-12.,83.1698579788208));
#65539=CARTESIAN_POINT('Origin',(37.772510766983,-12.,86.5999994277954));
#65540=CARTESIAN_POINT('',(37.772510766983,-12.4,86.5999994277954));
#65541=CARTESIAN_POINT('',(37.772510766983,-12.4,83.1698579788208));
#65542=CARTESIAN_POINT('',(37.772510766983,-12.,86.5999994277954));
#65543=CARTESIAN_POINT('Origin',(39.5783770084381,-12.,86.5999994277954));
#65544=CARTESIAN_POINT('',(39.5783770084381,-12.4,86.5999994277954));
#65545=CARTESIAN_POINT('',(37.772510766983,-12.4,86.5999994277954));
#65546=CARTESIAN_POINT('',(39.5783770084381,-12.,86.5999994277954));
#65547=CARTESIAN_POINT('Origin',(39.5783770084381,-12.,80.3999996185303));
#65548=CARTESIAN_POINT('',(39.5783770084381,-12.4,80.3999996185303));
#65549=CARTESIAN_POINT('',(39.5783770084381,-12.4,86.5999994277954));
#65550=CARTESIAN_POINT('',(39.5783770084381,-12.,80.3999996185303));
#65551=CARTESIAN_POINT('Origin',(37.772510766983,-12.,80.3999996185303));
#65552=CARTESIAN_POINT('',(37.772510766983,-12.4,80.3999996185303));
#65553=CARTESIAN_POINT('',(39.5783770084381,-12.4,80.3999996185303));
#65554=CARTESIAN_POINT('',(37.772510766983,-12.,80.3999996185303));
#65555=CARTESIAN_POINT('Origin',(35.4506828784943,-12.,83.8042373657227));
#65556=CARTESIAN_POINT('',(35.4506828784943,-12.4,83.8042373657227));
#65557=CARTESIAN_POINT('',(37.772510766983,-12.4,80.3999996185303));
#65558=CARTESIAN_POINT('',(35.4506828784943,-12.,83.8042373657227));
#65559=CARTESIAN_POINT('Origin',(35.4506828784943,-12.,80.3999996185303));
#65560=CARTESIAN_POINT('',(35.4506828784943,-12.4,80.3999996185303));
#65561=CARTESIAN_POINT('',(35.4506828784943,-12.4,83.8042373657227));
#65562=CARTESIAN_POINT('',(35.4506828784943,-12.,80.3999996185303));
#65563=CARTESIAN_POINT('Origin',(33.6490461826324,-12.,80.3999996185303));
#65564=CARTESIAN_POINT('',(33.6490461826324,-12.4,80.3999996185303));
#65565=CARTESIAN_POINT('',(35.4506828784943,-12.4,80.3999996185303));
#65566=CARTESIAN_POINT('',(33.6490461826324,-12.,80.3999996185303));
#65567=CARTESIAN_POINT('Origin',(33.6490461826324,-12.,86.5999994277954));
#65568=CARTESIAN_POINT('',(33.6490461826324,-12.4,80.3999996185303));
#65569=CARTESIAN_POINT('Origin',(36.6137115955353,-12.4,83.4999995231628));
#65570=CARTESIAN_POINT('Ctrl Pts',(42.5261261463165,-12.,83.4873123168945));
#65571=CARTESIAN_POINT('Ctrl Pts',(42.5261261463165,-12.4,83.4873123168945));
#65572=CARTESIAN_POINT('Ctrl Pts',(42.5261261463165,-12.,84.4346513748169));
#65573=CARTESIAN_POINT('Ctrl Pts',(42.5261261463165,-12.4,84.4346513748169));
#65574=CARTESIAN_POINT('Ctrl Pts',(42.8771488666534,-12.,84.8448829650879));
#65575=CARTESIAN_POINT('Ctrl Pts',(42.8771488666534,-12.4,84.8448829650879));
#65576=CARTESIAN_POINT('',(42.8771488666534,-12.,84.8448829650879));
#65577=CARTESIAN_POINT('',(42.5261261463165,-12.,83.4873123168945));
#65578=CARTESIAN_POINT('Ctrl Pts',(42.8771488666534,-12.,84.8448829650879));
#65579=CARTESIAN_POINT('Ctrl Pts',(42.5261261463165,-12.,84.4346513748169));
#65580=CARTESIAN_POINT('Ctrl Pts',(42.5261261463165,-12.,83.4873123168945));
#65581=CARTESIAN_POINT('',(42.8771488666534,-12.4,84.8448829650879));
#65582=CARTESIAN_POINT('',(42.8771488666534,-12.,84.8448829650879));
#65583=CARTESIAN_POINT('',(42.5261261463165,-12.4,83.4873123168945));
#65584=CARTESIAN_POINT('Ctrl Pts',(42.5261261463165,-12.4,83.4873123168945));
#65585=CARTESIAN_POINT('Ctrl Pts',(42.5261261463165,-12.4,84.4346513748169));
#65586=CARTESIAN_POINT('Ctrl Pts',(42.8771488666534,-12.4,84.8448829650879));
#65587=CARTESIAN_POINT('',(42.5261261463165,-12.,83.4873123168945));
#65588=CARTESIAN_POINT('Ctrl Pts',(42.875034570694,-12.,82.1381988525391));
#65589=CARTESIAN_POINT('Ctrl Pts',(42.875034570694,-12.4,82.1381988525391));
#65590=CARTESIAN_POINT('Ctrl Pts',(42.5261261463165,-12.,82.5484304428101));
#65591=CARTESIAN_POINT('Ctrl Pts',(42.5261261463165,-12.4,82.5484304428101));
#65592=CARTESIAN_POINT('Ctrl Pts',(42.5261261463165,-12.,83.4873123168945));
#65593=CARTESIAN_POINT('Ctrl Pts',(42.5261261463165,-12.4,83.4873123168945));
#65594=CARTESIAN_POINT('',(42.875034570694,-12.,82.1381988525391));
#65595=CARTESIAN_POINT('Ctrl Pts',(42.5261261463165,-12.,83.4873123168945));
#65596=CARTESIAN_POINT('Ctrl Pts',(42.5261261463165,-12.,82.5484304428101));
#65597=CARTESIAN_POINT('Ctrl Pts',(42.875034570694,-12.,82.1381988525391));
#65598=CARTESIAN_POINT('',(42.875034570694,-12.4,82.1381988525391));
#65599=CARTESIAN_POINT('Ctrl Pts',(42.875034570694,-12.4,82.1381988525391));
#65600=CARTESIAN_POINT('Ctrl Pts',(42.5261261463165,-12.4,82.5484304428101));
#65601=CARTESIAN_POINT('Ctrl Pts',(42.5261261463165,-12.4,83.4873123168945));
#65602=CARTESIAN_POINT('',(42.875034570694,-12.,82.1381988525391));
#65603=CARTESIAN_POINT('Ctrl Pts',(43.8244888782501,-12.,81.7279672622681));
#65604=CARTESIAN_POINT('Ctrl Pts',(43.8244888782501,-12.4,81.7279672622681));
#65605=CARTESIAN_POINT('Ctrl Pts',(43.2239429950714,-12.,81.7279672622681));
#65606=CARTESIAN_POINT('Ctrl Pts',(43.2239429950714,-12.4,81.7279672622681));
#65607=CARTESIAN_POINT('Ctrl Pts',(42.875034570694,-12.,82.1381988525391));
#65608=CARTESIAN_POINT('Ctrl Pts',(42.875034570694,-12.4,82.1381988525391));
#65609=CARTESIAN_POINT('',(43.8244888782501,-12.,81.7279672622681));
#65610=CARTESIAN_POINT('Ctrl Pts',(42.875034570694,-12.,82.1381988525391));
#65611=CARTESIAN_POINT('Ctrl Pts',(43.2239429950714,-12.,81.7279672622681));
#65612=CARTESIAN_POINT('Ctrl Pts',(43.8244888782501,-12.,81.7279672622681));
#65613=CARTESIAN_POINT('',(43.8244888782501,-12.4,81.7279672622681));
#65614=CARTESIAN_POINT('Ctrl Pts',(43.8244888782501,-12.4,81.7279672622681));
#65615=CARTESIAN_POINT('Ctrl Pts',(43.2239429950714,-12.4,81.7279672622681));
#65616=CARTESIAN_POINT('Ctrl Pts',(42.875034570694,-12.4,82.1381988525391));
#65617=CARTESIAN_POINT('',(43.8244888782501,-12.,81.7279672622681));
#65618=CARTESIAN_POINT('Ctrl Pts',(44.780287027359,-12.,82.1297407150269));
#65619=CARTESIAN_POINT('Ctrl Pts',(44.780287027359,-12.4,82.1297407150269));
#65620=CARTESIAN_POINT('Ctrl Pts',(44.4419510364532,-12.,81.7279672622681));
#65621=CARTESIAN_POINT('Ctrl Pts',(44.4419510364532,-12.4,81.7279672622681));
#65622=CARTESIAN_POINT('Ctrl Pts',(43.8244888782501,-12.,81.7279672622681));
#65623=CARTESIAN_POINT('Ctrl Pts',(43.8244888782501,-12.4,81.7279672622681));
#65624=CARTESIAN_POINT('',(44.780287027359,-12.,82.1297407150269));
#65625=CARTESIAN_POINT('Ctrl Pts',(43.8244888782501,-12.,81.7279672622681));
#65626=CARTESIAN_POINT('Ctrl Pts',(44.4419510364532,-12.,81.7279672622681));
#65627=CARTESIAN_POINT('Ctrl Pts',(44.780287027359,-12.,82.1297407150269));
#65628=CARTESIAN_POINT('',(44.780287027359,-12.4,82.1297407150269));
#65629=CARTESIAN_POINT('Ctrl Pts',(44.780287027359,-12.4,82.1297407150269));
#65630=CARTESIAN_POINT('Ctrl Pts',(44.4419510364532,-12.4,81.7279672622681));
#65631=CARTESIAN_POINT('Ctrl Pts',(43.8244888782501,-12.4,81.7279672622681));
#65632=CARTESIAN_POINT('',(44.780287027359,-12.,82.1297407150269));
#65633=CARTESIAN_POINT('Ctrl Pts',(45.1186230182648,-12.,83.5718955993652));
#65634=CARTESIAN_POINT('Ctrl Pts',(45.1186230182648,-12.4,83.5718955993652));
#65635=CARTESIAN_POINT('Ctrl Pts',(45.1186230182648,-12.,82.5315141677856));
#65636=CARTESIAN_POINT('Ctrl Pts',(45.1186230182648,-12.4,82.5315141677856));
#65637=CARTESIAN_POINT('Ctrl Pts',(44.780287027359,-12.,82.1297407150269));
#65638=CARTESIAN_POINT('Ctrl Pts',(44.780287027359,-12.4,82.1297407150269));
#65639=CARTESIAN_POINT('',(45.1186230182648,-12.,83.5718955993652));
#65640=CARTESIAN_POINT('Ctrl Pts',(44.780287027359,-12.,82.1297407150269));
#65641=CARTESIAN_POINT('Ctrl Pts',(45.1186230182648,-12.,82.5315141677856));
#65642=CARTESIAN_POINT('Ctrl Pts',(45.1186230182648,-12.,83.5718955993652));
#65643=CARTESIAN_POINT('',(45.1186230182648,-12.4,83.5718955993652));
#65644=CARTESIAN_POINT('Ctrl Pts',(45.1186230182648,-12.4,83.5718955993652));
#65645=CARTESIAN_POINT('Ctrl Pts',(45.1186230182648,-12.4,82.5315141677856));
#65646=CARTESIAN_POINT('Ctrl Pts',(44.780287027359,-12.4,82.1297407150269));
#65647=CARTESIAN_POINT('',(45.1186230182648,-12.,83.5718955993652));
#65648=CARTESIAN_POINT('Ctrl Pts',(44.7654850482941,-12.,84.8512268066406));
#65649=CARTESIAN_POINT('Ctrl Pts',(44.7654850482941,-12.4,84.8512268066406));
#65650=CARTESIAN_POINT('Ctrl Pts',(45.1186230182648,-12.,84.4473390579224));
#65651=CARTESIAN_POINT('Ctrl Pts',(45.1186230182648,-12.4,84.4473390579224));
#65652=CARTESIAN_POINT('Ctrl Pts',(45.1186230182648,-12.,83.5718955993652));
#65653=CARTESIAN_POINT('Ctrl Pts',(45.1186230182648,-12.4,83.5718955993652));
#65654=CARTESIAN_POINT('',(44.7654850482941,-12.,84.8512268066406));
#65655=CARTESIAN_POINT('Ctrl Pts',(45.1186230182648,-12.,83.5718955993652));
#65656=CARTESIAN_POINT('Ctrl Pts',(45.1186230182648,-12.,84.4473390579224));
#65657=CARTESIAN_POINT('Ctrl Pts',(44.7654850482941,-12.,84.8512268066406));
#65658=CARTESIAN_POINT('',(44.7654850482941,-12.4,84.8512268066406));
#65659=CARTESIAN_POINT('Ctrl Pts',(44.7654850482941,-12.4,84.8512268066406));
#65660=CARTESIAN_POINT('Ctrl Pts',(45.1186230182648,-12.4,84.4473390579224));
#65661=CARTESIAN_POINT('Ctrl Pts',(45.1186230182648,-12.4,83.5718955993652));
#65662=CARTESIAN_POINT('',(44.7654850482941,-12.,84.8512268066406));
#65663=CARTESIAN_POINT('Ctrl Pts',(43.8075726032257,-12.,85.2551155090332));
#65664=CARTESIAN_POINT('Ctrl Pts',(43.8075726032257,-12.4,85.2551155090332));
#65665=CARTESIAN_POINT('Ctrl Pts',(44.4123470783234,-12.,85.2551155090332));
#65666=CARTESIAN_POINT('Ctrl Pts',(44.4123470783234,-12.4,85.2551155090332));
#65667=CARTESIAN_POINT('Ctrl Pts',(44.7654850482941,-12.,84.8512268066406));
#65668=CARTESIAN_POINT('Ctrl Pts',(44.7654850482941,-12.4,84.8512268066406));
#65669=CARTESIAN_POINT('',(43.8075726032257,-12.,85.2551155090332));
#65670=CARTESIAN_POINT('Ctrl Pts',(44.7654850482941,-12.,84.8512268066406));
#65671=CARTESIAN_POINT('Ctrl Pts',(44.4123470783234,-12.,85.2551155090332));
#65672=CARTESIAN_POINT('Ctrl Pts',(43.8075726032257,-12.,85.2551155090332));
#65673=CARTESIAN_POINT('',(43.8075726032257,-12.4,85.2551155090332));
#65674=CARTESIAN_POINT('Ctrl Pts',(43.8075726032257,-12.4,85.2551155090332));
#65675=CARTESIAN_POINT('Ctrl Pts',(44.4123470783234,-12.4,85.2551155090332));
#65676=CARTESIAN_POINT('Ctrl Pts',(44.7654850482941,-12.4,84.8512268066406));
#65677=CARTESIAN_POINT('',(43.8075726032257,-12.,85.2551155090332));
#65678=CARTESIAN_POINT('Ctrl Pts',(42.8771488666534,-12.,84.8448829650879));
#65679=CARTESIAN_POINT('Ctrl Pts',(42.8771488666534,-12.4,84.8448829650879));
#65680=CARTESIAN_POINT('Ctrl Pts',(43.2281725406647,-12.,85.2551155090332));
#65681=CARTESIAN_POINT('Ctrl Pts',(43.2281725406647,-12.4,85.2551155090332));
#65682=CARTESIAN_POINT('Ctrl Pts',(43.8075726032257,-12.,85.2551155090332));
#65683=CARTESIAN_POINT('Ctrl Pts',(43.8075726032257,-12.4,85.2551155090332));
#65684=CARTESIAN_POINT('Ctrl Pts',(43.8075726032257,-12.,85.2551155090332));
#65685=CARTESIAN_POINT('Ctrl Pts',(43.2281725406647,-12.,85.2551155090332));
#65686=CARTESIAN_POINT('Ctrl Pts',(42.8771488666534,-12.,84.8448829650879));
#65687=CARTESIAN_POINT('Ctrl Pts',(42.8771488666534,-12.4,84.8448829650879));
#65688=CARTESIAN_POINT('Ctrl Pts',(43.2281725406647,-12.4,85.2551155090332));
#65689=CARTESIAN_POINT('Ctrl Pts',(43.8075726032257,-12.4,85.2551155090332));
#65690=CARTESIAN_POINT('Ctrl Pts',(41.4561398029327,-12.,85.8598899841309));
#65691=CARTESIAN_POINT('Ctrl Pts',(41.4561398029327,-12.4,85.8598899841309));
#65692=CARTESIAN_POINT('Ctrl Pts',(40.6103012561798,-12.,85.0140514373779));
#65693=CARTESIAN_POINT('Ctrl Pts',(40.6103012561798,-12.4,85.0140514373779));
#65694=CARTESIAN_POINT('Ctrl Pts',(40.6103012561798,-12.,83.4957704544067));
#65695=CARTESIAN_POINT('Ctrl Pts',(40.6103012561798,-12.4,83.4957704544067));
#65696=CARTESIAN_POINT('',(40.6103012561798,-12.4,83.4957704544067));
#65697=CARTESIAN_POINT('',(40.6103012561798,-12.,83.4957704544067));
#65698=CARTESIAN_POINT('',(41.4561398029327,-12.4,85.8598899841309));
#65699=CARTESIAN_POINT('Ctrl Pts',(41.4561398029327,-12.4,85.8598899841309));
#65700=CARTESIAN_POINT('Ctrl Pts',(40.6103012561798,-12.4,85.0140514373779));
#65701=CARTESIAN_POINT('Ctrl Pts',(40.6103012561798,-12.4,83.4957704544067));
#65702=CARTESIAN_POINT('',(41.4561398029327,-12.,85.8598899841309));
#65703=CARTESIAN_POINT('Ctrl Pts',(43.8118011951447,-12.,86.7057290077209));
#65704=CARTESIAN_POINT('Ctrl Pts',(43.8118011951447,-12.4,86.7057290077209));
#65705=CARTESIAN_POINT('Ctrl Pts',(42.3019783496857,-12.,86.7057290077209));
#65706=CARTESIAN_POINT('Ctrl Pts',(42.3019783496857,-12.4,86.7057290077209));
#65707=CARTESIAN_POINT('Ctrl Pts',(41.4561398029327,-12.,85.8598899841309));
#65708=CARTESIAN_POINT('Ctrl Pts',(41.4561398029327,-12.4,85.8598899841309));
#65709=CARTESIAN_POINT('',(43.8118011951447,-12.4,86.7057290077209));
#65710=CARTESIAN_POINT('Ctrl Pts',(43.8118011951447,-12.4,86.7057290077209));
#65711=CARTESIAN_POINT('Ctrl Pts',(42.3019783496857,-12.4,86.7057290077209));
#65712=CARTESIAN_POINT('Ctrl Pts',(41.4561398029327,-12.4,85.8598899841309));
#65713=CARTESIAN_POINT('',(43.8118011951447,-12.,86.7057290077209));
#65714=CARTESIAN_POINT('Ctrl Pts',(46.1970684528351,-12.,85.874692440033));
#65715=CARTESIAN_POINT('Ctrl Pts',(46.1970684528351,-12.4,85.874692440033));
#65716=CARTESIAN_POINT('Ctrl Pts',(45.35968708992,-12.,86.7057290077209));
#65717=CARTESIAN_POINT('Ctrl Pts',(45.35968708992,-12.4,86.7057290077209));
#65718=CARTESIAN_POINT('Ctrl Pts',(43.8118011951447,-12.,86.7057290077209));
#65719=CARTESIAN_POINT('Ctrl Pts',(43.8118011951447,-12.4,86.7057290077209));
#65720=CARTESIAN_POINT('',(46.1970684528351,-12.4,85.874692440033));
#65721=CARTESIAN_POINT('Ctrl Pts',(46.1970684528351,-12.4,85.874692440033));
#65722=CARTESIAN_POINT('Ctrl Pts',(45.35968708992,-12.4,86.7057290077209));
#65723=CARTESIAN_POINT('Ctrl Pts',(43.8118011951447,-12.4,86.7057290077209));
#65724=CARTESIAN_POINT('',(46.1970684528351,-12.,85.874692440033));
#65725=CARTESIAN_POINT('Ctrl Pts',(47.0344479084015,-12.,83.5465202331543));
#65726=CARTESIAN_POINT('Ctrl Pts',(47.0344479084015,-12.4,83.5465202331543));
#65727=CARTESIAN_POINT('Ctrl Pts',(47.0344479084015,-12.,85.0436553955078));
#65728=CARTESIAN_POINT('Ctrl Pts',(47.0344479084015,-12.4,85.0436553955078));
#65729=CARTESIAN_POINT('Ctrl Pts',(46.1970684528351,-12.,85.874692440033));
#65730=CARTESIAN_POINT('Ctrl Pts',(46.1970684528351,-12.4,85.874692440033));
#65731=CARTESIAN_POINT('',(47.0344479084015,-12.4,83.5465202331543));
#65732=CARTESIAN_POINT('Ctrl Pts',(47.0344479084015,-12.4,83.5465202331543));
#65733=CARTESIAN_POINT('Ctrl Pts',(47.0344479084015,-12.4,85.0436553955078));
#65734=CARTESIAN_POINT('Ctrl Pts',(46.1970684528351,-12.4,85.874692440033));
#65735=CARTESIAN_POINT('',(47.0344479084015,-12.,83.5465202331543));
#65736=CARTESIAN_POINT('Ctrl Pts',(46.6686222553253,-12.,81.7639150619507));
#65737=CARTESIAN_POINT('Ctrl Pts',(46.6686222553253,-12.4,81.7639150619507));
#65738=CARTESIAN_POINT('Ctrl Pts',(47.0344479084015,-12.,82.4596176147461));
#65739=CARTESIAN_POINT('Ctrl Pts',(47.0344479084015,-12.4,82.4596176147461));
#65740=CARTESIAN_POINT('Ctrl Pts',(47.0344479084015,-12.,83.5465202331543));
#65741=CARTESIAN_POINT('Ctrl Pts',(47.0344479084015,-12.4,83.5465202331543));
#65742=CARTESIAN_POINT('',(46.6686222553253,-12.4,81.7639150619507));
#65743=CARTESIAN_POINT('Ctrl Pts',(46.6686222553253,-12.4,81.7639150619507));
#65744=CARTESIAN_POINT('Ctrl Pts',(47.0344479084015,-12.4,82.4596176147461));
#65745=CARTESIAN_POINT('Ctrl Pts',(47.0344479084015,-12.4,83.5465202331543));
#65746=CARTESIAN_POINT('',(46.6686222553253,-12.,81.7639150619507));
#65747=CARTESIAN_POINT('Ctrl Pts',(45.611323595047,-12.,80.6812410354614));
#65748=CARTESIAN_POINT('Ctrl Pts',(45.611323595047,-12.4,80.6812410354614));
#65749=CARTESIAN_POINT('Ctrl Pts',(46.3027966022491,-12.,81.0682125091553));
#65750=CARTESIAN_POINT('Ctrl Pts',(46.3027966022491,-12.4,81.0682125091553));
#65751=CARTESIAN_POINT('Ctrl Pts',(46.6686222553253,-12.,81.7639150619507));
#65752=CARTESIAN_POINT('Ctrl Pts',(46.6686222553253,-12.4,81.7639150619507));
#65753=CARTESIAN_POINT('',(45.611323595047,-12.4,80.6812410354614));
#65754=CARTESIAN_POINT('Ctrl Pts',(45.611323595047,-12.4,80.6812410354614));
#65755=CARTESIAN_POINT('Ctrl Pts',(46.3027966022491,-12.4,81.0682125091553));
#65756=CARTESIAN_POINT('Ctrl Pts',(46.6686222553253,-12.4,81.7639150619507));
#65757=CARTESIAN_POINT('',(45.611323595047,-12.,80.6812410354614));
#65758=CARTESIAN_POINT('Ctrl Pts',(43.8879272937775,-12.,80.2942695617676));
#65759=CARTESIAN_POINT('Ctrl Pts',(43.8879272937775,-12.4,80.2942695617676));
#65760=CARTESIAN_POINT('Ctrl Pts',(44.9198505878448,-12.,80.2942695617676));
#65761=CARTESIAN_POINT('Ctrl Pts',(44.9198505878448,-12.4,80.2942695617676));
#65762=CARTESIAN_POINT('Ctrl Pts',(45.611323595047,-12.,80.6812410354614));
#65763=CARTESIAN_POINT('Ctrl Pts',(45.611323595047,-12.4,80.6812410354614));
#65764=CARTESIAN_POINT('',(43.8879272937775,-12.4,80.2942695617676));
#65765=CARTESIAN_POINT('Ctrl Pts',(43.8879272937775,-12.4,80.2942695617676));
#65766=CARTESIAN_POINT('Ctrl Pts',(44.9198505878448,-12.4,80.2942695617676));
#65767=CARTESIAN_POINT('Ctrl Pts',(45.611323595047,-12.4,80.6812410354614));
#65768=CARTESIAN_POINT('',(43.8879272937775,-12.,80.2942695617676));
#65769=CARTESIAN_POINT('Ctrl Pts',(42.1518423557281,-12.,80.6283760070801));
#65770=CARTESIAN_POINT('Ctrl Pts',(42.1518423557281,-12.4,80.6283760070801));
#65771=CARTESIAN_POINT('Ctrl Pts',(42.8390867710114,-12.,80.2942695617676));
#65772=CARTESIAN_POINT('Ctrl Pts',(42.8390867710114,-12.4,80.2942695617676));
#65773=CARTESIAN_POINT('Ctrl Pts',(43.8879272937775,-12.,80.2942695617676));
#65774=CARTESIAN_POINT('Ctrl Pts',(43.8879272937775,-12.4,80.2942695617676));
#65775=CARTESIAN_POINT('',(42.1518423557281,-12.4,80.6283760070801));
#65776=CARTESIAN_POINT('Ctrl Pts',(42.1518423557281,-12.4,80.6283760070801));
#65777=CARTESIAN_POINT('Ctrl Pts',(42.8390867710114,-12.4,80.2942695617676));
#65778=CARTESIAN_POINT('Ctrl Pts',(43.8879272937775,-12.4,80.2942695617676));
#65779=CARTESIAN_POINT('',(42.1518423557281,-12.,80.6283760070801));
#65780=CARTESIAN_POINT('Ctrl Pts',(41.0374491214752,-12.,81.6856746673584));
#65781=CARTESIAN_POINT('Ctrl Pts',(41.0374491214752,-12.4,81.6856746673584));
#65782=CARTESIAN_POINT('Ctrl Pts',(41.4645979404449,-12.,80.9624824523926));
#65783=CARTESIAN_POINT('Ctrl Pts',(41.4645979404449,-12.4,80.9624824523926));
#65784=CARTESIAN_POINT('Ctrl Pts',(42.1518423557281,-12.,80.6283760070801));
#65785=CARTESIAN_POINT('Ctrl Pts',(42.1518423557281,-12.4,80.6283760070801));
#65786=CARTESIAN_POINT('',(41.0374491214752,-12.4,81.6856746673584));
#65787=CARTESIAN_POINT('Ctrl Pts',(41.0374491214752,-12.4,81.6856746673584));
#65788=CARTESIAN_POINT('Ctrl Pts',(41.4645979404449,-12.4,80.9624824523926));
#65789=CARTESIAN_POINT('Ctrl Pts',(42.1518423557281,-12.4,80.6283760070801));
#65790=CARTESIAN_POINT('',(41.0374491214752,-12.,81.6856746673584));
#65791=CARTESIAN_POINT('Ctrl Pts',(40.6103012561798,-12.,83.4957704544067));
#65792=CARTESIAN_POINT('Ctrl Pts',(40.6103012561798,-12.4,83.4957704544067));
#65793=CARTESIAN_POINT('Ctrl Pts',(40.6103012561798,-12.,82.4088668823242));
#65794=CARTESIAN_POINT('Ctrl Pts',(40.6103012561798,-12.4,82.4088668823242));
#65795=CARTESIAN_POINT('Ctrl Pts',(41.0374491214752,-12.,81.6856746673584));
#65796=CARTESIAN_POINT('Ctrl Pts',(41.0374491214752,-12.4,81.6856746673584));
#65797=CARTESIAN_POINT('Ctrl Pts',(40.6103012561798,-12.4,83.4957704544067));
#65798=CARTESIAN_POINT('Ctrl Pts',(40.6103012561798,-12.4,82.4088668823242));
#65799=CARTESIAN_POINT('Ctrl Pts',(41.0374491214752,-12.4,81.6856746673584));
#65800=CARTESIAN_POINT('Origin',(43.8223745822906,-12.4,83.4999992847443));
#65801=CARTESIAN_POINT('Origin',(49.5719635486603,-12.,82.1255111694336));
#65802=CARTESIAN_POINT('',(47.7322647571564,-12.4,82.1255111694336));
#65803=CARTESIAN_POINT('',(47.7322647571564,-12.,82.1255111694336));
#65804=CARTESIAN_POINT('',(49.5719635486603,-12.4,82.1255111694336));
#65805=CARTESIAN_POINT('',(47.7322647571564,-12.4,82.1255111694336));
#65806=CARTESIAN_POINT('',(49.5719635486603,-12.,82.1255111694336));
#65807=CARTESIAN_POINT('Origin',(49.5719635486603,-12.,80.3999996185303));
#65808=CARTESIAN_POINT('',(49.5719635486603,-12.4,80.3999996185303));
#65809=CARTESIAN_POINT('',(49.5719635486603,-12.4,82.1255111694336));
#65810=CARTESIAN_POINT('',(49.5719635486603,-12.,80.3999996185303));
#65811=CARTESIAN_POINT('Origin',(47.7322647571564,-12.,80.3999996185303));
#65812=CARTESIAN_POINT('',(47.7322647571564,-12.4,80.3999996185303));
#65813=CARTESIAN_POINT('',(49.5719635486603,-12.4,80.3999996185303));
#65814=CARTESIAN_POINT('',(47.7322647571564,-12.,80.3999996185303));
#65815=CARTESIAN_POINT('Origin',(47.7322647571564,-12.,82.1255111694336));
#65816=CARTESIAN_POINT('',(47.7322647571564,-12.4,80.3999996185303));
#65817=CARTESIAN_POINT('Origin',(48.6521141529083,-12.4,81.2627553939819));
#65818=CARTESIAN_POINT('Origin',(56.25,15.,10.5));
#65819=CARTESIAN_POINT('',(51.75,15.,10.5));
#65820=CARTESIAN_POINT('Origin',(54.,15.,10.5));
#65821=CARTESIAN_POINT('Origin',(54.,15.,10.765));
#65822=CARTESIAN_POINT('',(51.75,15.,10.765));
#65823=CARTESIAN_POINT('Origin',(56.25,-15.,10.5));
#65824=CARTESIAN_POINT('',(51.75,-15.,10.5));
#65825=CARTESIAN_POINT('Origin',(54.,-15.,10.5));
#65826=CARTESIAN_POINT('Origin',(54.,-15.,10.765));
#65827=CARTESIAN_POINT('',(51.75,-15.,10.765));
#65828=CARTESIAN_POINT('Origin',(-8.,15.,10.765));
#65829=CARTESIAN_POINT('',(-10.25,15.,10.765));
#65830=CARTESIAN_POINT('Origin',(-8.,-15.,10.765));
#65831=CARTESIAN_POINT('',(-10.25,-15.,10.765));
#65832=CARTESIAN_POINT('Origin',(-6.,11.,0.));
#65833=CARTESIAN_POINT('',(-6.,-11.,0.));
#65834=CARTESIAN_POINT('Origin',(48.,-11.,0.));
#65835=CARTESIAN_POINT('',(48.,-11.,0.));
#65836=CARTESIAN_POINT('Origin',(-6.,-11.,0.));
#65837=CARTESIAN_POINT('Origin',(0.,0.,11.));
#65838=CARTESIAN_POINT('Origin',(-11.9,9.5,0.1));
#65839=CARTESIAN_POINT('',(-12.,17.5,0.2));
#65840=CARTESIAN_POINT('',(-12.,9.5,0.2));
#65841=CARTESIAN_POINT('',(-11.8,17.5,0.));
#65842=CARTESIAN_POINT('Origin',(-12.,19.,0.));
#65843=CARTESIAN_POINT('',(-12.,17.5,0.));
#65844=CARTESIAN_POINT('Origin',(4.62,-2.26,64.1));
#65845=CARTESIAN_POINT('',(4.72,-4.72,64.));
#65846=CARTESIAN_POINT('Origin',(8.95,-4.62,64.1));
#65847=CARTESIAN_POINT('',(1.425,-4.52,64.2));
#65848=CARTESIAN_POINT('Origin',(-6.1,-4.52,62.));
#65849=CARTESIAN_POINT('',(4.52,-4.52,91.8));
#65850=CARTESIAN_POINT('',(-6.05,-4.52,91.8));
#65851=CARTESIAN_POINT('',(4.52,-4.52,62.));
#65852=CARTESIAN_POINT('Origin',(4.62,-2.26,91.9));
#65853=CARTESIAN_POINT('',(4.52,-2.26,91.8));
#65854=CARTESIAN_POINT('',(4.52,-4.52,91.8));
#65855=CARTESIAN_POINT('Origin',(-6.05,-4.62,91.9));
#65856=CARTESIAN_POINT('Origin',(4.52,-4.52,62.));
#65857=CARTESIAN_POINT('Origin',(9.31,13.9,78.));
#65858=CARTESIAN_POINT('',(2.855,14.,78.));
#65859=CARTESIAN_POINT('Origin',(9.31,14.,78.));
#65860=CARTESIAN_POINT('',(2.955,13.9,78.));
#65861=CARTESIAN_POINT('Origin',(9.31,14.,78.));
#65862=CARTESIAN_POINT('',(-0.390000000000001,14.,78.));
#65863=CARTESIAN_POINT('Origin',(9.31,14.,78.));
#65864=CARTESIAN_POINT('Origin',(9.31,-13.9,78.));
#65865=CARTESIAN_POINT('',(2.855,-14.,78.));
#65866=CARTESIAN_POINT('Origin',(9.31,-14.,78.));
#65867=CARTESIAN_POINT('',(2.955,-13.9,78.));
#65868=CARTESIAN_POINT('Origin',(9.31,-14.,78.));
#65869=CARTESIAN_POINT('',(-0.390000000000001,-14.,78.));
#65870=CARTESIAN_POINT('Origin',(9.31,-14.,78.));
#65871=CARTESIAN_POINT('Origin',(9.31,-12.15,78.));
#65872=CARTESIAN_POINT('',(-0.690000000000001,-12.3,78.));
#65873=CARTESIAN_POINT('',(-0.840000000000002,-12.15,78.));
#65874=CARTESIAN_POINT('Origin',(9.31,-12.3,78.));
#65875=CARTESIAN_POINT('Origin',(9.31,0.,78.));
#65876=CARTESIAN_POINT('',(-0.690000000000001,-13.7,78.));
#65877=CARTESIAN_POINT('',(-0.690000000000001,0.,78.));
#65878=CARTESIAN_POINT('Origin',(9.31,-13.7,78.));
#65879=CARTESIAN_POINT('Origin',(24.25,-12.,61.5));
#65880=CARTESIAN_POINT('Origin',(9.31,-13.85,78.));
#65881=CARTESIAN_POINT('',(-0.540000000000001,-13.85,78.));
#65882=CARTESIAN_POINT('Origin',(9.31,12.15,78.));
#65883=CARTESIAN_POINT('',(-0.690000000000001,12.3,78.));
#65884=CARTESIAN_POINT('',(-0.840000000000002,12.15,78.));
#65885=CARTESIAN_POINT('Origin',(9.31,12.3,78.));
#65886=CARTESIAN_POINT('Origin',(9.31,0.,78.));
#65887=CARTESIAN_POINT('',(-0.690000000000001,13.7,78.));
#65888=CARTESIAN_POINT('Origin',(9.31,13.7,78.));
#65889=CARTESIAN_POINT('',(-0.690000000000001,0.,78.));
#65890=CARTESIAN_POINT('Origin',(9.31,13.85,78.));
#65891=CARTESIAN_POINT('',(-0.540000000000001,13.85,78.));
#65892=CARTESIAN_POINT('Origin',(24.0625,-12.106066017178,11.343933982822));
#65893=CARTESIAN_POINT('',(27.1391971013664,-12.212132034356,11.087867965644));
#65894=CARTESIAN_POINT('Origin',(24.,-10.0189862838483,16.3825901807804));
#65895=CARTESIAN_POINT('',(24.0625,-12.212132034356,11.087867965644));
#65896=CARTESIAN_POINT('Origin',(44.,-11.85,100.));
#65897=CARTESIAN_POINT('',(32.,-11.7,100.));
#65898=CARTESIAN_POINT('Origin',(32.15,-11.85,79.25));
#65899=CARTESIAN_POINT('',(32.,-11.7,97.));
#65900=CARTESIAN_POINT('Origin',(27.,-11.85,97.));
#65901=CARTESIAN_POINT('',(27.,-11.7,92.));
#65902=CARTESIAN_POINT('Origin',(27.,-11.7,97.));
#65903=CARTESIAN_POINT('Origin',(9.125,-11.85,91.85));
#65904=CARTESIAN_POINT('Origin',(-9.85,-11.85,64.75));
#65905=CARTESIAN_POINT('',(-10.,-11.7,68.));
#65906=CARTESIAN_POINT('Origin',(-5.99999999999999,-11.85,68.));
#65907=CARTESIAN_POINT('',(-6.,-11.7,64.));
#65908=CARTESIAN_POINT('Origin',(24.125,-11.85,64.15));
#65909=CARTESIAN_POINT('Origin',(32.15,-11.85,40.25));
#65910=CARTESIAN_POINT('',(32.,-11.7,19.));
#65911=CARTESIAN_POINT('Origin',(24.,-11.85,19.));
#65912=CARTESIAN_POINT('',(27.0983866769659,-12.,11.3));
#65913=CARTESIAN_POINT('Ctrl Pts',(27.0983866769659,-12.,11.3));
#65914=CARTESIAN_POINT('Ctrl Pts',(27.0690767311041,-11.8486440903987,11.4513559096013));
#65915=CARTESIAN_POINT('Ctrl Pts',(27.0397667852433,-11.7001517572237,11.5998482427763));
#65916=CARTESIAN_POINT('Ctrl Pts',(27.1391971013664,-12.212132034356,11.087867965644));
#65917=CARTESIAN_POINT('Ctrl Pts',(27.1187918891661,-12.1053720627028,11.1946279372972));
#65918=CARTESIAN_POINT('Ctrl Pts',(27.0983866769659,-12.,11.3));
#65919=CARTESIAN_POINT('Origin',(27.,0.,97.));
#65920=CARTESIAN_POINT('Origin',(27.,11.7,97.));
#65921=CARTESIAN_POINT('Origin',(58.5,0.,13.5));
#65922=CARTESIAN_POINT('Origin',(58.5,-9.79999999999997,13.5));
#65923=CARTESIAN_POINT('Origin',(32.15,11.85,40.25));
#65924=CARTESIAN_POINT('',(32.,11.7,56.));
#65925=CARTESIAN_POINT('Origin',(24.,11.85,56.));
#65926=CARTESIAN_POINT('',(24.,11.7,64.));
#65927=CARTESIAN_POINT('Origin',(24.125,11.85,64.15));
#65928=CARTESIAN_POINT('Origin',(-9.85,11.85,64.75));
#65929=CARTESIAN_POINT('Origin',(9.125,11.85,91.85));
#65930=CARTESIAN_POINT('',(27.,11.7,92.));
#65931=CARTESIAN_POINT('Origin',(27.,11.85,97.));
#65932=CARTESIAN_POINT('',(32.,11.7,97.));
#65933=CARTESIAN_POINT('Origin',(32.15,11.85,79.25));
#65934=CARTESIAN_POINT('Origin',(58.9,-9.5,0.1));
#65935=CARTESIAN_POINT('',(59.,17.5,0.2));
#65936=CARTESIAN_POINT('',(58.8,17.5,0.));
#65937=CARTESIAN_POINT('',(59.,-17.5,0.2));
#65938=CARTESIAN_POINT('',(59.,-9.5,0.2));
#65939=CARTESIAN_POINT('',(59.,-17.5,0.2));
#65940=CARTESIAN_POINT('Origin',(57.5,17.5,0.1));
#65941=CARTESIAN_POINT('',(57.5,19.,0.2));
#65942=CARTESIAN_POINT('',(57.5,18.8,0.));
#65943=CARTESIAN_POINT('Origin',(57.5,17.5,0.2));
#65944=CARTESIAN_POINT('Origin',(41.25,18.9,0.1));
#65945=CARTESIAN_POINT('',(-10.5,19.,0.2));
#65946=CARTESIAN_POINT('',(-10.5,18.8,0.));
#65947=CARTESIAN_POINT('',(41.25,19.,0.2));
#65948=CARTESIAN_POINT('Origin',(-10.5,17.5,0.1));
#65949=CARTESIAN_POINT('Origin',(-10.5,17.5,0.2));
#65950=CARTESIAN_POINT('Origin',(-10.5,-17.5,0.1));
#65951=CARTESIAN_POINT('',(-10.5,-19.,0.2));
#65952=CARTESIAN_POINT('',(-10.5,-18.8,0.));
#65953=CARTESIAN_POINT('Origin',(-10.5,-17.5,0.2));
#65954=CARTESIAN_POINT('Origin',(5.75,-18.9,0.1));
#65955=CARTESIAN_POINT('',(57.5,-19.,0.2));
#65956=CARTESIAN_POINT('',(57.5,-18.8,0.));
#65957=CARTESIAN_POINT('',(5.75,-19.,0.2));
#65958=CARTESIAN_POINT('Origin',(57.5,-17.5,0.1));
#65959=CARTESIAN_POINT('Origin',(57.5,-17.5,0.2));
#65960=CARTESIAN_POINT('Origin',(-10.5,-17.5,0.));
#65961=CARTESIAN_POINT('',(-10.5,-19.,10.7));
#65962=CARTESIAN_POINT('',(-10.5,-19.,0.));
#65963=CARTESIAN_POINT('Origin',(-10.5,-17.5,10.7));
#65964=CARTESIAN_POINT('Origin',(-12.,-19.,0.));
#65965=CARTESIAN_POINT('',(57.5,-19.,10.7));
#65966=CARTESIAN_POINT('',(57.5,-19.,0.));
#65967=CARTESIAN_POINT('',(5.75,-19.,10.7));
#65968=CARTESIAN_POINT('Origin',(57.5,-17.5,0.));
#65969=CARTESIAN_POINT('',(59.,-17.5,10.7));
#65970=CARTESIAN_POINT('',(59.,-17.5,0.));
#65971=CARTESIAN_POINT('Origin',(57.5,-17.5,10.7));
#65972=CARTESIAN_POINT('Origin',(59.,-19.,0.));
#65973=CARTESIAN_POINT('',(59.,17.5,10.7));
#65974=CARTESIAN_POINT('',(59.,17.5,0.));
#65975=CARTESIAN_POINT('',(59.,-9.5,10.7));
#65976=CARTESIAN_POINT('Origin',(23.875,-12.15,11.15));
#65977=CARTESIAN_POINT('Origin',(-10.5,-17.5,10.85));
#65978=CARTESIAN_POINT('',(-10.5,-19.,10.7));
#65979=CARTESIAN_POINT('Origin',(-10.5,17.5,10.85));
#65980=CARTESIAN_POINT('',(-10.5,19.,10.7));
#65981=CARTESIAN_POINT('',(-10.5,18.7,11.));
#65982=CARTESIAN_POINT('Origin',(-10.5,17.5,10.7));
#65983=CARTESIAN_POINT('Origin',(41.25,18.85,10.85));
#65984=CARTESIAN_POINT('',(57.5,19.,10.7));
#65985=CARTESIAN_POINT('',(57.5,18.7,11.));
#65986=CARTESIAN_POINT('',(41.25,19.,10.7));
#65987=CARTESIAN_POINT('Origin',(57.5,17.5,10.85));
#65988=CARTESIAN_POINT('',(58.7,17.5,11.));
#65989=CARTESIAN_POINT('Origin',(57.5,17.5,10.7));
#65990=CARTESIAN_POINT('Origin',(58.85,-9.5,10.85));
#65991=CARTESIAN_POINT('',(58.7,-17.5,11.));
#65992=CARTESIAN_POINT('Origin',(57.5,-17.5,10.85));
#65993=CARTESIAN_POINT('',(57.5,-18.7,11.));
#65994=CARTESIAN_POINT('Origin',(5.75,-18.85,10.85));
#65995=CARTESIAN_POINT('Origin',(57.5,17.5,0.));
#65996=CARTESIAN_POINT('',(57.5,19.,0.));
#65997=CARTESIAN_POINT('Origin',(-10.5,17.5,0.));
#65998=CARTESIAN_POINT('',(-10.5,19.,0.));
#65999=CARTESIAN_POINT('Origin',(59.,19.,0.));
#66000=CARTESIAN_POINT('',(0.,0.,0.));
#66001=CARTESIAN_POINT('Origin',(0.,0.,-1.425));
#66002=CARTESIAN_POINT('',(-0.791102872936695,2.03416717624305E-5,-2.8446668491763));
#66003=CARTESIAN_POINT('',(-0.791090026729892,1.30542722735929E-5,-2.87313315082371));
#66004=CARTESIAN_POINT('',(-0.7911,-9.68818082805471E-17,-1.425));
#66005=CARTESIAN_POINT('',(0.342081635505615,0.713330693753523,-2.9089));
#66006=CARTESIAN_POINT('Ctrl Pts',(-0.791102872936695,2.03416717624305E-5,
-2.8446668491763));
#66007=CARTESIAN_POINT('Ctrl Pts',(-0.791132933740977,0.0293885304818959,
-2.84584855390734));
#66008=CARTESIAN_POINT('Ctrl Pts',(-0.789528925786739,0.0587534438189118,
-2.84703025863837));
#66009=CARTESIAN_POINT('Ctrl Pts',(-0.786265627890728,0.0879327739588084,
-2.84821196336941));
#66010=CARTESIAN_POINT('Ctrl Pts',(-0.771682871848867,0.218326953851245,
-2.85349266784549));
#66011=CARTESIAN_POINT('Ctrl Pts',(-0.723965033050537,0.345015142138505,
-2.85877337232157));
#66012=CARTESIAN_POINT('Ctrl Pts',(-0.64890100849163,0.452629069386829,
-2.86405407679765));
#66013=CARTESIAN_POINT('Ctrl Pts',(-0.573836983932724,0.560242996635152,
-2.86933478127373));
#66014=CARTESIAN_POINT('Ctrl Pts',(-0.47142677361324,0.648782662844538,
-2.8746154857498));
#66015=CARTESIAN_POINT('Ctrl Pts',(-0.354094167074879,0.707505252038821,
-2.87989619022588));
#66016=CARTESIAN_POINT('Ctrl Pts',(-0.236761560536518,0.766227841233104,
-2.88517689470196));
#66017=CARTESIAN_POINT('Ctrl Pts',(-0.10450655777928,0.795133353412285,
-2.89045759917804));
#66018=CARTESIAN_POINT('Ctrl Pts',(0.0266262731194924,0.790718402262909,
-2.89573830365412));
#66019=CARTESIAN_POINT('Ctrl Pts',(0.135571996118135,0.787050441755417,
-2.90012553576941));
#66020=CARTESIAN_POINT('Ctrl Pts',(0.243743155897518,0.760383503731005,
-2.9045127678847));
#66021=CARTESIAN_POINT('Ctrl Pts',(0.342095308501471,0.713339076749545,
-2.9089));
#66022=CARTESIAN_POINT('',(-0.342067962509755,0.713322310757504,-2.9089));
#66023=CARTESIAN_POINT('Origin',(0.,0.,-2.9089));
#66024=CARTESIAN_POINT('Ctrl Pts',(-0.342067962509754,0.713322310757504,
-2.9089));
#66025=CARTESIAN_POINT('Ctrl Pts',(-0.460406866917162,0.65657384333148,
-2.90361929552392));
#66026=CARTESIAN_POINT('Ctrl Pts',(-0.564293460884465,0.569839529886298,
-2.89833859104784));
#66027=CARTESIAN_POINT('Ctrl Pts',(-0.641163354894195,0.463527805702664,
-2.89305788657176));
#66028=CARTESIAN_POINT('Ctrl Pts',(-0.718033248903927,0.357216081519026,
-2.88777718209569));
#66029=CARTESIAN_POINT('Ctrl Pts',(-0.767886442956084,0.231326946596934,
-2.88249647761961));
#66030=CARTESIAN_POINT('Ctrl Pts',(-0.784669586715434,0.101191204740451,
-2.87721577314353));
#66031=CARTESIAN_POINT('Ctrl Pts',(-0.788994719067196,0.0676543230158658,
-2.87585489903692));
#66032=CARTESIAN_POINT('Ctrl Pts',(-0.791123574843936,0.0338354119852844,
-2.87449402493032));
#66033=CARTESIAN_POINT('Ctrl Pts',(-0.791090026729892,1.30542722735929E-5,
-2.87313315082371));
#66034=CARTESIAN_POINT('Origin',(0.,0.,-1.425));
#66035=CARTESIAN_POINT('',(-0.791132110743512,-1.71897034488278E-5,-2.6446668491763));
#66036=CARTESIAN_POINT('',(-0.791144428618858,-1.44065313715571E-5,-2.6731331508237));
#66037=CARTESIAN_POINT('',(-0.7911,-9.68818082805471E-17,-1.425));
#66038=CARTESIAN_POINT('Ctrl Pts',(-0.791132110743512,-1.71897034488278E-5,
-2.6446668491763));
#66039=CARTESIAN_POINT('Ctrl Pts',(-0.791026015708889,0.111307599100088,
-2.64914676686106));
#66040=CARTESIAN_POINT('Ctrl Pts',(-0.767301189153144,0.222676174543509,
-2.65362668454582));
#66041=CARTESIAN_POINT('Ctrl Pts',(-0.721687452926102,0.324211361281666,
-2.65810660223059));
#66042=CARTESIAN_POINT('Ctrl Pts',(-0.667920246023168,0.443895996763073,
-2.66338730670667));
#66043=CARTESIAN_POINT('Ctrl Pts',(-0.583739442038409,0.549917607154516,
-2.66866801118275));
#66044=CARTESIAN_POINT('Ctrl Pts',(-0.479357396305173,0.629414230058327,
-2.67394871565882));
#66045=CARTESIAN_POINT('Ctrl Pts',(-0.374975350571937,0.708910852962139,
-2.6792294201349));
#66046=CARTESIAN_POINT('Ctrl Pts',(-0.250392063090227,0.761882488378319,
-2.68451012461098));
#66047=CARTESIAN_POINT('Ctrl Pts',(-0.120721297776761,0.781902906330603,
-2.68979082908706));
#66048=CARTESIAN_POINT('Ctrl Pts',(0.00894946753670305,0.801923324282887,
-2.69507153356314));
#66049=CARTESIAN_POINT('Ctrl Pts',(0.143707710681922,0.788992524771275,
-2.70035223803922));
#66050=CARTESIAN_POINT('Ctrl Pts',(0.267205297646592,0.744679202764205,
-2.70563294251529));
#66051=CARTESIAN_POINT('Ctrl Pts',(0.390702884611263,0.700365880757135,
-2.71091364699137));
#66052=CARTESIAN_POINT('Ctrl Pts',(0.502939815395386,0.624670036254607,
-2.71619435146745));
#66053=CARTESIAN_POINT('Ctrl Pts',(0.590300118688603,0.526774673675583,
-2.72147505594353));
#66054=CARTESIAN_POINT('Ctrl Pts',(0.677660421981819,0.428879311096558,
-2.72675576041961));
#66055=CARTESIAN_POINT('Ctrl Pts',(0.740144097784128,0.308784430441036,
-2.73203646489569));
#66056=CARTESIAN_POINT('Ctrl Pts',(0.770170967713734,0.181059290505753,
-2.73731716937176));
#66057=CARTESIAN_POINT('Ctrl Pts',(0.800197837643339,0.0533341505704711,
-2.74259787384784));
#66058=CARTESIAN_POINT('Ctrl Pts',(0.797767901700242,-0.0820212486445725,
-2.74787857832392));
#66059=CARTESIAN_POINT('Ctrl Pts',(0.763175946702779,-0.20858633702776,
-2.7531592828));
#66060=CARTESIAN_POINT('Ctrl Pts',(0.728583991705317,-0.335151425410948,
-2.75843998727608));
#66061=CARTESIAN_POINT('Ctrl Pts',(0.661830017653489,-0.452926202962279,
-2.76372069175216));
#66062=CARTESIAN_POINT('Ctrl Pts',(0.57101225153822,-0.547622862109841,
-2.76900139622824));
#66063=CARTESIAN_POINT('Ctrl Pts',(0.480194485422949,-0.642319521257404,
-2.77428210070431));
#66064=CARTESIAN_POINT('Ctrl Pts',(0.365312927244237,-0.713938062001196,
-2.77956280518039));
#66065=CARTESIAN_POINT('Ctrl Pts',(0.240304381141893,-0.753790143362176,
-2.78484350965647));
#66066=CARTESIAN_POINT('Ctrl Pts',(0.11529583503955,-0.793642224723155,
-2.79012421413255));
#66067=CARTESIAN_POINT('Ctrl Pts',(-0.0198396989864242,-0.801727846701323,
-2.79540491860863));
#66068=CARTESIAN_POINT('Ctrl Pts',(-0.148708318074358,-0.777066048525618,
-2.80068562308471));
#66069=CARTESIAN_POINT('Ctrl Pts',(-0.277576937162291,-0.752404250349915,
-2.80596632756078));
#66070=CARTESIAN_POINT('Ctrl Pts',(-0.400178641312184,-0.69499503202034,
-2.81124703203686));
#66071=CARTESIAN_POINT('Ctrl Pts',(-0.50164005756068,-0.611803078728568,
-2.81652773651294));
#66072=CARTESIAN_POINT('Ctrl Pts',(-0.603101473809176,-0.528611125436796,
-2.82180844098902));
#66073=CARTESIAN_POINT('Ctrl Pts',(-0.683422602156275,-0.419636437182826,
-2.8270891454651));
#66074=CARTESIAN_POINT('Ctrl Pts',(-0.732859329687128,-0.298099007307034,
-2.83236984994118));
#66075=CARTESIAN_POINT('Ctrl Pts',(-0.771233212274681,-0.203758963032545,
-2.83646884968622));
#66076=CARTESIAN_POINT('Ctrl Pts',(-0.790998600502259,-0.101849605433625,
-2.84056784943126));
#66077=CARTESIAN_POINT('Ctrl Pts',(-0.791102872936695,2.03416717624305E-5,
-2.8446668491763));
#66078=CARTESIAN_POINT('Ctrl Pts',(-0.791090026729892,1.30542722735929E-5,
-2.87313315082371));
#66079=CARTESIAN_POINT('Ctrl Pts',(-0.790993395516444,-0.0974080843082692,
-2.86921332045424));
#66080=CARTESIAN_POINT('Ctrl Pts',(-0.772956226440993,-0.194857818535022,
-2.86529349008476));
#66081=CARTESIAN_POINT('Ctrl Pts',(-0.737787983582658,-0.285678789184145,
-2.86137365971529));
#66082=CARTESIAN_POINT('Ctrl Pts',(-0.690410143223988,-0.408030692461386,
-2.85609295523921));
#66083=CARTESIAN_POINT('Ctrl Pts',(-0.611941369040105,-0.518352150224994,
-2.85081225076314));
#66084=CARTESIAN_POINT('Ctrl Pts',(-0.511899355351125,-0.60324695438924,
-2.84553154628706));
#66085=CARTESIAN_POINT('Ctrl Pts',(-0.411857341662145,-0.688141758553486,
-2.84025084181098));
#66086=CARTESIAN_POINT('Ctrl Pts',(-0.290242088468068,-0.74760990911837,
-2.8349701373349));
#66087=CARTESIAN_POINT('Ctrl Pts',(-0.161808168596516,-0.774443449936211,
-2.82968943285882));
#66088=CARTESIAN_POINT('Ctrl Pts',(-0.0333742487249623,-0.801276990754052,
-2.82440872838274));
#66089=CARTESIAN_POINT('Ctrl Pts',(0.101878337824068,-0.795475921824851,
-2.81912802390667));
#66090=CARTESIAN_POINT('Ctrl Pts',(0.227541932230471,-0.757740739969511,
-2.81384731943059));
#66091=CARTESIAN_POINT('Ctrl Pts',(0.353205526636875,-0.720005558114172,
-2.80856661495451));
#66092=CARTESIAN_POINT('Ctrl Pts',(0.469280128900652,-0.650336263332695,
-2.80328591047843));
#66093=CARTESIAN_POINT('Ctrl Pts',(0.561683974793613,-0.557186414195635,
-2.79800520600235));
#66094=CARTESIAN_POINT('Ctrl Pts',(0.654087820686573,-0.464036565058575,
-2.79272450152627));
#66095=CARTESIAN_POINT('Ctrl Pts',(0.722820910208717,-0.347406161565934,
-2.7874437970502));
#66096=CARTESIAN_POINT('Ctrl Pts',(0.759545036365206,-0.221443320796046,
-2.78216309257412));
#66097=CARTESIAN_POINT('Ctrl Pts',(0.796269162521695,-0.0954804800261573,
-2.77688238809804));
#66098=CARTESIAN_POINT('Ctrl Pts',(0.800984325312529,0.0398147980209764,
-2.77160168362196));
#66099=CARTESIAN_POINT('Ctrl Pts',(0.773118447809453,0.168028797714986,
-2.76632097914588));
#66100=CARTESIAN_POINT('Ctrl Pts',(0.745252570306378,0.296242797408994,
-2.7610402746698));
#66101=CARTESIAN_POINT('Ctrl Pts',(0.684805652509392,0.417375518749878,
-2.75575957019373));
#66102=CARTESIAN_POINT('Ctrl Pts',(0.599110814457919,0.516732021631281,
-2.75047886571765));
#66103=CARTESIAN_POINT('Ctrl Pts',(0.513415976406445,0.616088524512684,
-2.74519816124157));
#66104=CARTESIAN_POINT('Ctrl Pts',(0.402473218100484,0.693668808934607,
-2.73991745676549));
#66105=CARTESIAN_POINT('Ctrl Pts',(0.27974149361296,0.740061146397167,-2.73463675228941));
#66106=CARTESIAN_POINT('Ctrl Pts',(0.157009769125436,0.786453483859727,
-2.72935604781333));
#66107=CARTESIAN_POINT('Ctrl Pts',(0.0224890784563497,0.801657874362924,
-2.72407534333726));
#66108=CARTESIAN_POINT('Ctrl Pts',(-0.107501255149887,0.783829861479462,
-2.71879463886118));
#66109=CARTESIAN_POINT('Ctrl Pts',(-0.237491588756123,0.766001848595999,
-2.7135139343851));
#66110=CARTESIAN_POINT('Ctrl Pts',(-0.36295156529951,0.715141432325876,
-2.70823322990902));
#66111=CARTESIAN_POINT('Ctrl Pts',(-0.468661069712101,0.637418691408968,
-2.70295252543294));
#66112=CARTESIAN_POINT('Ctrl Pts',(-0.574370574124692,0.559695950492061,
-2.69767182095686));
#66113=CARTESIAN_POINT('Ctrl Pts',(-0.660329606406489,0.455110884928367,
-2.69239111648079));
#66114=CARTESIAN_POINT('Ctrl Pts',(-0.716110084252664,0.336351198465617,
-2.68711041200471));
#66115=CARTESIAN_POINT('Ctrl Pts',(-0.765324370666461,0.231571292490118,
-2.68245132494437));
#66116=CARTESIAN_POINT('Ctrl Pts',(-0.791046853705215,0.115757478055327,
-2.67779223788404));
#66117=CARTESIAN_POINT('Ctrl Pts',(-0.791144428618858,-1.44065313715571E-5,
-2.6731331508237));
#66118=CARTESIAN_POINT('Origin',(0.,0.,-1.425));
#66119=CARTESIAN_POINT('',(-0.79103374865932,3.27018256038314E-6,-2.4446668491763));
#66120=CARTESIAN_POINT('',(-0.791033002877254,-8.32524903205056E-7,-2.47313315082371));
#66121=CARTESIAN_POINT('',(-0.7911,-9.68818082805471E-17,-1.425));
#66122=CARTESIAN_POINT('Ctrl Pts',(-0.79103374865932,3.27018256038314E-6,
-2.4446668491763));
#66123=CARTESIAN_POINT('Ctrl Pts',(-0.791042731182178,0.0620858397671934,
-2.44716427533871));
#66124=CARTESIAN_POINT('Ctrl Pts',(-0.783823321886597,0.124166354682933,
-2.44966170150112));
#66125=CARTESIAN_POINT('Ctrl Pts',(-0.769352119996688,0.184507728644354,
-2.45215912766353));
#66126=CARTESIAN_POINT('Ctrl Pts',(-0.738753361264814,0.31209707177161,
-2.45743983213961));
#66127=CARTESIAN_POINT('Ctrl Pts',(-0.675732304910451,0.431910827705095,
-2.46272053661569));
#66128=CARTESIAN_POINT('Ctrl Pts',(-0.587934321254863,0.529413846025484,
-2.46800124109177));
#66129=CARTESIAN_POINT('Ctrl Pts',(-0.500136337599273,0.626916864345873,
-2.47328194556784));
#66130=CARTESIAN_POINT('Ctrl Pts',(-0.387561426642458,0.702109145053164,
-2.47856265004392));
#66131=CARTESIAN_POINT('Ctrl Pts',(-0.263866561671389,0.74586877136973,
-2.48384335452));
#66132=CARTESIAN_POINT('Ctrl Pts',(-0.140171696700323,0.789628397686295,
-2.48912405899608));
#66133=CARTESIAN_POINT('Ctrl Pts',(-0.00535687771500397,0.801955369612136,
-2.49440476347216));
#66134=CARTESIAN_POINT('Ctrl Pts',(0.124222897835128,0.781354246245838,
-2.49968546794824));
#66135=CARTESIAN_POINT('Ctrl Pts',(0.253802673385261,0.760753122879539,
-2.50496617242431));
#66136=CARTESIAN_POINT('Ctrl Pts',(0.378147405500207,0.707223904221101,
-2.51024687690039));
#66137=CARTESIAN_POINT('Ctrl Pts',(0.482172270479579,0.627260462689446,
-2.51552758137647));
#66138=CARTESIAN_POINT('Ctrl Pts',(0.586197135458951,0.547297021157791,
-2.52080828585255));
#66139=CARTESIAN_POINT('Ctrl Pts',(0.669902133302747,0.440899356752921,
-2.52608899032863));
#66140=CARTESIAN_POINT('Ctrl Pts',(0.72313263088872,0.320975052951074,-2.53136969480471));
#66141=CARTESIAN_POINT('Ctrl Pts',(0.776363128474693,0.201050749149226,
-2.53665039928079));
#66142=CARTESIAN_POINT('Ctrl Pts',(0.799119125802842,0.0675998059503994,
-2.54193110375686));
#66143=CARTESIAN_POINT('Ctrl Pts',(0.788639989575818,-0.0631882371553828,
-2.54721180823294));
#66144=CARTESIAN_POINT('Ctrl Pts',(0.778160853348794,-0.193976280261165,
-2.55249251270902));
#66145=CARTESIAN_POINT('Ctrl Pts',(0.734446583566596,-0.322101423273906,
-2.5577732171851));
#66146=CARTESIAN_POINT('Ctrl Pts',(0.662800356661787,-0.432020223694912,
-2.56305392166118));
#66147=CARTESIAN_POINT('Ctrl Pts',(0.59115412975698,-0.541939024115916,
-2.56833462613726));
#66148=CARTESIAN_POINT('Ctrl Pts',(0.491575945729561,-0.633651481945187,
-2.57361533061333));
#66149=CARTESIAN_POINT('Ctrl Pts',(0.376146085946411,-0.696031542749064,
-2.57889603508941));
#66150=CARTESIAN_POINT('Ctrl Pts',(0.260716226163259,-0.758411603552943,
-2.58417673956549));
#66151=CARTESIAN_POINT('Ctrl Pts',(0.129434690624375,-0.791459267331427,
-2.58945744404157));
#66152=CARTESIAN_POINT('Ctrl Pts',(-0.00177216186859303,-0.791165372037872,
-2.59473814851765));
#66153=CARTESIAN_POINT('Ctrl Pts',(-0.132979014361561,-0.790871476744317,
-2.60001885299372));
#66154=CARTESIAN_POINT('Ctrl Pts',(-0.264111183808613,-0.757236022378723,
-2.6052995574698));
#66155=CARTESIAN_POINT('Ctrl Pts',(-0.379260431687407,-0.694339478522506,
-2.61058026194588));
#66156=CARTESIAN_POINT('Ctrl Pts',(-0.4944096795662,-0.631442934666289,
-2.61586096642196));
#66157=CARTESIAN_POINT('Ctrl Pts',(-0.593576005876736,-0.53928530131945,
-2.62114167089804));
#66158=CARTESIAN_POINT('Ctrl Pts',(-0.664729093579334,-0.429046639207677,
-2.62642237537412));
#66159=CARTESIAN_POINT('Ctrl Pts',(-0.735882181281933,-0.318807977095903,
-2.6317030798502));
#66160=CARTESIAN_POINT('Ctrl Pts',(-0.779022030376594,-0.190488286219194,
-2.63698378432627));
#66161=CARTESIAN_POINT('Ctrl Pts',(-0.78891515001337,-0.059654610495154,
-2.64226448880235));
#66162=CARTESIAN_POINT('Ctrl Pts',(-0.790415381576396,-0.0398144774497269,
-2.64306527559367));
#66163=CARTESIAN_POINT('Ctrl Pts',(-0.791151075266596,-0.019916533104998,
-2.64386606238498));
#66164=CARTESIAN_POINT('Ctrl Pts',(-0.791132110743512,-1.71897034488278E-5,
-2.6446668491763));
#66165=CARTESIAN_POINT('Ctrl Pts',(-0.791144428618858,-1.44065313715571E-5,
-2.6731331508237));
#66166=CARTESIAN_POINT('Ctrl Pts',(-0.791157447106144,-0.0154607415709918,
-2.67251153340796));
#66167=CARTESIAN_POINT('Ctrl Pts',(-0.790714316293819,-0.0309063302168789,
-2.67188991599221));
#66168=CARTESIAN_POINT('Ctrl Pts',(-0.7898099700181,-0.0463248671453487,
-2.67126829857647));
#66169=CARTESIAN_POINT('Ctrl Pts',(-0.782127454526808,-0.177306938931758,
-2.66598759410039));
#66170=CARTESIAN_POINT('Ctrl Pts',(-0.741160500133669,-0.306336775142769,
-2.66070688962431));
#66171=CARTESIAN_POINT('Ctrl Pts',(-0.671878993445302,-0.417761176977514,
-2.65542618514824));
#66172=CARTESIAN_POINT('Ctrl Pts',(-0.602597486756935,-0.529185578812257,
-2.65014548067216));
#66173=CARTESIAN_POINT('Ctrl Pts',(-0.50500142777334,-0.623004546270734,
-2.64486477619608));
#66174=CARTESIAN_POINT('Ctrl Pts',(-0.390930637547929,-0.687836476651132,
-2.63958407172));
#66175=CARTESIAN_POINT('Ctrl Pts',(-0.276859847322517,-0.752668407031531,
-2.63430336724392));
#66176=CARTESIAN_POINT('Ctrl Pts',(-0.146314325855289,-0.78851330033385,
-2.62902266276784));
#66177=CARTESIAN_POINT('Ctrl Pts',(-0.0151311426031084,-0.791022648891824,
-2.62374195829176));
#66178=CARTESIAN_POINT('Ctrl Pts',(0.116052040649072,-0.793531997449798,
-2.61846125381568));
#66179=CARTESIAN_POINT('Ctrl Pts',(0.247872885686205,-0.762705801263428,
-2.61318054933961));
#66180=CARTESIAN_POINT('Ctrl Pts',(0.364339607554318,-0.702283726586036,
-2.60789984486353));
#66181=CARTESIAN_POINT('Ctrl Pts',(0.48080632942243,-0.641861651908644,
-2.60261914038745));
#66182=CARTESIAN_POINT('Ctrl Pts',(0.581918928121522,-0.551843698740229,
-2.59733843591137));
#66183=CARTESIAN_POINT('Ctrl Pts',(0.655410975513677,-0.443150353199274,
-2.59205773143529));
#66184=CARTESIAN_POINT('Ctrl Pts',(0.72890302290583,-0.334457007658322,
-2.58677702695921));
#66185=CARTESIAN_POINT('Ctrl Pts',(0.774774518991048,-0.207088269744829,
-2.58149632248314));
#66186=CARTESIAN_POINT('Ctrl Pts',(0.787460584406806,-0.0764958191578642,
-2.57621561800706));
#66187=CARTESIAN_POINT('Ctrl Pts',(0.800146649822565,0.0540966314291024,
-2.57093491353098));
#66188=CARTESIAN_POINT('Ctrl Pts',(0.779647284568864,0.187912794689541,
-2.5656542090549));
#66189=CARTESIAN_POINT('Ctrl Pts',(0.728449359675282,0.308718824699482,
-2.56037350457882));
#66190=CARTESIAN_POINT('Ctrl Pts',(0.677251434781699,0.429524854709423,
-2.55509280010275));
#66191=CARTESIAN_POINT('Ctrl Pts',(0.595354950248236,0.537320751468866,
-2.54981209562667));
#66192=CARTESIAN_POINT('Ctrl Pts',(0.492695140236132,0.619029305554604,
-2.54453139115059));
#66193=CARTESIAN_POINT('Ctrl Pts',(0.39003533022403,0.700737859640341,-2.53925068667451));
#66194=CARTESIAN_POINT('Ctrl Pts',(0.266612194733288,0.756359071052374,
-2.53396998219843));
#66195=CARTESIAN_POINT('Ctrl Pts',(0.137398754398226,0.779145278255797,
-2.52868927772235));
#66196=CARTESIAN_POINT('Ctrl Pts',(0.0081853140631645,0.80193148545922,
-2.52340857324627));
#66197=CARTESIAN_POINT('Ctrl Pts',(-0.126818431116216,0.791882688454035,
-2.5181278687702));
#66198=CARTESIAN_POINT('Ctrl Pts',(-0.251234564197799,0.750217952395059,
-2.51284716429412));
#66199=CARTESIAN_POINT('Ctrl Pts',(-0.375650697279383,0.708553216336082,
-2.50756645981804));
#66200=CARTESIAN_POINT('Ctrl Pts',(-0.489479218263168,0.635272541223315,
-2.50228575534196));
#66201=CARTESIAN_POINT('Ctrl Pts',(-0.578911072740594,0.539265938289951,
-2.49700505086588));
#66202=CARTESIAN_POINT('Ctrl Pts',(-0.668342927218019,0.443259335356588,
-2.49172434638981));
#66203=CARTESIAN_POINT('Ctrl Pts',(-0.733378115189086,0.324526804602629,
-2.48644364191373));
#66204=CARTESIAN_POINT('Ctrl Pts',(-0.766126922886764,0.197472328112149,
-2.48116293743765));
#66205=CARTESIAN_POINT('Ctrl Pts',(-0.782726093121508,0.133073071082062,
-2.47848634189967));
#66206=CARTESIAN_POINT('Ctrl Pts',(-0.791030554834729,0.066535819218492,
-2.47580974636169));
#66207=CARTESIAN_POINT('Ctrl Pts',(-0.791033002877254,-8.32524903205056E-7,
-2.47313315082371));
#66208=CARTESIAN_POINT('Origin',(0.,0.,-1.425));
#66209=CARTESIAN_POINT('',(-0.791150917366707,1.23845276237822E-5,-2.2446668491763));
#66210=CARTESIAN_POINT('',(-0.791139629808145,1.56300862382004E-5,-2.27313315082371));
#66211=CARTESIAN_POINT('',(-0.7911,-9.68818082805471E-17,-1.425));
#66212=CARTESIAN_POINT('Ctrl Pts',(-0.791150917366707,1.23845276237822E-5,
-2.2446668491763));
#66213=CARTESIAN_POINT('Ctrl Pts',(-0.791160527113968,0.0128074960584554,
-2.24518178381636));
#66214=CARTESIAN_POINT('Ctrl Pts',(-0.790856504970953,0.0256021508212593,
-2.24569671845641));
#66215=CARTESIAN_POINT('Ctrl Pts',(-0.79023582091272,0.038381425446427,
-2.24621165309647));
#66216=CARTESIAN_POINT('Ctrl Pts',(-0.783870645937939,0.169434121195563,
-2.25149235757255));
#66217=CARTESIAN_POINT('Ctrl Pts',(-0.744203085343301,0.298869333913646,
-2.25677306204863));
#66218=CARTESIAN_POINT('Ctrl Pts',(-0.676045390906717,0.410984690598912,
-2.2620537665247));
#66219=CARTESIAN_POINT('Ctrl Pts',(-0.607887696470134,0.523100047284177,
-2.26733447100078));
#66220=CARTESIAN_POINT('Ctrl Pts',(-0.511239868191607,0.617895547936626,
-2.27261517547686));
#66221=CARTESIAN_POINT('Ctrl Pts',(-0.397826692685,0.683871120212145,-2.27789587995294));
#66222=CARTESIAN_POINT('Ctrl Pts',(-0.284413517178393,0.749846692487665,
-2.28317658442902));
#66223=CARTESIAN_POINT('Ctrl Pts',(-0.154234994443706,0.787002336386255,
-2.2884572889051));
#66224=CARTESIAN_POINT('Ctrl Pts',(-0.0230836717937855,0.790830532142896,
-2.29373799338118));
#66225=CARTESIAN_POINT('Ctrl Pts',(0.108067650856135,0.794658727899538,
-2.29901869785726));
#66226=CARTESIAN_POINT('Ctrl Pts',(0.24019177342129,0.765159475514229,-2.30429940233333));
#66227=CARTESIAN_POINT('Ctrl Pts',(0.357260119044719,0.705911463154589,
-2.30958010680941));
#66228=CARTESIAN_POINT('Ctrl Pts',(0.474328464668147,0.64666345079495,-2.31486081128549));
#66229=CARTESIAN_POINT('Ctrl Pts',(0.57634103334985,0.55766667846098,-2.32014151576157));
#66230=CARTESIAN_POINT('Ctrl Pts',(0.650922217473707,0.449717748451195,
-2.32542222023765));
#66231=CARTESIAN_POINT('Ctrl Pts',(0.725503401597566,0.341768818441408,
-2.33070292471373));
#66232=CARTESIAN_POINT('Ctrl Pts',(0.772653201163578,0.214867730755806,
-2.3359836291898));
#66233=CARTESIAN_POINT('Ctrl Pts',(0.786651660031553,0.0844094321891896,
-2.34126433366588));
#66234=CARTESIAN_POINT('Ctrl Pts',(0.800650118899528,-0.0460488663774256,
-2.34654503814196));
#66235=CARTESIAN_POINT('Ctrl Pts',(0.781497237069466,-0.180064375825055,
-2.35182574261804));
#66236=CARTESIAN_POINT('Ctrl Pts',(0.731516537547499,-0.30137906657135,
-2.35710644709412));
#66237=CARTESIAN_POINT('Ctrl Pts',(0.681535838025532,-0.422693757317647,
-2.3623871515702));
#66238=CARTESIAN_POINT('Ctrl Pts',(0.600727320811662,-0.531307629362611,
-2.36766785604627));
#66239=CARTESIAN_POINT('Ctrl Pts',(0.498894233819384,-0.614044241023943,
-2.37294856052235));
#66240=CARTESIAN_POINT('Ctrl Pts',(0.397061146827107,-0.696780852685274,
-2.37822926499843));
#66241=CARTESIAN_POINT('Ctrl Pts',(0.274203490056424,-0.753640203962973,
-2.38350996947451));
#66242=CARTESIAN_POINT('Ctrl Pts',(0.145225683349696,-0.777724428939013,
-2.38879067395059));
#66243=CARTESIAN_POINT('Ctrl Pts',(0.0162478766429679,-0.801808653915053,
-2.39407137842667));
#66244=CARTESIAN_POINT('Ctrl Pts',(-0.118850079999805,-0.793117752589433,
-2.39935208290275));
#66245=CARTESIAN_POINT('Ctrl Pts',(-0.243678840415138,-0.752706057639257,
-2.40463278737882));
#66246=CARTESIAN_POINT('Ctrl Pts',(-0.36850760083047,-0.712294362689082,
-2.4099134918549));
#66247=CARTESIAN_POINT('Ctrl Pts',(-0.483067165018363,-0.640161874114352,
-2.41519419633098));
#66248=CARTESIAN_POINT('Ctrl Pts',(-0.573459792402489,-0.545059311424541,
-2.42047490080706));
#66249=CARTESIAN_POINT('Ctrl Pts',(-0.663852419786615,-0.449956748734731,
-2.42575560528314));
#66250=CARTESIAN_POINT('Ctrl Pts',(-0.730078110366975,-0.331884111929841,
-2.43103630975922));
#66251=CARTESIAN_POINT('Ctrl Pts',(-0.764102725102462,-0.205165328366884,
-2.43631701423529));
#66252=CARTESIAN_POINT('Ctrl Pts',(-0.782035933210049,-0.138376201305743,
-2.43910029254896));
#66253=CARTESIAN_POINT('Ctrl Pts',(-0.791023738008576,-0.0691851895935175,
-2.44188357086263));
#66254=CARTESIAN_POINT('Ctrl Pts',(-0.79103374865932,3.27018256038314E-6,
-2.4446668491763));
#66255=CARTESIAN_POINT('Ctrl Pts',(-0.791033002877254,-8.32524903205056E-7,
-2.47313315082371));
#66256=CARTESIAN_POINT('Ctrl Pts',(-0.79103538462277,-0.0647355625419663,
-2.47052904188561));
#66257=CARTESIAN_POINT('Ctrl Pts',(-0.783179328184073,-0.129469724503196,
-2.46792493294751));
#66258=CARTESIAN_POINT('Ctrl Pts',(-0.767458105990247,-0.192233810480545,
-2.46532082400941));
#66259=CARTESIAN_POINT('Ctrl Pts',(-0.73557805397176,-0.319509050355758,
-2.46004011953334));
#66260=CARTESIAN_POINT('Ctrl Pts',(-0.671355522510494,-0.438683107879184,
-2.45475941505726));
#66261=CARTESIAN_POINT('Ctrl Pts',(-0.582581638325029,-0.535298437349069,
-2.44947871058118));
#66262=CARTESIAN_POINT('Ctrl Pts',(-0.493807754139564,-0.631913766818955,
-2.4441980061051));
#66263=CARTESIAN_POINT('Ctrl Pts',(-0.380482517229898,-0.705970368235301,
-2.43891730162902));
#66264=CARTESIAN_POINT('Ctrl Pts',(-0.256353926329107,-0.748484099228321,
-2.43363659715294));
#66265=CARTESIAN_POINT('Ctrl Pts',(-0.132225335428317,-0.790997830221342,
-2.42835589267686));
#66266=CARTESIAN_POINT('Ctrl Pts',(0.00270660946359702,-0.801968690791038,
-2.42307518820079));
#66267=CARTESIAN_POINT('Ctrl Pts',(0.132072701821953,-0.780065756058642,
-2.41779448372471));
#66268=CARTESIAN_POINT('Ctrl Pts',(0.261438794180308,-0.758162821326247,
-2.41251377924863));
#66269=CARTESIAN_POINT('Ctrl Pts',(0.385239034005103,-0.703386091291759,
-2.40723307477255));
#66270=CARTESIAN_POINT('Ctrl Pts',(0.488454652426469,-0.622380779639659,
-2.40195237029647));
#66271=CARTESIAN_POINT('Ctrl Pts',(0.591670270847835,-0.541375467987559,
-2.39667166582039));
#66272=CARTESIAN_POINT('Ctrl Pts',(0.674301267865773,-0.434141574717848,
-2.39139096134431));
#66273=CARTESIAN_POINT('Ctrl Pts',(0.726323302271758,-0.313688130025617,
-2.38611025686824));
#66274=CARTESIAN_POINT('Ctrl Pts',(0.778345336677742,-0.193234685333386,
-2.38082955239216));
#66275=CARTESIAN_POINT('Ctrl Pts',(0.799758408471774,-0.0595616892186328,
-2.37554884791608));
#66276=CARTESIAN_POINT('Ctrl Pts',(0.787964800746976,0.0711143805829716,
-2.37026814344));
#66277=CARTESIAN_POINT('Ctrl Pts',(0.776171193022177,0.201790450384576,
-2.36498743896392));
#66278=CARTESIAN_POINT('Ctrl Pts',(0.731170905778547,0.329469593873033,
-2.35970673448784));
#66279=CARTESIAN_POINT('Ctrl Pts',(0.658423128062463,0.438662474773447,
-2.35442603001176));
#66280=CARTESIAN_POINT('Ctrl Pts',(0.585675350346377,0.547855355673862,
-2.34914532553569));
#66281=CARTESIAN_POINT('Ctrl Pts',(0.485180082157836,0.638561973986235,
-2.34386462105961));
#66282=CARTESIAN_POINT('Ctrl Pts',(0.369128860504978,0.699778298237532,
-2.33858391658353));
#66283=CARTESIAN_POINT('Ctrl Pts',(0.253077638852122,0.760994622488829,
-2.33330321210745));
#66284=CARTESIAN_POINT('Ctrl Pts',(0.121470463734948,0.79272065267905,-2.32802250763137));
#66285=CARTESIAN_POINT('Ctrl Pts',(-0.00972680123028606,0.791107560120461,
-2.32274180315529));
#66286=CARTESIAN_POINT('Ctrl Pts',(-0.140924066195523,0.789494467561872,
-2.31746109867922));
#66287=CARTESIAN_POINT('Ctrl Pts',(-0.271711421008817,0.754542252254472,
-2.31218039420314));
#66288=CARTESIAN_POINT('Ctrl Pts',(-0.386222458175134,0.690491126042238,
-2.30689968972706));
#66289=CARTESIAN_POINT('Ctrl Pts',(-0.500733495341449,0.626439999830005,
-2.30161898525098));
#66290=CARTESIAN_POINT('Ctrl Pts',(-0.598968214860784,0.533289962712938,
-2.2963382807749));
#66291=CARTESIAN_POINT('Ctrl Pts',(-0.669009317141909,0.422341468386942,
-2.29105757629882));
#66292=CARTESIAN_POINT('Ctrl Pts',(-0.739050419423034,0.311392974060945,
-2.28577687182274));
#66293=CARTESIAN_POINT('Ctrl Pts',(-0.780897904465948,0.182646022526017,
-2.28049616734667));
#66294=CARTESIAN_POINT('Ctrl Pts',(-0.789475063965926,0.0517194906966256,
-2.27521546287059));
#66295=CARTESIAN_POINT('Ctrl Pts',(-0.79060245916075,0.0345103035689084,
-2.27452135885496));
#66296=CARTESIAN_POINT('Ctrl Pts',(-0.791155046841484,0.0172634600879581,
-2.27382725483933));
#66297=CARTESIAN_POINT('Ctrl Pts',(-0.791139629808145,1.56300862382004E-5,
-2.27313315082371));
#66298=CARTESIAN_POINT('Origin',(0.,0.,-1.425));
#66299=CARTESIAN_POINT('',(-0.791081097997334,-1.97830511448061E-5,-2.0446668491763));
#66300=CARTESIAN_POINT('',(-0.791094572033932,-2.03193093578051E-5,-2.07313315082371));
#66301=CARTESIAN_POINT('',(-0.7911,-9.68818082805471E-17,-1.425));
#66302=CARTESIAN_POINT('Ctrl Pts',(-0.791081097997334,-1.9783051144806E-5,
-2.0446668491763));
#66303=CARTESIAN_POINT('Ctrl Pts',(-0.790990817900606,0.0947535438784193,
-2.04847999677008));
#66304=CARTESIAN_POINT('Ctrl Pts',(-0.773944248118208,0.189558474775009,
-2.05229314436386));
#66305=CARTESIAN_POINT('Ctrl Pts',(-0.740623479673775,0.278249254857598,
-2.05610629195765));
#66306=CARTESIAN_POINT('Ctrl Pts',(-0.69447862775203,0.401074240738709,
-2.06138699643373));
#66307=CARTESIAN_POINT('Ctrl Pts',(-0.617122170298751,0.512173152277855,
-2.0666677009098));
#66308=CARTESIAN_POINT('Ctrl Pts',(-0.51793857019323,0.598068076375167,
-2.07194840538588));
#66309=CARTESIAN_POINT('Ctrl Pts',(-0.41875497008771,0.683963000472479,
-2.07722910986196));
#66310=CARTESIAN_POINT('Ctrl Pts',(-0.297744227329949,0.744653937127956,
-2.08250981433804));
#66311=CARTESIAN_POINT('Ctrl Pts',(-0.169586704242536,0.772778193414549,
-2.08779051881412));
#66312=CARTESIAN_POINT('Ctrl Pts',(-0.0414291811551249,0.800902449701142,
-2.0930712232902));
#66313=CARTESIAN_POINT('Ctrl Pts',(0.0938751222619378,0.796460025618851,
-2.09835192776627));
#66314=CARTESIAN_POINT('Ctrl Pts',(0.219911826981627,0.759989851791787,
-2.10363263224235));
#66315=CARTESIAN_POINT('Ctrl Pts',(0.345948531701318,0.723519677964723,
-2.10891333671843));
#66316=CARTESIAN_POINT('Ctrl Pts',(0.462717637723634,0.655021754392886,
-2.11419404119451));
#66317=CARTESIAN_POINT('Ctrl Pts',(0.556053354925926,0.562805875012443,
-2.11947474567059));
#66318=CARTESIAN_POINT('Ctrl Pts',(0.649389072128219,0.470589995632,-2.12475545014667));
#66319=CARTESIAN_POINT('Ctrl Pts',(0.719291400510487,0.354656160442951,
-2.13003615462275));
#66320=CARTESIAN_POINT('Ctrl Pts',(0.757280171416149,0.229068829072896,
-2.13531685909882));
#66321=CARTESIAN_POINT('Ctrl Pts',(0.79526894232181,0.103481497702842,-2.1405975635749));
#66322=CARTESIAN_POINT('Ctrl Pts',(0.801344155750865,-0.0317593298482181,
-2.14587826805098));
#66323=CARTESIAN_POINT('Ctrl Pts',(0.774768799994326,-0.160246975098601,
-2.15115897252706));
#66324=CARTESIAN_POINT('Ctrl Pts',(0.748193444237787,-0.288734620348983,
-2.15643967700314));
#66325=CARTESIAN_POINT('Ctrl Pts',(0.688967519295655,-0.410469083298688,
-2.16172038147922));
#66326=CARTESIAN_POINT('Ctrl Pts',(0.604275990876151,-0.510682203844568,
-2.1670010859553));
#66327=CARTESIAN_POINT('Ctrl Pts',(0.519584462456648,-0.610895324390448,
-2.17228179043137));
#66328=CARTESIAN_POINT('Ctrl Pts',(0.409427330559771,-0.689587102532504,
-2.17756249490745));
#66329=CARTESIAN_POINT('Ctrl Pts',(0.287168256723413,-0.737211081579309,
-2.18284319938353));
#66330=CARTESIAN_POINT('Ctrl Pts',(0.164909182887057,-0.784835060626115,
-2.18812390385961));
#66331=CARTESIAN_POINT('Ctrl Pts',(0.0305481671112177,-0.801391240577672,
-2.19340460833569));
#66332=CARTESIAN_POINT('Ctrl Pts',(-0.0996148460812547,-0.784871116115957,
-2.19868531281176));
#66333=CARTESIAN_POINT('Ctrl Pts',(-0.229777859273729,-0.768350991654242,
-2.20396601728784));
#66334=CARTESIAN_POINT('Ctrl Pts',(-0.355742869882836,-0.718754562779255,
-2.20924672176392));
#66335=CARTESIAN_POINT('Ctrl Pts',(-0.462228490871624,-0.642098597334895,
-2.21452742624));
#66336=CARTESIAN_POINT('Ctrl Pts',(-0.568714111860411,-0.565442631890537,
-2.21980813071608));
#66337=CARTESIAN_POINT('Ctrl Pts',(-0.65572034322888,-0.461727129876807,
-2.22508883519216));
#66338=CARTESIAN_POINT('Ctrl Pts',(-0.712692064235652,-0.343534289479849,
-2.23036953966824));
#66339=CARTESIAN_POINT('Ctrl Pts',(-0.764108330892919,-0.236866727197373,
-2.23513530950426));
#66340=CARTESIAN_POINT('Ctrl Pts',(-0.791061978227509,-0.118407608688093,
-2.23990107934028));
#66341=CARTESIAN_POINT('Ctrl Pts',(-0.791150917366707,1.23845276237822E-5,
-2.2446668491763));
#66342=CARTESIAN_POINT('Ctrl Pts',(-0.791139629808145,1.56300862382004E-5,
-2.27313315082371));
#66343=CARTESIAN_POINT('Ctrl Pts',(-0.791037754915302,-0.113957064562566,
-2.26854655036325));
#66344=CARTESIAN_POINT('Ctrl Pts',(-0.766133997457558,-0.227972835565614,
-2.2639599499028));
#66345=CARTESIAN_POINT('Ctrl Pts',(-0.718391205861583,-0.331451139208576,
-2.25937334944235));
#66346=CARTESIAN_POINT('Ctrl Pts',(-0.663423354300215,-0.450589125160531,
-2.25409264496627));
#66347=CARTESIAN_POINT('Ctrl Pts',(-0.578180817220436,-0.555758984940586,
-2.2488119404902));
#66348=CARTESIAN_POINT('Ctrl Pts',(-0.473004753606229,-0.634202085622424,
-2.24353123601412));
#66349=CARTESIAN_POINT('Ctrl Pts',(-0.367828689992021,-0.712645186304262,
-2.23825053153804));
#66350=CARTESIAN_POINT('Ctrl Pts',(-0.242719099843387,-0.764361527887883,
-2.23296982706196));
#66351=CARTESIAN_POINT('Ctrl Pts',(-0.112853595259514,-0.783077166299033,
-2.22768912258588));
#66352=CARTESIAN_POINT('Ctrl Pts',(0.0170119093243585,-0.801792804710183,
-2.22240841810981));
#66353=CARTESIAN_POINT('Ctrl Pts',(0.151633328343468,-0.787507739948862,
-2.21712771363373));
#66354=CARTESIAN_POINT('Ctrl Pts',(0.274679126575874,-0.741954958043571,
-2.21184700915765));
#66355=CARTESIAN_POINT('Ctrl Pts',(0.397724924808278,-0.69640217613828,
-2.20656630468157));
#66356=CARTESIAN_POINT('Ctrl Pts',(0.509195102253979,-0.619581677089019,
-2.20128560020549));
#66357=CARTESIAN_POINT('Ctrl Pts',(0.595566705861264,-0.520812904229037,
-2.19600489572941));
#66358=CARTESIAN_POINT('Ctrl Pts',(0.681938309468549,-0.422044131369055,
-2.19072419125333));
#66359=CARTESIAN_POINT('Ctrl Pts',(0.743211339237417,-0.30132708469835,
-2.18544348677726));
#66360=CARTESIAN_POINT('Ctrl Pts',(0.77195248588383,-0.173306496934467,
-2.18016278230118));
#66361=CARTESIAN_POINT('Ctrl Pts',(0.800693632530243,-0.0452859091705829,
-2.1748820778251));
#66362=CARTESIAN_POINT('Ctrl Pts',(0.7969028960542,0.0900382196864831,-2.16960137334902));
#66363=CARTESIAN_POINT('Ctrl Pts',(0.761040147899091,0.216249105495609,
-2.16432066887294));
#66364=CARTESIAN_POINT('Ctrl Pts',(0.725177399743983,0.342459991304734,
-2.15903996439686));
#66365=CARTESIAN_POINT('Ctrl Pts',(0.65724263990981,0.45955763406592,-2.15375925992079));
#66366=CARTESIAN_POINT('Ctrl Pts',(0.565477342384216,0.553336387373906,
-2.14847855544471));
#66367=CARTESIAN_POINT('Ctrl Pts',(0.473712044858623,0.647115140681891,
-2.14319785096863));
#66368=CARTESIAN_POINT('Ctrl Pts',(0.358116209641609,0.717575004536675,
-2.13791714649255));
#66369=CARTESIAN_POINT('Ctrl Pts',(0.232713292050402,0.756168173123536,
-2.13263644201647));
#66370=CARTESIAN_POINT('Ctrl Pts',(0.107310374459195,0.794761341710397,
-2.12735573754039));
#66371=CARTESIAN_POINT('Ctrl Pts',(-0.0278996255061993,0.801487815029334,
-2.12207503306431));
#66372=CARTESIAN_POINT('Ctrl Pts',(-0.156513769198413,0.775531574078856,
-2.11679432858824));
#66373=CARTESIAN_POINT('Ctrl Pts',(-0.285127912890625,0.749575333128377,
-2.11151362411216));
#66374=CARTESIAN_POINT('Ctrl Pts',(-0.407146200309654,0.690936377908482,
-2.10623291963608));
#66375=CARTESIAN_POINT('Ctrl Pts',(-0.507766039318046,0.606728466166857,
-2.10095221516));
#66376=CARTESIAN_POINT('Ctrl Pts',(-0.60838587832644,0.522520554425229,
-2.09567151068392));
#66377=CARTESIAN_POINT('Ctrl Pts',(-0.687607268924199,0.412743686161869,
-2.09039080620784));
#66378=CARTESIAN_POINT('Ctrl Pts',(-0.735819504729637,0.290715391407736,
-2.08511010173177));
#66379=CARTESIAN_POINT('Ctrl Pts',(-0.772268908025816,0.198459588399807,
-2.08111778476241));
#66380=CARTESIAN_POINT('Ctrl Pts',(-0.790994536208493,0.0992012879231028,
-2.07712546779306));
#66381=CARTESIAN_POINT('Ctrl Pts',(-0.791094572033932,-2.03193093578051E-5,
-2.07313315082371));
#66382=CARTESIAN_POINT('Origin',(0.,0.,-1.425));
#66383=CARTESIAN_POINT('',(-0.791057251695019,1.61679271216408E-5,-1.8446668491763));
#66384=CARTESIAN_POINT('',(-0.79104797996428,1.33236467988428E-5,-1.87313315082371));
#66385=CARTESIAN_POINT('',(-0.7911,-9.68818082805471E-17,-1.425));
#66386=CARTESIAN_POINT('Ctrl Pts',(-0.791057251695019,1.61679271216408E-5,
-1.8446668491763));
#66387=CARTESIAN_POINT('Ctrl Pts',(-0.791091088198568,0.0455198809875166,
-1.84649750524773));
#66388=CARTESIAN_POINT('Ctrl Pts',(-0.787229605616998,0.0910179144373288,
-1.84832816131916));
#66389=CARTESIAN_POINT('Ctrl Pts',(-0.779420639490756,0.135828028067558,
-1.85015881739059));
#66390=CARTESIAN_POINT('Ctrl Pts',(-0.756894921514591,0.265087134304733,
-1.85543952186667));
#66391=CARTESIAN_POINT('Ctrl Pts',(-0.701522594957182,0.388622129777778,
-1.86072022634275));
#66392=CARTESIAN_POINT('Ctrl Pts',(-0.620021128019969,0.491446423612732,
-1.86600093081882));
#66393=CARTESIAN_POINT('Ctrl Pts',(-0.538519661082756,0.594270717447687,
-1.8712816352949));
#66394=CARTESIAN_POINT('Ctrl Pts',(-0.430889053765737,0.676384309644556,
-1.87656233977098));
#66395=CARTESIAN_POINT('Ctrl Pts',(-0.310186463445237,0.727825627721529,
-1.88184304424706));
#66396=CARTESIAN_POINT('Ctrl Pts',(-0.18948387312474,0.7792669457985,-1.88712374872314));
#66397=CARTESIAN_POINT('Ctrl Pts',(-0.0557092998007569,0.800035989755576,
-1.89240445319922));
#66398=CARTESIAN_POINT('Ctrl Pts',(0.0749084559988265,0.787613172625225,
-1.8976851576753));
#66399=CARTESIAN_POINT('Ctrl Pts',(0.205526211798415,0.775190355494874,
-1.90296586215137));
#66400=CARTESIAN_POINT('Ctrl Pts',(0.332987150073606,0.729575677277096,
-1.90824656662745));
#66401=CARTESIAN_POINT('Ctrl Pts',(0.44182840601411,0.656302861575303,-1.91352727110353));
#66402=CARTESIAN_POINT('Ctrl Pts',(0.550669661954614,0.58303004587351,-1.91880797557961));
#66403=CARTESIAN_POINT('Ctrl Pts',(0.640891235560426,0.482099092687703,
-1.92408868005569));
#66404=CARTESIAN_POINT('Ctrl Pts',(0.70154793833288,0.365754393950074,-1.92936938453177));
#66405=CARTESIAN_POINT('Ctrl Pts',(0.762204641105332,0.249409695212449,
-1.93465008900784));
#66406=CARTESIAN_POINT('Ctrl Pts',(0.793296473044426,0.117651250923005,
-1.93993079348392));
#66407=CARTESIAN_POINT('Ctrl Pts',(0.791051542930121,-0.01353672415229,
-1.94521149796));
#66408=CARTESIAN_POINT('Ctrl Pts',(0.788806612815815,-0.144724699227588,
-1.95049220243608));
#66409=CARTESIAN_POINT('Ctrl Pts',(0.753224920648107,-0.275342205088737,
-1.95577290691216));
#66410=CARTESIAN_POINT('Ctrl Pts',(0.688623042965317,-0.389543439387815,
-1.96105361138824));
#66411=CARTESIAN_POINT('Ctrl Pts',(0.624021165282528,-0.503744673686888,
-1.96633431586431));
#66412=CARTESIAN_POINT('Ctrl Pts',(0.530399102084659,-0.601529636423893,
-1.97161502034039));
#66413=CARTESIAN_POINT('Ctrl Pts',(0.419114570693421,-0.671035590043754,
-1.97689572481647));
#66414=CARTESIAN_POINT('Ctrl Pts',(0.30783003930218,-0.740541543663617,
-1.98217642929255));
#66415=CARTESIAN_POINT('Ctrl Pts',(0.178883039717568,-0.781768488166335,
-1.98745713376863));
#66416=CARTESIAN_POINT('Ctrl Pts',(0.0479167175907291,-0.789714995835985,
-1.99273783824471));
#66417=CARTESIAN_POINT('Ctrl Pts',(-0.0830496045361099,-0.797661503505635,
-1.99801854272078));
#66418=CARTESIAN_POINT('Ctrl Pts',(-0.216035249205176,-0.772327574342217,
-2.00329924719686));
#66419=CARTESIAN_POINT('Ctrl Pts',(-0.334907124403696,-0.716786582252031,
-2.00857995167294));
#66420=CARTESIAN_POINT('Ctrl Pts',(-0.453778999602217,-0.661245590161845,
-2.01386065614902));
#66421=CARTESIAN_POINT('Ctrl Pts',(-0.558537105330192,-0.575497535144891,
-2.0191413606251));
#66422=CARTESIAN_POINT('Ctrl Pts',(-0.636472760413809,-0.469944902860034,
-2.02442206510118));
#66423=CARTESIAN_POINT('Ctrl Pts',(-0.714408415497425,-0.364392270575176,
-2.02970276957726));
#66424=CARTESIAN_POINT('Ctrl Pts',(-0.765521619936684,-0.239035061022416,
-2.03498347405333));
#66425=CARTESIAN_POINT('Ctrl Pts',(-0.783611598961207,-0.109080926134498,
-2.04026417852941));
#66426=CARTESIAN_POINT('Ctrl Pts',(-0.788638972361532,-0.0729654635288157,
-2.04173173541171));
#66427=CARTESIAN_POINT('Ctrl Pts',(-0.791115843879582,-0.0364949639280258,
-2.043199292294));
#66428=CARTESIAN_POINT('Ctrl Pts',(-0.791081097997334,-1.9783051144806E-5,
-2.0446668491763));
#66429=CARTESIAN_POINT('Ctrl Pts',(-0.791094572033932,-2.03193093578051E-5,
-2.07313315082371));
#66430=CARTESIAN_POINT('Ctrl Pts',(-0.791126855269133,-0.0320407926677618,
-2.07184476331698));
#66431=CARTESIAN_POINT('Ctrl Pts',(-0.789219355838881,-0.0640574445681548,
-2.07055637581026));
#66432=CARTESIAN_POINT('Ctrl Pts',(-0.785341763947706,-0.0958336900125776,
-2.06926798830353));
#66433=CARTESIAN_POINT('Ctrl Pts',(-0.769448706347217,-0.226074755433851,
-2.06398728382745));
#66434=CARTESIAN_POINT('Ctrl Pts',(-0.720459510133122,-0.352277165031491,
-2.05870657935137));
#66435=CARTESIAN_POINT('Ctrl Pts',(-0.644317276999745,-0.459130731819986,
-2.05342587487529));
#66436=CARTESIAN_POINT('Ctrl Pts',(-0.568175043866367,-0.565984298608481,
-2.04814517039922));
#66437=CARTESIAN_POINT('Ctrl Pts',(-0.464879773813709,-0.65348902258783,
-2.04286446592314));
#66438=CARTESIAN_POINT('Ctrl Pts',(-0.346962684781801,-0.711029308615985,
-2.03758376144706));
#66439=CARTESIAN_POINT('Ctrl Pts',(-0.229045595749893,-0.768569594644141,
-2.03230305697098));
#66440=CARTESIAN_POINT('Ctrl Pts',(-0.0965066877387357,-0.796145442721103,
-2.0270223524949));
#66441=CARTESIAN_POINT('Ctrl Pts',(0.0345751428900571,-0.790411501583861,
-2.02174164801882));
#66442=CARTESIAN_POINT('Ctrl Pts',(0.16565697351885,-0.784677560446619,
-2.01646094354275));
#66443=CARTESIAN_POINT('Ctrl Pts',(0.295281726765278,-0.745633830095173,
-2.01118023906667));
#66444=CARTESIAN_POINT('Ctrl Pts',(0.407724035605994,-0.678016882629838,
-2.00589953459059));
#66445=CARTESIAN_POINT('Ctrl Pts',(0.520166344446709,-0.610399935164503,
-2.00061883011451));
#66446=CARTESIAN_POINT('Ctrl Pts',(0.615426208881714,-0.514209770585277,
-1.99533812563843));
#66447=CARTESIAN_POINT('Ctrl Pts',(0.681947222489256,-0.401115654245894,
-1.99005742116235));
#66448=CARTESIAN_POINT('Ctrl Pts',(0.748468236096796,-0.288021537906514,
-1.98477671668627));
#66449=CARTESIAN_POINT('Ctrl Pts',(0.786250398876875,-0.158023469806975,
-1.9794960122102));
#66450=CARTESIAN_POINT('Ctrl Pts',(0.790710185215964,-0.0268921054894726,
-1.97421530773412));
#66451=CARTESIAN_POINT('Ctrl Pts',(0.795169971555054,0.104239258828034,
-1.96893460325804));
#66452=CARTESIAN_POINT('Ctrl Pts',(0.76630738145315,0.236503919363504,-1.96365389878196));
#66453=CARTESIAN_POINT('Ctrl Pts',(0.707623866687246,0.353856249961072,
-1.95837319430588));
#66454=CARTESIAN_POINT('Ctrl Pts',(0.648940351921342,0.471208580558639,
-1.9530924898298));
#66455=CARTESIAN_POINT('Ctrl Pts',(0.560435912491437,0.573648581218303,
-1.94781178535373));
#66456=CARTESIAN_POINT('Ctrl Pts',(0.452847423557364,0.648748790611111,
-1.94253108087765));
#66457=CARTESIAN_POINT('Ctrl Pts',(0.34525893462329,0.723849000003919,-1.93725037640157));
#66458=CARTESIAN_POINT('Ctrl Pts',(0.218586396185047,0.77160941812987,-1.93196967192549));
#66459=CARTESIAN_POINT('Ctrl Pts',(0.0881970286911367,0.78623601194042,
-1.92668896744941));
#66460=CARTESIAN_POINT('Ctrl Pts',(-0.0421923388027758,0.800862605750971,
-1.92140826297333));
#66461=CARTESIAN_POINT('Ctrl Pts',(-0.176298535352356,0.78235537524612,
-1.91612755849726));
#66462=CARTESIAN_POINT('Ctrl Pts',(-0.297852529711402,0.732959516539925,
-1.91084685402118));
#66463=CARTESIAN_POINT('Ctrl Pts',(-0.419406524070446,0.68356365783373,
-1.9055661495451));
#66464=CARTESIAN_POINT('Ctrl Pts',(-0.528408316238956,0.603279170926192,
-1.90028544506902));
#66465=CARTESIAN_POINT('Ctrl Pts',(-0.611634404184154,0.501845731236419,
-1.89500474059294));
#66466=CARTESIAN_POINT('Ctrl Pts',(-0.69486049212935,0.400412291546648,
-1.88972403611686));
#66467=CARTESIAN_POINT('Ctrl Pts',(-0.752310875851237,0.277829899074643,
-1.88444333164079));
#66468=CARTESIAN_POINT('Ctrl Pts',(-0.777015988604014,0.148969580101607,
-1.87916262716471));
#66469=CARTESIAN_POINT('Ctrl Pts',(-0.786418704568611,0.0999256032318913,
-1.87715280171771));
#66470=CARTESIAN_POINT('Ctrl Pts',(-0.791078110168372,0.0499722384426156,
-1.87514297627071));
#66471=CARTESIAN_POINT('Ctrl Pts',(-0.79104797996428,1.33236467988428E-5,
-1.87313315082371));
#66472=CARTESIAN_POINT('Origin',(0.,0.,-1.425));
#66473=CARTESIAN_POINT('',(-0.791165709393907,-3.94338443360231E-6,-1.6446668491763));
#66474=CARTESIAN_POINT('',(-0.791167324336245,7.15608088368358E-7,-1.6731331508237));
#66475=CARTESIAN_POINT('',(-0.7911,-9.68818082805471E-17,-1.425));
#66476=CARTESIAN_POINT('Ctrl Pts',(-0.791165709393907,-3.94338443360232E-6,
-1.6446668491763));
#66477=CARTESIAN_POINT('Ctrl Pts',(-0.791130303728021,0.127431427810519,
-1.64979571820145));
#66478=CARTESIAN_POINT('Ctrl Pts',(-0.759749767008419,0.254883610031654,
-1.65492458722661));
#66479=CARTESIAN_POINT('Ctrl Pts',(-0.700520896362271,0.367717636553784,
-1.66005345625176));
#66480=CARTESIAN_POINT('Ctrl Pts',(-0.639538609468196,0.483892010667631,
-1.66533416072784));
#66481=CARTESIAN_POINT('Ctrl Pts',(-0.549034733691348,0.584569903594896,
-1.67061486520392));
#66482=CARTESIAN_POINT('Ctrl Pts',(-0.439988704887787,0.657537623291678,
-1.67589556968));
#66483=CARTESIAN_POINT('Ctrl Pts',(-0.330942676084231,0.730505342988456,
-1.68117627415608));
#66484=CARTESIAN_POINT('Ctrl Pts',(-0.203354494253961,0.775762889454755,
-1.68645697863216));
#66485=CARTESIAN_POINT('Ctrl Pts',(-0.0727024607003433,0.787819864360512,
-1.69173768310824));
#66486=CARTESIAN_POINT('Ctrl Pts',(0.0579495728532782,0.79987683926627,
-1.69701838758431));
#66487=CARTESIAN_POINT('Ctrl Pts',(0.191665458130249,0.778733242611484,
-1.70229909206039));
#66488=CARTESIAN_POINT('Ctrl Pts',(0.312223514315988,0.726954100051079,
-1.70757979653647));
#66489=CARTESIAN_POINT('Ctrl Pts',(0.432781570501728,0.675174957490674,
-1.71286050101255));
#66490=CARTESIAN_POINT('Ctrl Pts',(0.540181797596237,0.592760269024648,
-1.71814120548863));
#66491=CARTESIAN_POINT('Ctrl Pts',(0.621394986693395,0.48970813448953,-1.72342190996471));
#66492=CARTESIAN_POINT('Ctrl Pts',(0.702608175790553,0.386655999954413,
-1.72870261444078));
#66493=CARTESIAN_POINT('Ctrl Pts',(0.75763432689036,0.262966419350202,-1.73398331891686));
#66494=CARTESIAN_POINT('Ctrl Pts',(0.779797967907005,0.133644736974585,
-1.73926402339294));
#66495=CARTESIAN_POINT('Ctrl Pts',(0.80196160892365,0.00432305459896595,
-1.74454472786902));
#66496=CARTESIAN_POINT('Ctrl Pts',(0.791262739857134,-0.130630729548055,
-1.7498254323451));
#66497=CARTESIAN_POINT('Ctrl Pts',(0.748999289062897,-0.254844759522685,
-1.75510613682118));
#66498=CARTESIAN_POINT('Ctrl Pts',(0.706735838268662,-0.379058789497312,
-1.76038684129725));
#66499=CARTESIAN_POINT('Ctrl Pts',(0.632907805746706,-0.492533065299543,
-1.76566754577333));
#66500=CARTESIAN_POINT('Ctrl Pts',(0.536471605136735,-0.581501507611902,
-1.77094825024941));
#66501=CARTESIAN_POINT('Ctrl Pts',(0.440035404526762,-0.670469949924263,
-1.77622895472549));
#66502=CARTESIAN_POINT('Ctrl Pts',(0.320991035828772,-0.734932558746751,
-1.78150965920157));
#66503=CARTESIAN_POINT('Ctrl Pts',(0.193780311605213,-0.767069082486765,
-1.78679036367765));
#66504=CARTESIAN_POINT('Ctrl Pts',(0.0665695873816547,-0.799205606226778,
-1.79207106815373));
#66505=CARTESIAN_POINT('Ctrl Pts',(-0.0688074923674732,-0.799016044884316,
-1.7973517726298));
#66506=CARTESIAN_POINT('Ctrl Pts',(-0.195927719788058,-0.766523395006019,
-1.80263247710588));
#66507=CARTESIAN_POINT('Ctrl Pts',(-0.32304794720864,-0.734030745127722,
-1.80791318158196));
#66508=CARTESIAN_POINT('Ctrl Pts',(-0.441911322300681,-0.66923500671359,
-1.81319388605804));
#66509=CARTESIAN_POINT('Ctrl Pts',(-0.538097989657374,-0.579996844818653,
-1.81847459053412));
#66510=CARTESIAN_POINT('Ctrl Pts',(-0.63428465701407,-0.490758682923715,
-1.8237552950102));
#66511=CARTESIAN_POINT('Ctrl Pts',(-0.707794616635418,-0.37707809754797,
-1.82903599948627));
#66512=CARTESIAN_POINT('Ctrl Pts',(-0.749710041748631,-0.252746196359444,
-1.83431670396235));
#66513=CARTESIAN_POINT('Ctrl Pts',(-0.777094692072668,-0.171516299991357,
-1.837766752367));
#66514=CARTESIAN_POINT('Ctrl Pts',(-0.790993483531841,-0.0857399798821861,
-1.84121680077165));
#66515=CARTESIAN_POINT('Ctrl Pts',(-0.791057251695019,1.61679271216408E-5,
-1.8446668491763));
#66516=CARTESIAN_POINT('Ctrl Pts',(-0.79104797996428,1.33236467988428E-5,
-1.87313315082371));
#66517=CARTESIAN_POINT('Ctrl Pts',(-0.790998944734453,-0.0812920289971471,
-1.86986227179463));
#66518=CARTESIAN_POINT('Ctrl Pts',(-0.778529321983252,-0.162612081249939,
-1.86659139276555));
#66519=CARTESIAN_POINT('Ctrl Pts',(-0.753870902032603,-0.240050922536179,
-1.86332051373647));
#66520=CARTESIAN_POINT('Ctrl Pts',(-0.714060860924751,-0.365072860726848,
-1.85803980926039));
#66521=CARTESIAN_POINT('Ctrl Pts',(-0.642480936925383,-0.479978491634118,
-1.85275910478431));
#66522=CARTESIAN_POINT('Ctrl Pts',(-0.547814815427932,-0.570828091757565,
-1.84747840030824));
#66523=CARTESIAN_POINT('Ctrl Pts',(-0.45314869393048,-0.661677691881011,
-1.84219769583216));
#66524=CARTESIAN_POINT('Ctrl Pts',(-0.335396374934945,-0.728471261220633,
-1.83691699135608));
#66525=CARTESIAN_POINT('Ctrl Pts',(-0.208842926591348,-0.763105768786138,
-1.83163628688));
#66526=CARTESIAN_POINT('Ctrl Pts',(-0.0822894782477499,-0.797740276351643,
-1.82635558240392));
#66527=CARTESIAN_POINT('Ctrl Pts',(0.0530650994439101,-0.80021572214303,
-1.82107487792784));
#66528=CARTESIAN_POINT('Ctrl Pts',(0.180800328456221,-0.770231798598347,
-1.81579417345177));
#66529=CARTESIAN_POINT('Ctrl Pts',(0.308535557468532,-0.740247875053664,
-1.81051346897569));
#66530=CARTESIAN_POINT('Ctrl Pts',(0.428651437801493,-0.677804582172911,
-1.80523276449961));
#66531=CARTESIAN_POINT('Ctrl Pts',(0.526576166953947,-0.590477199168613,
-1.79995206002353));
#66532=CARTESIAN_POINT('Ctrl Pts',(0.624500896106401,-0.503149816164315,
-1.79467135554745));
#66533=CARTESIAN_POINT('Ctrl Pts',(0.700234474078348,-0.390938343036472,
-1.78939065107137));
#66534=CARTESIAN_POINT('Ctrl Pts',(0.744589316864623,-0.267455662779823,
-1.78410994659529));
#66535=CARTESIAN_POINT('Ctrl Pts',(0.788944159650899,-0.143972982523175,
-1.77882924211922));
#66536=CARTESIAN_POINT('Ctrl Pts',(0.801920267251505,-0.00921909513772246,
-1.77354853764314));
#66537=CARTESIAN_POINT('Ctrl Pts',(0.781943449170847,0.120458393815963,
-1.76826783316706));
#66538=CARTESIAN_POINT('Ctrl Pts',(0.761966631090189,0.250135882769648,
-1.76298712869098));
#66539=CARTESIAN_POINT('Ctrl Pts',(0.709036887328268,0.374736973291566,
-1.7577064242149));
#66540=CARTESIAN_POINT('Ctrl Pts',(0.629575365283726,0.479145741679694,
-1.75242571973882));
#66541=CARTESIAN_POINT('Ctrl Pts',(0.550113843239185,0.583554510067822,
-1.74714501526275));
#66542=CARTESIAN_POINT('Ctrl Pts',(0.444120542912024,0.66777095632216,-1.74186431078667));
#66543=CARTESIAN_POINT('Ctrl Pts',(0.324453992537908,0.721578401192921,
-1.73658360631059));
#66544=CARTESIAN_POINT('Ctrl Pts',(0.204787442163794,0.775385846063682,
-1.73130290183451));
#66545=CARTESIAN_POINT('Ctrl Pts',(0.0714476417427256,0.798784289550868,
-1.72602219735843));
#66546=CARTESIAN_POINT('Ctrl Pts',(-0.059389352471172,0.788935160298346,
-1.72074149288235));
#66547=CARTESIAN_POINT('Ctrl Pts',(-0.19022634668507,0.779086031045823,
-1.71546078840628));
#66548=CARTESIAN_POINT('Ctrl Pts',(-0.318560534691797,0.735989329053593,
-1.7101800839302));
#66549=CARTESIAN_POINT('Ctrl Pts',(-0.428823113793521,0.664873310803156,
-1.70489937945412));
#66550=CARTESIAN_POINT('Ctrl Pts',(-0.539085692895245,0.59375729255272,
-1.69961867497804));
#66551=CARTESIAN_POINT('Ctrl Pts',(-0.631276663091966,0.494621958044076,
-1.69433797050196));
#66552=CARTESIAN_POINT('Ctrl Pts',(-0.694211919447908,0.379493864559592,
-1.68905726602588));
#66553=CARTESIAN_POINT('Ctrl Pts',(-0.757147175803852,0.264365771075104,
-1.68377656154981));
#66554=CARTESIAN_POINT('Ctrl Pts',(-0.790826718319016,0.133244918614775,
-1.67849585707373));
#66555=CARTESIAN_POINT('Ctrl Pts',(-0.791164728860946,0.0020381727865403,
-1.67321515259765));
#66556=CARTESIAN_POINT('Ctrl Pts',(-0.791166478467409,0.00135902186643757,
-1.673187818673));
#66557=CARTESIAN_POINT('Ctrl Pts',(-0.79116733475644,0.000679868644999612,
-1.67316048474835));
#66558=CARTESIAN_POINT('Ctrl Pts',(-0.791167298283308,7.15331164842455E-7,
-1.6731331508237));
#66559=CARTESIAN_POINT('Origin',(0.,0.,-1.425));
#66560=CARTESIAN_POINT('',(-0.791042737690139,-1.10214458017843E-5,-1.4446668491763));
#66561=CARTESIAN_POINT('',(-0.791050601996816,-1.425480118063E-5,-1.4731331508237));
#66562=CARTESIAN_POINT('',(-0.7911,-9.68818082805471E-17,-1.425));
#66563=CARTESIAN_POINT('Ctrl Pts',(-0.791042737690139,-1.10214458017843E-5,
-1.4446668491763));
#66564=CARTESIAN_POINT('Ctrl Pts',(-0.791004053579004,0.0782010396373887,
-1.4478132266791));
#66565=CARTESIAN_POINT('Ctrl Pts',(-0.779479835816688,0.156424253179001,
-1.4509596041819));
#66566=CARTESIAN_POINT('Ctrl Pts',(-0.756635697237545,0.231188685144309,
-1.45410598168471));
#66567=CARTESIAN_POINT('Ctrl Pts',(-0.718295369435313,0.356669136927015,
-1.45938668616078));
#66568=CARTESIAN_POINT('Ctrl Pts',(-0.648068643805594,0.472406756836154,
-1.46466739063686));
#66569=CARTESIAN_POINT('Ctrl Pts',(-0.554475043107099,0.56436088901011,
-1.46994809511294));
#66570=CARTESIAN_POINT('Ctrl Pts',(-0.460881442408603,0.656315021184065,
-1.47522879958902));
#66571=CARTESIAN_POINT('Ctrl Pts',(-0.343920966641331,0.724485665622839,
-1.4805095040651));
#66572=CARTESIAN_POINT('Ctrl Pts',(-0.217782621860084,0.76060273210701,
-1.48579020854118));
#66573=CARTESIAN_POINT('Ctrl Pts',(-0.0916442770788372,0.796719798591182,
-1.49107091301725));
#66574=CARTESIAN_POINT('Ctrl Pts',(0.0436719367163846,0.800783287120751,
-1.49635161749333));
#66575=CARTESIAN_POINT('Ctrl Pts',(0.171750195596534,0.77230023746303,-1.50163232196941));
#66576=CARTESIAN_POINT('Ctrl Pts',(0.299828454476682,0.74381718780531,-1.50691302644549));
#66577=CARTESIAN_POINT('Ctrl Pts',(0.420668758441757,0.682787599960299,
-1.51219373092157));
#66578=CARTESIAN_POINT('Ctrl Pts',(0.519611421872524,0.596615250167572,
-1.51747443539765));
#66579=CARTESIAN_POINT('Ctrl Pts',(0.618554085303293,0.510442900374843,
-1.52275513987373));
#66580=CARTESIAN_POINT('Ctrl Pts',(0.69559910819975,0.399127788634402,-1.5280358443498));
#66581=CARTESIAN_POINT('Ctrl Pts',(0.741399809221914,0.276174056273594,
-1.53331654882588));
#66582=CARTESIAN_POINT('Ctrl Pts',(0.787200510244078,0.153220323912786,
-1.53859725330196));
#66583=CARTESIAN_POINT('Ctrl Pts',(0.801756889391944,0.0186279709316112,
-1.54387795777804));
#66584=CARTESIAN_POINT('Ctrl Pts',(0.783303046257617,-0.111274993580937,
-1.54915866225412));
#66585=CARTESIAN_POINT('Ctrl Pts',(0.764849203123291,-0.241177958093484,
-1.5544393667302));
#66586=CARTESIAN_POINT('Ctrl Pts',(0.713385137706772,-0.36639153413741,
-1.55972007120627));
#66587=CARTESIAN_POINT('Ctrl Pts',(0.635154189315716,-0.4717254946127,-1.56500077568235));
#66588=CARTESIAN_POINT('Ctrl Pts',(0.556923240924658,-0.577059455087992,
-1.57028148015843));
#66589=CARTESIAN_POINT('Ctrl Pts',(0.451925409559061,-0.662513799994649,
-1.57556218463451));
#66590=CARTESIAN_POINT('Ctrl Pts',(0.332898458597657,-0.717721674980074,
-1.58084288911059));
#66591=CARTESIAN_POINT('Ctrl Pts',(0.213871507636254,-0.7729295499655,-1.58612359358667));
#66592=CARTESIAN_POINT('Ctrl Pts',(0.0808154370790435,-0.797890955029695,
-1.59140429806274));
#66593=CARTESIAN_POINT('Ctrl Pts',(-0.0501281173771344,-0.789577708855262,
-1.59668500253882));
#66594=CARTESIAN_POINT('Ctrl Pts',(-0.181071671833312,-0.781264462680829,
-1.6019657070149));
#66595=CARTESIAN_POINT('Ctrl Pts',(-0.309902710188458,-0.739676565267769,
-1.60724641149098));
#66596=CARTESIAN_POINT('Ctrl Pts',(-0.420992154574379,-0.669859233167479,
-1.61252711596706));
#66597=CARTESIAN_POINT('Ctrl Pts',(-0.532081598960299,-0.600041901067189,
-1.61780782044314));
#66598=CARTESIAN_POINT('Ctrl Pts',(-0.625429449376996,-0.501995134279669,
-1.62308852491922));
#66599=CARTESIAN_POINT('Ctrl Pts',(-0.689711254499554,-0.387613430997369,
-1.62836922939529));
#66600=CARTESIAN_POINT('Ctrl Pts',(-0.753993059622111,-0.273231727715071,
-1.63364993387137));
#66601=CARTESIAN_POINT('Ctrl Pts',(-0.789208819450532,-0.142515087937991,
-1.63893063834745));
#66602=CARTESIAN_POINT('Ctrl Pts',(-0.79108635035909,-0.0113213403992397,
-1.64421134282353));
#66603=CARTESIAN_POINT('Ctrl Pts',(-0.791140334776021,-0.00754914259760037,
-1.64436317827445));
#66604=CARTESIAN_POINT('Ctrl Pts',(-0.791166757546086,-0.00377655035762189,
-1.64451501372537));
#66605=CARTESIAN_POINT('Ctrl Pts',(-0.791165709393907,-3.94338443360232E-6,
-1.6446668491763));
#66606=CARTESIAN_POINT('Ctrl Pts',(-0.791167298283308,7.15331164842455E-7,
-1.6731331508237));
#66607=CARTESIAN_POINT('Ctrl Pts',(-0.791160288427158,-0.130527339633897,
-1.66787978027227));
#66608=CARTESIAN_POINT('Ctrl Pts',(-0.75817652789474,-0.261058807542124,
-1.66262640972084));
#66609=CARTESIAN_POINT('Ctrl Pts',(-0.696157971514176,-0.375912038965486,
-1.65737303916941));
#66610=CARTESIAN_POINT('Ctrl Pts',(-0.633816725056783,-0.491362865693143,
-1.65209233469333));
#66611=CARTESIAN_POINT('Ctrl Pts',(-0.542137753573301,-0.590971879952318,
-1.64681163021726));
#66612=CARTESIAN_POINT('Ctrl Pts',(-0.432243049112271,-0.662655060220662,
-1.64153092574118));
#66613=CARTESIAN_POINT('Ctrl Pts',(-0.322348344651241,-0.734338240489005,
-1.6362502212651));
#66614=CARTESIAN_POINT('Ctrl Pts',(-0.194237907212663,-0.778095586766515,
-1.63096951678902));
#66615=CARTESIAN_POINT('Ctrl Pts',(-0.063453395297621,-0.788618696815594,
-1.62568881231294));
#66616=CARTESIAN_POINT('Ctrl Pts',(0.0673311166174213,-0.799141806864672,
-1.62040810783686));
#66617=CARTESIAN_POINT('Ctrl Pts',(0.200789703008928,-0.776430680685319,
-1.61512740336078));
#66618=CARTESIAN_POINT('Ctrl Pts',(0.320731897157678,-0.723240508052168,
-1.60984669888471));
#66619=CARTESIAN_POINT('Ctrl Pts',(0.440674091306426,-0.670050335419017,
-1.60456599440863));
#66620=CARTESIAN_POINT('Ctrl Pts',(0.547099893212418,-0.586381116332069,
-1.59928528993255));
#66621=CARTESIAN_POINT('Ctrl Pts',(0.627098305910867,-0.482383143430243,
-1.59400458545647));
#66622=CARTESIAN_POINT('Ctrl Pts',(0.707096718609317,-0.378385170528417,
-1.58872388098039));
#66623=CARTESIAN_POINT('Ctrl Pts',(0.760667742100224,-0.254058443811713,
-1.58344317650431));
#66624=CARTESIAN_POINT('Ctrl Pts',(0.781312432431045,-0.124485602663945,
-1.57816247202824));
#66625=CARTESIAN_POINT('Ctrl Pts',(0.801957122761867,0.0050872384838257,
-1.57288176755216));
#66626=CARTESIAN_POINT('Ctrl Pts',(0.789675479932601,0.139906194062661,
-1.56760106307608));
#66627=CARTESIAN_POINT('Ctrl Pts',(0.745957445766109,0.263615764794187,
-1.5623203586));
#66628=CARTESIAN_POINT('Ctrl Pts',(0.702239411599617,0.387325335525712,
-1.55703965412392));
#66629=CARTESIAN_POINT('Ctrl Pts',(0.627084986095899,0.499925521409928,
-1.55175894964784));
#66630=CARTESIAN_POINT('Ctrl Pts',(0.529611493646138,0.587756282943728,
-1.54647824517177));
#66631=CARTESIAN_POINT('Ctrl Pts',(0.432138001196376,0.67558704447753,-1.54119754069569));
#66632=CARTESIAN_POINT('Ctrl Pts',(0.312345441800571,0.738648381660915,
-1.53591683621961));
#66633=CARTESIAN_POINT('Ctrl Pts',(0.184766394429838,0.769290037522467,
-1.53063613174353));
#66634=CARTESIAN_POINT('Ctrl Pts',(0.057187347059108,0.799931693384018,
-1.52535542726745));
#66635=CARTESIAN_POINT('Ctrl Pts',(-0.078178188286549,0.798153667923737,
-1.52007472279137));
#66636=CARTESIAN_POINT('Ctrl Pts',(-0.204908404256992,0.764171661478476,
-1.51479401831529));
#66637=CARTESIAN_POINT('Ctrl Pts',(-0.331638620227433,0.730189655033216,
-1.50951331383922));
#66638=CARTESIAN_POINT('Ctrl Pts',(-0.449733516822661,0.664003667602976,
-1.50423260936314));
#66639=CARTESIAN_POINT('Ctrl Pts',(-0.544866466249495,0.573643021659559,
-1.49895190488706));
#66640=CARTESIAN_POINT('Ctrl Pts',(-0.639999415676332,0.48328237571614,
-1.49367120041098));
#66641=CARTESIAN_POINT('Ctrl Pts',(-0.712170417934775,0.368747071259543,
-1.4883904959349));
#66642=CARTESIAN_POINT('Ctrl Pts',(-0.752624081245608,0.243931905808006,
-1.48310979145882));
#66643=CARTESIAN_POINT('Ctrl Pts',(-0.77809995370761,0.165329006190866,
-1.47978424458045));
#66644=CARTESIAN_POINT('Ctrl Pts',(-0.790997027553039,0.0826492102907407,
-1.47645869770208));
#66645=CARTESIAN_POINT('Ctrl Pts',(-0.791050601996816,-1.425480118063E-5,
-1.4731331508237));
#66646=CARTESIAN_POINT('Origin',(0.,0.,-1.425));
#66647=CARTESIAN_POINT('',(-0.791104263028763,2.01628765369166E-5,-1.2446668491763));
#66648=CARTESIAN_POINT('',(-0.791090383657342,2.02495652405869E-5,-1.2731331508237));
#66649=CARTESIAN_POINT('',(-0.7911,-9.68818082805471E-17,-1.425));
#66650=CARTESIAN_POINT('Ctrl Pts',(-0.791104263028763,2.01628765369166E-5,
-1.2446668491763));
#66651=CARTESIAN_POINT('Ctrl Pts',(-0.791133904479299,0.0289453631637145,
-1.24583073515675));
#66652=CARTESIAN_POINT('Ctrl Pts',(-0.789578009246314,0.0578673918392402,
-1.2469946211372));
#66653=CARTESIAN_POINT('Ctrl Pts',(-0.786412187639368,0.0866121100375816,
-1.24815850711765));
#66654=CARTESIAN_POINT('Ctrl Pts',(-0.77204843671267,0.217030694506554,
-1.25343921159373));
#66655=CARTESIAN_POINT('Ctrl Pts',(-0.724543437014594,0.343799242098573,
-1.2587199160698));
#66656=CARTESIAN_POINT('Ctrl Pts',(-0.649660235625171,0.451538885059025,
-1.26400062054588));
#66657=CARTESIAN_POINT('Ctrl Pts',(-0.574777034235747,0.559278528019478,
-1.26928132502196));
#66658=CARTESIAN_POINT('Ctrl Pts',(-0.472515631154975,0.647989266348364,
-1.27456202949804));
#66659=CARTESIAN_POINT('Ctrl Pts',(-0.355281821229079,0.706909197830279,
-1.27984273397412));
#66660=CARTESIAN_POINT('Ctrl Pts',(-0.238048011303183,0.765829129312195,
-1.2851234384502));
#66661=CARTESIAN_POINT('Ctrl Pts',(-0.105841794532163,0.794958253947141,
-1.29040414292628));
#66662=CARTESIAN_POINT('Ctrl Pts',(0.0252982930063838,0.790762785444449,
-1.29568484740235));
#66663=CARTESIAN_POINT('Ctrl Pts',(0.15643838054493,0.786567316941757,-1.30096555187843));
#66664=CARTESIAN_POINT('Ctrl Pts',(0.286512338850998,0.74904725530143,-1.30624625635451));
#66665=CARTESIAN_POINT('Ctrl Pts',(0.399740305797077,0.682754329458378,
-1.31152696083059));
#66666=CARTESIAN_POINT('Ctrl Pts',(0.512968272743153,0.616461403615328,
-1.31680766530667));
#66667=CARTESIAN_POINT('Ctrl Pts',(0.609350248329239,0.521395613569551,
-1.32208836978275));
#66668=CARTESIAN_POINT('Ctrl Pts',(0.677193697737961,0.409089821697983,
-1.32736907425882));
#66669=CARTESIAN_POINT('Ctrl Pts',(0.745037147146684,0.296784029826413,
-1.3326497787349));
#66670=CARTESIAN_POINT('Ctrl Pts',(0.784342070378046,0.167238236129048,
-1.33793048321098));
#66671=CARTESIAN_POINT('Ctrl Pts',(0.790340208838238,0.0361682286880373,
-1.34321118768706));
#66672=CARTESIAN_POINT('Ctrl Pts',(0.796338347298431,-0.0949017787529772,
-1.34849189216314));
#66673=CARTESIAN_POINT('Ctrl Pts',(0.769029700987452,-0.227495999937637,
-1.35377259663922));
#66674=CARTESIAN_POINT('Ctrl Pts',(0.711727205709581,-0.345528828212252,
-1.35905330111529));
#66675=CARTESIAN_POINT('Ctrl Pts',(0.65442471043171,-0.463561656486866,
-1.36433400559137));
#66676=CARTESIAN_POINT('Ctrl Pts',(0.567128366186948,-0.567033091851435,
-1.36961471006745));
#66677=CARTESIAN_POINT('Ctrl Pts',(0.460428488626161,-0.643390544952542,
-1.37489541454353));
#66678=CARTESIAN_POINT('Ctrl Pts',(0.353728611065377,-0.719747998053647,
-1.38017611901961));
#66679=CARTESIAN_POINT('Ctrl Pts',(0.227625200188569,-0.768991468891293,
-1.38545682349569));
#66680=CARTESIAN_POINT('Ctrl Pts',(0.0974164329971917,-0.785147008562731,
-1.39073752797176));
#66681=CARTESIAN_POINT('Ctrl Pts',(-0.0327923341941915,-0.801302548234169,
-1.39601823244784));
#66682=CARTESIAN_POINT('Ctrl Pts',(-0.167106457700145,-0.784370156739396,
-1.40129893692392));
#66683=CARTESIAN_POINT('Ctrl Pts',(-0.289231681711864,-0.736403979325904,
-1.4065796414));
#66684=CARTESIAN_POINT('Ctrl Pts',(-0.411356905723584,-0.688437801912412,
-1.41186034587608));
#66685=CARTESIAN_POINT('Ctrl Pts',(-0.52129323024107,-0.609437838580201,
-1.41714105035216));
#66686=CARTESIAN_POINT('Ctrl Pts',(-0.605703780871598,-0.508987933364585,
-1.42242175482824));
#66687=CARTESIAN_POINT('Ctrl Pts',(-0.690114331502122,-0.408538028148975,
-1.42770245930431));
#66688=CARTESIAN_POINT('Ctrl Pts',(-0.748999108245692,-0.286638181049963,
-1.43298316378039));
#66689=CARTESIAN_POINT('Ctrl Pts',(-0.775214531630106,-0.158076615672323,
-1.43826386825647));
#66690=CARTESIAN_POINT('Ctrl Pts',(-0.785810141647417,-0.106115287793623,
-1.44039819522975));
#66691=CARTESIAN_POINT('Ctrl Pts',(-0.791068978833091,-0.0530657205264479,
-1.44253252220302));
#66692=CARTESIAN_POINT('Ctrl Pts',(-0.791042737690139,-1.10214458017843E-5,
-1.4446668491763));
#66693=CARTESIAN_POINT('Ctrl Pts',(-0.791050601996816,-1.425480118063E-5,
-1.4731331508237));
#66694=CARTESIAN_POINT('Ctrl Pts',(-0.791082099517261,-0.0486138108255385,
-1.471177993226));
#66695=CARTESIAN_POINT('Ctrl Pts',(-0.786674232982901,-0.0972077220952497,
-1.46922283562829));
#66696=CARTESIAN_POINT('Ctrl Pts',(-0.777773211183365,-0.144964182843345,
-1.46726767803059));
#66697=CARTESIAN_POINT('Ctrl Pts',(-0.753732353447066,-0.273950079596685,
-1.46198697355451));
#66698=CARTESIAN_POINT('Ctrl Pts',(-0.696914313611244,-0.396826846656892,
-1.45670626907843));
#66699=CARTESIAN_POINT('Ctrl Pts',(-0.61421194591545,-0.498687745825661,
-1.45142556460235));
#66700=CARTESIAN_POINT('Ctrl Pts',(-0.531509578219655,-0.600548644994431,
-1.44614486012628));
#66701=CARTESIAN_POINT('Ctrl Pts',(-0.422922882663888,-0.681393676271764,
-1.4408641556502));
#66702=CARTESIAN_POINT('Ctrl Pts',(-0.301625004027223,-0.731415162057432,
-1.43558345117412));
#66703=CARTESIAN_POINT('Ctrl Pts',(-0.180327125390558,-0.7814366478431,
-1.43030274669804));
#66704=CARTESIAN_POINT('Ctrl Pts',(-0.046318063672995,-0.800634588137102,
-1.42502204222196));
#66705=CARTESIAN_POINT('Ctrl Pts',(0.0841449337465121,-0.786679993686579,
-1.41974133774588));
#66706=CARTESIAN_POINT('Ctrl Pts',(0.214607931166019,-0.772725399236057,
-1.4144606332698));
#66707=CARTESIAN_POINT('Ctrl Pts',(0.34152486428747,-0.72561827004101,-1.40917992879373));
#66708=CARTESIAN_POINT('Ctrl Pts',(0.449498864034337,-0.6510733857053,-1.40389922431765));
#66709=CARTESIAN_POINT('Ctrl Pts',(0.557472863781204,-0.57652850136959,
-1.39861851984157));
#66710=CARTESIAN_POINT('Ctrl Pts',(0.646503930153488,-0.474545861893217,
-1.39333781536549));
#66711=CARTESIAN_POINT('Ctrl Pts',(0.705791300487265,-0.357497444044592,
-1.38805711088941));
#66712=CARTESIAN_POINT('Ctrl Pts',(0.765078670821043,-0.240449026195966,
-1.38277640641333));
#66713=CARTESIAN_POINT('Ctrl Pts',(0.794622345116314,-0.108334829975088,
-1.37749570193726));
#66714=CARTESIAN_POINT('Ctrl Pts',(0.790838246181988,0.0228177719709503,
-1.37221499746118));
#66715=CARTESIAN_POINT('Ctrl Pts',(0.787054147247662,0.153970373916989,
-1.3669342929851));
#66716=CARTESIAN_POINT('Ctrl Pts',(0.749942275083739,0.284161381588188,
-1.36165358850902));
#66717=CARTESIAN_POINT('Ctrl Pts',(0.684004839307479,0.397596733067401,
-1.35637288403294));
#66718=CARTESIAN_POINT('Ctrl Pts',(0.618067403531222,0.511032084546611,
-1.35109217955686));
#66719=CARTESIAN_POINT('Ctrl Pts',(0.523304404142631,0.607711779833835,
-1.34581147508079));
#66720=CARTESIAN_POINT('Ctrl Pts',(0.411211970610016,0.675907166383779,
-1.34053077060471));
#66721=CARTESIAN_POINT('Ctrl Pts',(0.299119537077399,0.744102552933724,
-1.33525006612863));
#66722=CARTESIAN_POINT('Ctrl Pts',(0.169697669400756,0.783813630746388,
-1.32996936165255));
#66723=CARTESIAN_POINT('Ctrl Pts',(0.0386471216343184,0.790222868772667,
-1.32468865717647));
#66724=CARTESIAN_POINT('Ctrl Pts',(-0.0924034261321194,0.796632106798947,
-1.31940795270039));
#66725=CARTESIAN_POINT('Ctrl Pts',(-0.225082653988353,0.769739505038843,
-1.31412724822431));
#66726=CARTESIAN_POINT('Ctrl Pts',(-0.343294642735622,0.712807527044253,
-1.30884654374824));
#66727=CARTESIAN_POINT('Ctrl Pts',(-0.461506631482891,0.655875549049664,
-1.30356583927216));
#66728=CARTESIAN_POINT('Ctrl Pts',(-0.565251381121196,0.56890419482059,
-1.29828513479608));
#66729=CARTESIAN_POINT('Ctrl Pts',(-0.641943145302336,0.462444353994365,
-1.29300443032));
#66730=CARTESIAN_POINT('Ctrl Pts',(-0.718634909483477,0.35598451316814,
-1.28772372584392));
#66731=CARTESIAN_POINT('Ctrl Pts',(-0.768273688207453,0.230036185744764,
-1.28244302136784));
#66732=CARTESIAN_POINT('Ctrl Pts',(-0.784837575978011,0.0998787348482238,
-1.27716231689177));
#66733=CARTESIAN_POINT('Ctrl Pts',(-0.789050312798929,0.0667754505526489,
-1.27581926153574));
#66734=CARTESIAN_POINT('Ctrl Pts',(-0.791123597755304,0.0333998987815609,
-1.27447620617972));
#66735=CARTESIAN_POINT('Ctrl Pts',(-0.791090383657342,2.02495652405869E-5,
-1.2731331508237));
#66736=CARTESIAN_POINT('Origin',(0.,0.,-1.425));
#66737=CARTESIAN_POINT('',(-0.791130810276663,-1.74211169955418E-5,-1.0446668491763));
#66738=CARTESIAN_POINT('',(-0.791143275750807,-1.47194715005396E-5,-1.0731331508237));
#66739=CARTESIAN_POINT('',(-0.7911,-9.68818082805471E-17,-1.425));
#66740=CARTESIAN_POINT('Ctrl Pts',(-0.791130810276663,-1.74211169955418E-5,
-1.0446668491763));
#66741=CARTESIAN_POINT('Ctrl Pts',(-0.791024239474405,0.110865102978929,
-1.04912894811047));
#66742=CARTESIAN_POINT('Ctrl Pts',(-0.767493315443536,0.22179143015014,
-1.05359104704465));
#66743=CARTESIAN_POINT('Ctrl Pts',(-0.722230908301505,0.322998918832374,
-1.05805314597882));
#66744=CARTESIAN_POINT('Ctrl Pts',(-0.668664772830517,0.442773680974816,
-1.0633338504549));
#66745=CARTESIAN_POINT('Ctrl Pts',(-0.584662137800377,0.54893651327924,
-1.06861455493098));
#66746=CARTESIAN_POINT('Ctrl Pts',(-0.480413744051037,0.62860832081652,
-1.07389525940706));
#66747=CARTESIAN_POINT('Ctrl Pts',(-0.376165350301698,0.708280128353801,
-1.07917596388314));
#66748=CARTESIAN_POINT('Ctrl Pts',(-0.25167119783316,0.761460911123938,
-1.08445666835922));
#66749=CARTESIAN_POINT('Ctrl Pts',(-0.12203423720693,0.781699067047047,
-1.08973737283529));
#66750=CARTESIAN_POINT('Ctrl Pts',(0.00760272341930042,0.801937222970155,
-1.09501807731137));
#66751=CARTESIAN_POINT('Ctrl Pts',(0.142382492203222,0.789232752046236,
-1.10029878178745));
#66752=CARTESIAN_POINT('Ctrl Pts',(0.265954323794372,0.745126891293006,
-1.10557948626353));
#66753=CARTESIAN_POINT('Ctrl Pts',(0.389526155385522,0.701021030539776,
-1.11086019073961));
#66754=CARTESIAN_POINT('Ctrl Pts',(0.5018900497839,0.625513779957236,-1.11614089521569));
#66755=CARTESIAN_POINT('Ctrl Pts',(0.589414633078783,0.527765266747921,
-1.12142159969176));
#66756=CARTESIAN_POINT('Ctrl Pts',(0.676939216373666,0.430016753538605,
-1.12670230416784));
#66757=CARTESIAN_POINT('Ctrl Pts',(0.739624488565055,0.310026977702514,
-1.13198300864392));
#66758=CARTESIAN_POINT('Ctrl Pts',(0.769865814832208,0.182352443432055,
-1.13726371312));
#66759=CARTESIAN_POINT('Ctrl Pts',(0.80010714109936,0.0546779091615972,
-1.14254441759608));
#66760=CARTESIAN_POINT('Ctrl Pts',(0.797904521442275,-0.0806813835432276,
-1.14782512207216));
#66761=CARTESIAN_POINT('Ctrl Pts',(0.76352516564653,-0.207304384655365,
-1.15310582654824));
#66762=CARTESIAN_POINT('Ctrl Pts',(0.729145809850785,-0.333927385767502,
-1.15838653102431));
#66763=CARTESIAN_POINT('Ctrl Pts',(0.66258971791638,-0.451814095286952,
-1.16366723550039));
#66764=CARTESIAN_POINT('Ctrl Pts',(0.571931111371964,-0.546663141539403,
-1.16894793997647));
#66765=CARTESIAN_POINT('Ctrl Pts',(0.481272504827549,-0.641512187791854,
-1.17422864445255));
#66766=CARTESIAN_POINT('Ctrl Pts',(0.366511383673123,-0.713323570777307,
-1.17950934892863));
#66767=CARTESIAN_POINT('Ctrl Pts',(0.241569940275243,-0.753385525762419,
-1.18479005340471));
#66768=CARTESIAN_POINT('Ctrl Pts',(0.116628496877367,-0.793447480747529,
-1.19007075788078));
#66769=CARTESIAN_POINT('Ctrl Pts',(-0.0184932687639632,-0.8017600077323,
-1.19535146235686));
#66770=CARTESIAN_POINT('Ctrl Pts',(-0.147403122107609,-0.777314676347893,
-1.20063216683294));
#66771=CARTESIAN_POINT('Ctrl Pts',(-0.276312975451259,-0.752869344963485,
-1.20591287130902));
#66772=CARTESIAN_POINT('Ctrl Pts',(-0.399010916497224,-0.695666155209897,
-1.2111935757851));
#66773=CARTESIAN_POINT('Ctrl Pts',(-0.50061190124246,-0.612644685610925,
-1.21647428026118));
#66774=CARTESIAN_POINT('Ctrl Pts',(-0.602212885987697,-0.529623216011954,
-1.22175498473726));
#66775=CARTESIAN_POINT('Ctrl Pts',(-0.682716914432204,-0.420783466567598,
-1.22703568921333));
#66776=CARTESIAN_POINT('Ctrl Pts',(-0.732357677576797,-0.299329281172457,
-1.23231639368941));
#66777=CARTESIAN_POINT('Ctrl Pts',(-0.771057440605863,-0.204644028651473,
-1.23643321218504));
#66778=CARTESIAN_POINT('Ctrl Pts',(-0.790999417301728,-0.102292092389177,
-1.24055003068067));
#66779=CARTESIAN_POINT('Ctrl Pts',(-0.791104263028763,2.01628765369166E-5,
-1.2446668491763));
#66780=CARTESIAN_POINT('Ctrl Pts',(-0.791090383657342,2.02495652405869E-5,
-1.2731331508237));
#66781=CARTESIAN_POINT('Ctrl Pts',(-0.790993004600682,-0.0978441800543782,
-1.26919550170365));
#66782=CARTESIAN_POINT('Ctrl Pts',(-0.772788585159708,-0.195743830485581,
-1.26525785258359));
#66783=CARTESIAN_POINT('Ctrl Pts',(-0.737307591148638,-0.286920369399794,
-1.26132020346353));
#66784=CARTESIAN_POINT('Ctrl Pts',(-0.689724721731569,-0.409195448381568,
-1.25603949898745));
#66785=CARTESIAN_POINT('Ctrl Pts',(-0.611069986080291,-0.519379031975411,
-1.25075879451137));
#66786=CARTESIAN_POINT('Ctrl Pts',(-0.510885347093584,-0.604104249668043,
-1.24547809003529));
#66787=CARTESIAN_POINT('Ctrl Pts',(-0.410700708106876,-0.688829467360676,
-1.24019738555922));
#66788=CARTESIAN_POINT('Ctrl Pts',(-0.288986165784739,-0.748096319152098,
-1.23491668108314));
#66789=CARTESIAN_POINT('Ctrl Pts',(-0.160507463568594,-0.774714874312284,
-1.22963597660706));
#66790=CARTESIAN_POINT('Ctrl Pts',(-0.0320287613524518,-0.801333429472469,
-1.22435527213098));
#66791=CARTESIAN_POINT('Ctrl Pts',(0.103214100757698,-0.79530368800142,
-1.2190745676549));
#66792=CARTESIAN_POINT('Ctrl Pts',(0.228814197458578,-0.757357145198557,
-1.21379386317882));
#66793=CARTESIAN_POINT('Ctrl Pts',(0.354414294159461,-0.719410602395693,
-1.20851315870275));
#66794=CARTESIAN_POINT('Ctrl Pts',(0.470371625451073,-0.649547258261012,
-1.20323245422667));
#66795=CARTESIAN_POINT('Ctrl Pts',(0.562618881286993,-0.556242552095121,
-1.19795174975059));
#66796=CARTESIAN_POINT('Ctrl Pts',(0.654866137122914,-0.462937845929231,
-1.19267104527451));
#66797=CARTESIAN_POINT('Ctrl Pts',(0.723403317503141,-0.34619177773213,
-1.18739034079843));
#66798=CARTESIAN_POINT('Ctrl Pts',(0.759915866069944,-0.220167342803353,
-1.18210963632235));
#66799=CARTESIAN_POINT('Ctrl Pts',(0.796428414636747,-0.0941429078745748,
-1.17682893184628));
#66800=CARTESIAN_POINT('Ctrl Pts',(0.800916331390125,0.0411598937858802,
-1.1715482273702));
#66801=CARTESIAN_POINT('Ctrl Pts',(0.772835166783604,0.169326865335895,
-1.16626752289412));
#66802=CARTESIAN_POINT('Ctrl Pts',(0.744754002177082,0.29749383688591,-1.16098681841804));
#66803=CARTESIAN_POINT('Ctrl Pts',(0.684103756210661,0.418524978325484,
-1.15570611394196));
#66804=CARTESIAN_POINT('Ctrl Pts',(0.598242185439255,0.517737452675375,
-1.15042540946588));
#66805=CARTESIAN_POINT('Ctrl Pts',(0.512380614667846,0.616949927025268,
-1.1451447049898));
#66806=CARTESIAN_POINT('Ctrl Pts',(0.401307719091452,0.694343734285476,
-1.13986400051373));
#66807=CARTESIAN_POINT('Ctrl Pts',(0.278498255695447,0.740529880502141,
-1.13458329603765));
#66808=CARTESIAN_POINT('Ctrl Pts',(0.155688792299449,0.786716026718803,
-1.12930259156157));
#66809=CARTESIAN_POINT('Ctrl Pts',(0.0211427610838415,0.801694511891926,
-1.12402188708549));
#66810=CARTESIAN_POINT('Ctrl Pts',(-0.108817448365971,0.783648228016271,
-1.11874118260941));
#66811=CARTESIAN_POINT('Ctrl Pts',(-0.238777657815787,0.765601944140615,
-1.11346047813333));
#66812=CARTESIAN_POINT('Ctrl Pts',(-0.364152045499809,0.714530891216179,
-1.10817977365726));
#66813=CARTESIAN_POINT('Ctrl Pts',(-0.469730875528235,0.636630730421804,
-1.10289906918118));
#66814=CARTESIAN_POINT('Ctrl Pts',(-0.575309705556658,0.55873056962743,
-1.0976183647051));
#66815=CARTESIAN_POINT('Ctrl Pts',(-0.661092977929487,0.454001300963119,
-1.09233766022902));
#66816=CARTESIAN_POINT('Ctrl Pts',(-0.716673934610609,0.335148107247632,
-1.08705695575294));
#66817=CARTESIAN_POINT('Ctrl Pts',(-0.765524638913044,0.230686749108265,
-1.0824156874432));
#66818=CARTESIAN_POINT('Ctrl Pts',(-0.791044530563423,0.115314881568087,
-1.07777441913345));
#66819=CARTESIAN_POINT('Ctrl Pts',(-0.791143275750807,-1.47194715005396E-5,
-1.0731331508237));
#66820=CARTESIAN_POINT('Origin',(0.,0.,-1.425));
#66821=CARTESIAN_POINT('',(-0.791033958661136,3.6737787218466E-6,-0.844666849176296));
#66822=CARTESIAN_POINT('',(-0.791032964947078,-4.2330507261862E-7,-0.873133150823704));
#66823=CARTESIAN_POINT('',(-0.7911,-9.68818082805471E-17,-1.425));
#66824=CARTESIAN_POINT('Ctrl Pts',(-0.791033958661136,3.6737787218466E-6,
-0.844666849176296));
#66825=CARTESIAN_POINT('Ctrl Pts',(-0.791043981016399,0.0616432469844158,
-0.847146456588119));
#66826=CARTESIAN_POINT('Ctrl Pts',(-0.783928212048688,0.123280544004755,
-0.849626063999942));
#66827=CARTESIAN_POINT('Ctrl Pts',(-0.769660893106755,0.183215436290213,
-0.852105671411765));
#66828=CARTESIAN_POINT('Ctrl Pts',(-0.739276448117974,0.310855986345038,
-0.857386375887843));
#66829=CARTESIAN_POINT('Ctrl Pts',(-0.676456693085718,0.430775409428172,
-0.862667080363922));
#66830=CARTESIAN_POINT('Ctrl Pts',(-0.588822577554407,0.528425736158908,
-0.867947784840001));
#66831=CARTESIAN_POINT('Ctrl Pts',(-0.501188462023096,0.626076062889645,
-0.873228489316079));
#66832=CARTESIAN_POINT('Ctrl Pts',(-0.38873998599273,0.701457293267984,
-0.878509193792157));
#66833=CARTESIAN_POINT('Ctrl Pts',(-0.265118784355619,0.745424588174215,
-0.883789898268235));
#66834=CARTESIAN_POINT('Ctrl Pts',(-0.141497582718508,0.789391883080447,
-0.889070602744314));
#66835=CARTESIAN_POINT('Ctrl Pts',(-0.00670365547465232,0.80194524251457,
-0.894351307220393));
#66836=CARTESIAN_POINT('Ctrl Pts',(0.122910534398462,0.781561761479401,
-0.899632011696472));
#66837=CARTESIAN_POINT('Ctrl Pts',(0.252524724271576,0.761178280444233,
-0.90491271617255));
#66838=CARTESIAN_POINT('Ctrl Pts',(0.376959176773948,0.707857958939773,
-0.910193420648627));
#66839=CARTESIAN_POINT('Ctrl Pts',(0.481118183817872,0.628069327122963,
-0.915474125124706));
#66840=CARTESIAN_POINT('Ctrl Pts',(0.585277190861797,0.548280695306153,
-0.920754829600784));
#66841=CARTESIAN_POINT('Ctrl Pts',(0.669160752447273,0.442023753176993,
-0.926035534076864));
#66842=CARTESIAN_POINT('Ctrl Pts',(0.722592573074247,0.322189012554494,
-0.931316238552942));
#66843=CARTESIAN_POINT('Ctrl Pts',(0.776024393701218,0.202354271932001,
-0.936596943029021));
#66844=CARTESIAN_POINT('Ctrl Pts',(0.79900447336969,0.0689417328161721,
-0.941877647505098));
#66845=CARTESIAN_POINT('Ctrl Pts',(0.788744994336818,-0.0618637242777383,
-0.947158351981176));
#66846=CARTESIAN_POINT('Ctrl Pts',(0.778485515303946,-0.19266918137166,
-0.952439056457254));
#66847=CARTESIAN_POINT('Ctrl Pts',(0.734986477569723,-0.320867556443662,
-0.957719760933334));
#66848=CARTESIAN_POINT('Ctrl Pts',(0.663524946790219,-0.430906522879311,
-0.963000465409413));
#66849=CARTESIAN_POINT('Ctrl Pts',(0.592063416010716,-0.540945489314955,
-0.968281169885491));
#66850=CARTESIAN_POINT('Ctrl Pts',(0.492639392185934,-0.632825047114247,
-0.973561874361569));
#66851=CARTESIAN_POINT('Ctrl Pts',(0.377314454809184,-0.695398870192459,
-0.978842578837647));
#66852=CARTESIAN_POINT('Ctrl Pts',(0.261989517432433,-0.757972693270672,
-0.984123283313726));
#66853=CARTESIAN_POINT('Ctrl Pts',(0.130763666503716,-0.791240781627805,
-0.989403987789805));
#66854=CARTESIAN_POINT('Ctrl Pts',(-0.000443494528374638,-0.791167232502398,
-0.994684692265883));
#66855=CARTESIAN_POINT('Ctrl Pts',(-0.131650655560465,-0.791093683376991,
-0.999965396741962));
#66856=CARTESIAN_POINT('Ctrl Pts',(-0.262839126695928,-0.757678496769043,
-1.00524610121804));
#66857=CARTESIAN_POINT('Ctrl Pts',(-0.378093839198509,-0.694975420596321,
-1.01052680569412));
#66858=CARTESIAN_POINT('Ctrl Pts',(-0.493348551701089,-0.632272344423598,
-1.0158075101702));
#66859=CARTESIAN_POINT('Ctrl Pts',(-0.592669505570787,-0.540281378686101,
-1.02108821464627));
#66860=CARTESIAN_POINT('Ctrl Pts',(-0.66400762519825,-0.430162364871081,
-1.02636891912235));
#66861=CARTESIAN_POINT('Ctrl Pts',(-0.735345744825713,-0.320043351056061,
-1.03164962359843));
#66862=CARTESIAN_POINT('Ctrl Pts',(-0.778701030210941,-0.191796289163518,
-1.03693032807451));
#66863=CARTESIAN_POINT('Ctrl Pts',(-0.788813854947635,-0.0609794122270167,
-1.04221103255059));
#66864=CARTESIAN_POINT('Ctrl Pts',(-0.790381527293484,-0.0407004095068838,
-1.04302963809249));
#66865=CARTESIAN_POINT('Ctrl Pts',(-0.791150361490256,-0.020359652444469,
-1.04384824363439));
#66866=CARTESIAN_POINT('Ctrl Pts',(-0.791130810276663,-1.74211169955418E-5,
-1.0446668491763));
#66867=CARTESIAN_POINT('Ctrl Pts',(-0.791143275750807,-1.47194715005396E-5,
-1.0731331508237));
#66868=CARTESIAN_POINT('Ctrl Pts',(-0.791156880058908,-0.0159038930835007,
-1.07249371465737));
#66869=CARTESIAN_POINT('Ctrl Pts',(-0.790687963417032,-0.031792264431447,
-1.07185427849104));
#66870=CARTESIAN_POINT('Ctrl Pts',(-0.78973105947805,-0.0476511913555044,
-1.07121484232471));
#66871=CARTESIAN_POINT('Ctrl Pts',(-0.781828586674952,-0.178620177476483,
-1.06593413784863));
#66872=CARTESIAN_POINT('Ctrl Pts',(-0.74064500007934,-0.307581030951775,
-1.06065343337255));
#66873=CARTESIAN_POINT('Ctrl Pts',(-0.67117646746268,-0.41888892545189,
-1.05537272889647));
#66874=CARTESIAN_POINT('Ctrl Pts',(-0.60170793484602,-0.530196819952006,
-1.05009202442039));
#66875=CARTESIAN_POINT('Ctrl Pts',(-0.503954456208311,-0.623851755476946,
-1.04481131994431));
#66876=CARTESIAN_POINT('Ctrl Pts',(-0.389774949625676,-0.688492026813836,
-1.03953061546824));
#66877=CARTESIAN_POINT('Ctrl Pts',(-0.27559544304304,-0.753132298150725,
-1.03424991099216));
#66878=CARTESIAN_POINT('Ctrl Pts',(-0.144989908515477,-0.788757905299564,
-1.02896920651608));
#66879=CARTESIAN_POINT('Ctrl Pts',(-0.0138026960941072,-0.791046944196395,
-1.02368850204));
#66880=CARTESIAN_POINT('Ctrl Pts',(0.117384516327263,-0.793335983093227,
-1.01840779756392));
#66881=CARTESIAN_POINT('Ctrl Pts',(0.24915340664244,-0.762288453738051,
-1.01312709308784));
#66882=CARTESIAN_POINT('Ctrl Pts',(0.365518492830672,-0.701670872803422,
-1.00784638861177));
#66883=CARTESIAN_POINT('Ctrl Pts',(0.481883579018903,-0.641053291868793,
-1.00256568413569));
#66884=CARTESIAN_POINT('Ctrl Pts',(0.582844861080188,-0.550865659354709,
-0.997284979659609));
#66885=CARTESIAN_POINT('Ctrl Pts',(0.656154267748824,-0.442049046211985,
-0.99200427518353));
#66886=CARTESIAN_POINT('Ctrl Pts',(0.729463674417461,-0.33323243306926,
-0.986723570707451));
#66887=CARTESIAN_POINT('Ctrl Pts',(0.775121205693448,-0.205786839297894,
-0.981442866231373));
#66888=CARTESIAN_POINT('Ctrl Pts',(0.787587939274424,-0.0751732681967957,
-0.976162161755294));
#66889=CARTESIAN_POINT('Ctrl Pts',(0.8000546728554,0.0554403029043047,-0.970881457279216));
#66890=CARTESIAN_POINT('Ctrl Pts',(0.779330608741366,0.189221851335134,
-0.965600752803138));
#66891=CARTESIAN_POINT('Ctrl Pts',(0.727929877190982,0.309941730385962,
-0.960320048327059));
#66892=CARTESIAN_POINT('Ctrl Pts',(0.6765291456406,0.430661609436785,-0.955039343850981));
#66893=CARTESIAN_POINT('Ctrl Pts',(0.594451746653871,0.538319819107605,
-0.949758639374903));
#66894=CARTESIAN_POINT('Ctrl Pts',(0.491654861950048,0.619855853455302,
-0.944477934898824));
#66895=CARTESIAN_POINT('Ctrl Pts',(0.388857977246223,0.701391887803002,
-0.939197230422746));
#66896=CARTESIAN_POINT('Ctrl Pts',(0.265341606825302,0.756805746827579,
-0.933916525946668));
#66897=CARTESIAN_POINT('Ctrl Pts',(0.136090082071649,0.77937492383554,-0.928635821470589));
#66898=CARTESIAN_POINT('Ctrl Pts',(0.00683855731799995,0.8019441008435,
-0.923355116994511));
#66899=CARTESIAN_POINT('Ctrl Pts',(-0.128148121768382,0.791668595834846,
-0.918074412518432));
#66900=CARTESIAN_POINT('Ctrl Pts',(-0.25249410860933,0.749794976950034,
-0.912793708042354));
#66901=CARTESIAN_POINT('Ctrl Pts',(-0.376840095450286,0.707921358065218,
-0.907513003566275));
#66902=CARTESIAN_POINT('Ctrl Pts',(-0.490545390045807,0.63444962530424,
-0.902232299090197));
#66903=CARTESIAN_POINT('Ctrl Pts',(-0.579815887140293,0.538292967965992,
-0.896951594614119));
#66904=CARTESIAN_POINT('Ctrl Pts',(-0.669086384234776,0.442136310627747,
-0.89167089013804));
#66905=CARTESIAN_POINT('Ctrl Pts',(-0.733922083828226,0.323294728712234,
-0.886390185661961));
#66906=CARTESIAN_POINT('Ctrl Pts',(-0.766457472993615,0.196185433797119,
-0.881109481185883));
#66907=CARTESIAN_POINT('Ctrl Pts',(-0.78283868460536,0.132187297883035,
-0.87845070439849));
#66908=CARTESIAN_POINT('Ctrl Pts',(-0.791031728575481,0.0660932867542428,
-0.875791927611097));
#66909=CARTESIAN_POINT('Ctrl Pts',(-0.791032964947078,-4.2330507261862E-7,
-0.873133150823704));
#66910=CARTESIAN_POINT('Origin',(0.,0.,-1.425));
#66911=CARTESIAN_POINT('',(-0.791151924025282,1.20225912425137E-5,-0.644666849176296));
#66912=CARTESIAN_POINT('',(-0.791140835429741,1.53413302099771E-5,-0.673133150823704));
#66913=CARTESIAN_POINT('',(-0.7911,-9.68818082805471E-17,-1.425));
#66914=CARTESIAN_POINT('Ctrl Pts',(-0.791151924025282,1.20225912425137E-5,
-0.644666849176296));
#66915=CARTESIAN_POINT('Ctrl Pts',(-0.791160987250509,0.0123643276965679,
-0.645163965065766));
#66916=CARTESIAN_POINT('Ctrl Pts',(-0.790877649980244,0.0247162168630147,
-0.645661080955236));
#66917=CARTESIAN_POINT('Ctrl Pts',(-0.790299163437089,0.0370542675482504,
-0.646158196844706));
#66918=CARTESIAN_POINT('Ctrl Pts',(-0.784154084306661,0.168117468020605,
-0.651438901320784));
#66919=CARTESIAN_POINT('Ctrl Pts',(-0.744703950154256,0.297619114999562,
-0.656719605796863));
#66920=CARTESIAN_POINT('Ctrl Pts',(-0.676734635769451,0.409848776041709,
-0.662000310272941));
#66921=CARTESIAN_POINT('Ctrl Pts',(-0.608765321384648,0.522078437083854,
-0.66728101474902));
#66922=CARTESIAN_POINT('Ctrl Pts',(-0.512276826767448,0.617036112189189,
-0.672561719225099));
#66923=CARTESIAN_POINT('Ctrl Pts',(-0.398974609042237,0.683202054894812,
-0.677842423701178));
#66924=CARTESIAN_POINT('Ctrl Pts',(-0.28567239131703,0.749367997600434,
-0.683123128177256));
#66925=CARTESIAN_POINT('Ctrl Pts',(-0.155556450483816,0.786742207906344,
-0.688403832653334));
#66926=CARTESIAN_POINT('Ctrl Pts',(-0.0244117417609882,0.79079065076485,
-0.693684537129412));
#66927=CARTESIAN_POINT('Ctrl Pts',(0.106732966961839,0.794839093623355,
-0.69896524160549));
#66928=CARTESIAN_POINT('Ctrl Pts',(0.238906443574278,0.765561769034455,
-0.704245946081569));
#66929=CARTESIAN_POINT('Ctrl Pts',(0.356074123855939,0.706510442097727,
-0.709526650557647));
#66930=CARTESIAN_POINT('Ctrl Pts',(0.473241804137603,0.647459115160997,
-0.714807355033725));
#66931=CARTESIAN_POINT('Ctrl Pts',(0.575403688088487,0.558633785876438,
-0.720088059509804));
#66932=CARTESIAN_POINT('Ctrl Pts',(0.650166053979608,0.450810258008273,
-0.725368763985882));
#66933=CARTESIAN_POINT('Ctrl Pts',(0.724928419870729,0.342986730140108,
-0.730649468461961));
#66934=CARTESIAN_POINT('Ctrl Pts',(0.772291267702086,0.216165003688338,
-0.735930172938039));
#66935=CARTESIAN_POINT('Ctrl Pts',(0.786508795481657,0.0857303977763639,
-0.741210877414117));
#66936=CARTESIAN_POINT('Ctrl Pts',(0.800726323261227,-0.0447042081356141,
-0.746491581890196));
#66937=CARTESIAN_POINT('Ctrl Pts',(0.781798530989006,-0.178751693507805,
-0.751772286366276));
#66938=CARTESIAN_POINT('Ctrl Pts',(0.732021635035464,-0.300150149613334,
-0.757052990842354));
#66939=CARTESIAN_POINT('Ctrl Pts',(0.682244739081924,-0.421548605718856,
-0.762333695318433));
#66940=CARTESIAN_POINT('Ctrl Pts',(0.601618739447067,-0.530298032557726,
-0.76761439979451));
#66941=CARTESIAN_POINT('Ctrl Pts',(0.499924742008656,-0.613205543680484,
-0.772895104270588));
#66942=CARTESIAN_POINT('Ctrl Pts',(0.398230744570239,-0.696113054803247,
-0.778175808746667));
#66943=CARTESIAN_POINT('Ctrl Pts',(0.275468749328266,-0.753178650209894,
-0.783456513222746));
#66944=CARTESIAN_POINT('Ctrl Pts',(0.146531570990962,-0.777479443571225,
-0.788737217698825));
#66945=CARTESIAN_POINT('Ctrl Pts',(0.0175943926536692,-0.801780236932554,
-0.794017922174903));
#66946=CARTESIAN_POINT('Ctrl Pts',(-0.117517968778952,-0.793316228248573,
-0.799298626650981));
#66947=CARTESIAN_POINT('Ctrl Pts',(-0.242414419632999,-0.753114224820442,
-0.804579331127059));
#66948=CARTESIAN_POINT('Ctrl Pts',(-0.367310870487054,-0.712912221392309,
-0.809860035603137));
#66949=CARTESIAN_POINT('Ctrl Pts',(-0.481991410762531,-0.640972223220024,
-0.815140740079216));
#66950=CARTESIAN_POINT('Ctrl Pts',(-0.57254362372496,-0.546021597928866,
-0.820421444555294));
#66951=CARTESIAN_POINT('Ctrl Pts',(-0.663095836687388,-0.451070972637709,
-0.825702149031373));
#66952=CARTESIAN_POINT('Ctrl Pts',(-0.729519722336766,-0.33310972022768,
-0.830982853507451));
#66953=CARTESIAN_POINT('Ctrl Pts',(-0.763757097688803,-0.206448255509406,
-0.83626355798353));
#66954=CARTESIAN_POINT('Ctrl Pts',(-0.781917972250301,-0.139261943799696,
-0.839064655047785));
#66955=CARTESIAN_POINT('Ctrl Pts',(-0.791022636872949,-0.0696276826711715,
-0.841865752112041));
#66956=CARTESIAN_POINT('Ctrl Pts',(-0.791033958661136,3.6737787218466E-6,
-0.844666849176296));
#66957=CARTESIAN_POINT('Ctrl Pts',(-0.791032964947078,-4.2330507261862E-7,
-0.873133150823704));
#66958=CARTESIAN_POINT('Ctrl Pts',(-0.791034184183284,-0.0651781130134306,
-0.870511223135018));
#66959=CARTESIAN_POINT('Ctrl Pts',(-0.783069089680566,-0.130355509939776,
-0.867889295446333));
#66960=CARTESIAN_POINT('Ctrl Pts',(-0.76713419073724,-0.193522390807475,
-0.865267367757648));
#66961=CARTESIAN_POINT('Ctrl Pts',(-0.735040440578149,-0.320743912582239,
-0.859986663281569));
#66962=CARTESIAN_POINT('Ctrl Pts',(-0.670617861522639,-0.43980994821705,
-0.854705958805491));
#66963=CARTESIAN_POINT('Ctrl Pts',(-0.581681848970635,-0.536276056635037,
-0.849425254329413));
#66964=CARTESIAN_POINT('Ctrl Pts',(-0.492745836418631,-0.632742165053023,
-0.844144549853334));
#66965=CARTESIAN_POINT('Ctrl Pts',(-0.379296390370133,-0.706608346254182,
-0.838863845377255));
#66966=CARTESIAN_POINT('Ctrl Pts',(-0.255096577932519,-0.74891355860943,
-0.833583140901176));
#66967=CARTESIAN_POINT('Ctrl Pts',(-0.130896765494906,-0.791218770964677,
-0.828302436425098));
#66968=CARTESIAN_POINT('Ctrl Pts',(0.00405341333182155,-0.801963014474012,
-0.82302173194902));
#66969=CARTESIAN_POINT('Ctrl Pts',(0.133382539981627,-0.779842856202435,
-0.817741027472942));
#66970=CARTESIAN_POINT('Ctrl Pts',(0.262711666631428,-0.757722697930859,
-0.812460322996864));
#66971=CARTESIAN_POINT('Ctrl Pts',(0.386419741104306,-0.702738137878373,
-0.807179618520785));
#66972=CARTESIAN_POINT('Ctrl Pts',(0.489499175527448,-0.621559602532107,
-0.801898914044706));
#66973=CARTESIAN_POINT('Ctrl Pts',(0.592578609950594,-0.540381067185838,
-0.796618209568628));
#66974=CARTESIAN_POINT('Ctrl Pts',(0.675029404324002,-0.433008556545788,
-0.79133750509255));
#66975=CARTESIAN_POINT('Ctrl Pts',(0.72684907863968,-0.312467917109214,
-0.786056800616472));
#66976=CARTESIAN_POINT('Ctrl Pts',(0.778668752955358,-0.191927277672641,
-0.780776096140393));
#66977=CARTESIAN_POINT('Ctrl Pts',(0.799857307213305,-0.0582185094395453,
-0.775495391664314));
#66978=CARTESIAN_POINT('Ctrl Pts',(0.787844261747754,0.0724375701763816,
-0.770214687188236));
#66979=CARTESIAN_POINT('Ctrl Pts',(0.775831216282202,0.203093649792305,
-0.764933982712157));
#66980=CARTESIAN_POINT('Ctrl Pts',(0.73061657109315,0.330697040791069,-0.759653278236079));
#66981=CARTESIAN_POINT('Ctrl Pts',(0.657685519962043,0.439767596776046,
-0.754372573760001));
#66982=CARTESIAN_POINT('Ctrl Pts',(0.584754468830932,0.548838152761029,
-0.749091869283922));
#66983=CARTESIAN_POINT('Ctrl Pts',(0.484107011757771,0.639375873732224,
-0.743811164807844));
#66984=CARTESIAN_POINT('Ctrl Pts',(0.367953148474873,0.700397217919481,
-0.738530460331766));
#66985=CARTESIAN_POINT('Ctrl Pts',(0.251799285191982,0.761418562106735,
-0.733249755855687));
#66986=CARTESIAN_POINT('Ctrl Pts',(0.120139015699353,0.792923529510048,
-0.727969051379608));
#66987=CARTESIAN_POINT('Ctrl Pts',(-0.0110553552671211,0.791090109571494,
-0.722688346903529));
#66988=CARTESIAN_POINT('Ctrl Pts',(-0.142249726233599,0.789256689632941,
-0.717407642427451));
#66989=CARTESIAN_POINT('Ctrl Pts',(-0.272978198673932,0.754084882352523,
-0.712126937951373));
#66990=CARTESIAN_POINT('Ctrl Pts',(-0.387381508380938,0.689841539272919,
-0.706846233475295));
#66991=CARTESIAN_POINT('Ctrl Pts',(-0.501784818087942,0.625598196193318,
-0.701565528999217));
#66992=CARTESIAN_POINT('Ctrl Pts',(-0.599862965061619,0.532283317314533,
-0.696284824523138));
#66993=CARTESIAN_POINT('Ctrl Pts',(-0.669717644236744,0.421217354034596,
-0.69100412004706));
#66994=CARTESIAN_POINT('Ctrl Pts',(-0.739572323411872,0.310151390754656,
-0.685723415570981));
#66995=CARTESIAN_POINT('Ctrl Pts',(-0.781203534788445,0.181334343073565,
-0.680442711094903));
#66996=CARTESIAN_POINT('Ctrl Pts',(-0.789560807201604,0.0503935915873558,
-0.675162006618824));
#66997=CARTESIAN_POINT('Ctrl Pts',(-0.790631100041234,0.0336243705062366,
-0.674485721353784));
#66998=CARTESIAN_POINT('Ctrl Pts',(-0.791155659727199,0.0168203180943188,
-0.673809436088744));
#66999=CARTESIAN_POINT('Ctrl Pts',(-0.791140835429741,1.53413302099771E-5,
-0.673133150823704));
#67000=CARTESIAN_POINT('Origin',(0.,0.,-1.425));
#67001=CARTESIAN_POINT('',(-0.791079804116067,-1.96820758422422E-5,-0.444666849176296));
#67002=CARTESIAN_POINT('',(-0.791093201014614,-2.03057722054419E-5,-0.473133150823703));
#67003=CARTESIAN_POINT('',(-0.7911,-9.68818082805471E-17,-1.425));
#67004=CARTESIAN_POINT('Ctrl Pts',(-0.791079804116067,-1.96820758422422E-5,
-0.444666849176296));
#67005=CARTESIAN_POINT('Ctrl Pts',(-0.790990645563059,0.0943112144519883,
-0.448462178019491));
#67006=CARTESIAN_POINT('Ctrl Pts',(-0.774106485915666,0.188673174257029,
-0.452257506862687));
#67007=CARTESIAN_POINT('Ctrl Pts',(-0.7410897206494,0.277005076527925,-0.456052835705883));
#67008=CARTESIAN_POINT('Ctrl Pts',(-0.695151203242722,0.399907383804603,
-0.461333540181961));
#67009=CARTESIAN_POINT('Ctrl Pts',(-0.617981431816262,0.511136049324216,
-0.46661424465804));
#67010=CARTESIAN_POINT('Ctrl Pts',(-0.518942221524803,0.597197418942259,
-0.471894949134119));
#67011=CARTESIAN_POINT('Ctrl Pts',(-0.41990301123335,0.683258788560297,
-0.477175653610197));
#67012=CARTESIAN_POINT('Ctrl Pts',(-0.298994362076898,0.744152862276769,
-0.482456358086275));
#67013=CARTESIAN_POINT('Ctrl Pts',(-0.170884250937674,0.772492303686205,
-0.487737062562353));
#67014=CARTESIAN_POINT('Ctrl Pts',(-0.0427741397984416,0.800831745095644,
-0.493017767038432));
#67015=CARTESIAN_POINT('Ctrl Pts',(0.0925374333235549,0.796616554198045,
-0.49829847151451));
#67016=CARTESIAN_POINT('Ctrl Pts',(0.218635207479237,0.760358094928631,
-0.503579175990589));
#67017=CARTESIAN_POINT('Ctrl Pts',(0.344732981634912,0.724099635659218,
-0.508859880466667));
#67018=CARTESIAN_POINT('Ctrl Pts',(0.461616956824271,0.655797908017987,
-0.514140584942746));
#67019=CARTESIAN_POINT('Ctrl Pts',(0.555107407625345,0.563738904522544,
-0.519421289418824));
#67020=CARTESIAN_POINT('Ctrl Pts',(0.648597858426425,0.471679901027096,
-0.524701993894903));
#67021=CARTESIAN_POINT('Ctrl Pts',(0.718694784839222,0.355863621677439,
-0.529982698370981));
#67022=CARTESIAN_POINT('Ctrl Pts',(0.756894410636733,0.230340264868805,
-0.53526340284706));
#67023=CARTESIAN_POINT('Ctrl Pts',(0.795094036434242,0.104816908060178,
-0.540544107323138));
#67024=CARTESIAN_POINT('Ctrl Pts',(0.801396361616462,-0.0304135262074155,
-0.545824811799215));
#67025=CARTESIAN_POINT('Ctrl Pts',(0.775036822517206,-0.158945620308655,
-0.551105516275294));
#67026=CARTESIAN_POINT('Ctrl Pts',(0.74867728341795,-0.287477714409898,
-0.556386220751372));
#67027=CARTESIAN_POINT('Ctrl Pts',(0.689655880037216,-0.40931146834479,
-0.561666925227452));
#67028=CARTESIAN_POINT('Ctrl Pts',(0.605132766644463,-0.509666676570216,
-0.56694762970353));
#67029=CARTESIAN_POINT('Ctrl Pts',(0.520609653251709,-0.610021884795641,
-0.572228334179609));
#67030=CARTESIAN_POINT('Ctrl Pts',(0.410584829846934,-0.688898547311603,
-0.577509038655687));
#67031=CARTESIAN_POINT('Ctrl Pts',(0.288405907024508,-0.736727778264311,
-0.582789743131765));
#67032=CARTESIAN_POINT('Ctrl Pts',(0.166226984202082,-0.784557009217019,
-0.588070447607843));
#67033=CARTESIAN_POINT('Ctrl Pts',(0.0318939619620019,-0.801338808606473,
-0.593351152083922));
#67034=CARTESIAN_POINT('Ctrl Pts',(-0.0982966111957519,-0.785037300196832,
-0.59863185656));
#67035=CARTESIAN_POINT('Ctrl Pts',(-0.228487184353502,-0.768735791787191,
-0.603912561036079));
#67036=CARTESIAN_POINT('Ctrl Pts',(-0.354535308428928,-0.719350975578457,
-0.609193265512157));
#67037=CARTESIAN_POINT('Ctrl Pts',(-0.461149513513319,-0.642873947721737,
-0.614473969988235));
#67038=CARTESIAN_POINT('Ctrl Pts',(-0.567763718597715,-0.566396919865013,
-0.619754674464314));
#67039=CARTESIAN_POINT('Ctrl Pts',(-0.654944004691074,-0.462827680360298,
-0.625035378940393));
#67040=CARTESIAN_POINT('Ctrl Pts',(-0.712114135683525,-0.344730683625065,
-0.630316083416471));
#67041=CARTESIAN_POINT('Ctrl Pts',(-0.76390237479996,-0.237751122800469,
-0.635099672003079));
#67042=CARTESIAN_POINT('Ctrl Pts',(-0.791064711482551,-0.118850292960821,
-0.639883260589688));
#67043=CARTESIAN_POINT('Ctrl Pts',(-0.791151924025282,1.20225912425137E-5,
-0.644666849176296));
#67044=CARTESIAN_POINT('Ctrl Pts',(-0.791140835429741,1.53413302099771E-5,
-0.673133150823704));
#67045=CARTESIAN_POINT('Ctrl Pts',(-0.791039905713343,-0.11439962799359,
-0.668528731612665));
#67046=CARTESIAN_POINT('Ctrl Pts',(-0.765936218386557,-0.228857445000086,
-0.663924312401627));
#67047=CARTESIAN_POINT('Ctrl Pts',(-0.717833561436095,-0.332657121399638,
-0.659319893190589));
#67048=CARTESIAN_POINT('Ctrl Pts',(-0.662665709807682,-0.451702627609097,
-0.654039188714511));
#67049=CARTESIAN_POINT('Ctrl Pts',(-0.577246673101113,-0.556729184736689,
-0.648758484238432));
#67050=CARTESIAN_POINT('Ctrl Pts',(-0.47193902227101,-0.634995544551145,
-0.643477779762354));
#67051=CARTESIAN_POINT('Ctrl Pts',(-0.366631371440906,-0.7132619043656,
-0.638197075286275));
#67052=CARTESIAN_POINT('Ctrl Pts',(-0.241435106487268,-0.764768066866919,
-0.632916370810197));
#67053=CARTESIAN_POINT('Ctrl Pts',(-0.111538354423194,-0.783265585759063,
-0.627635666334118));
#67054=CARTESIAN_POINT('Ctrl Pts',(0.0183583976408846,-0.801763104651207,
-0.62235496185804));
#67055=CARTESIAN_POINT('Ctrl Pts',(0.1529556368154,-0.787251979934175,-0.617074257381961));
#67056=CARTESIAN_POINT('Ctrl Pts',(0.275924761245081,-0.741492621995504,
-0.611793552905882));
#67057=CARTESIAN_POINT('Ctrl Pts',(0.398893885674758,-0.695733264056833,
-0.606512848429804));
#67058=CARTESIAN_POINT('Ctrl Pts',(0.510234895359602,-0.618725672896525,
-0.601232143953725));
#67059=CARTESIAN_POINT('Ctrl Pts',(0.596440507175103,-0.519811988840799,
-0.595951439477647));
#67060=CARTESIAN_POINT('Ctrl Pts',(0.682646118990602,-0.420898304785076,
-0.590670735001569));
#67061=CARTESIAN_POINT('Ctrl Pts',(0.743716332936759,-0.300078527833936,
-0.585390030525491));
#67062=CARTESIAN_POINT('Ctrl Pts',(0.772242444237319,-0.172009853381406,
-0.580109326049412));
#67063=CARTESIAN_POINT('Ctrl Pts',(0.80076855553788,-0.0439411789288734,
-0.574828621573334));
#67064=CARTESIAN_POINT('Ctrl Pts',(0.796750564192842,0.0913763930250492,
-0.569547917097255));
#67065=CARTESIAN_POINT('Ctrl Pts',(0.760675910964986,0.217526873786918,
-0.564267212621177));
#67066=CARTESIAN_POINT('Ctrl Pts',(0.72460125773713,0.343677354548784,-0.558986508145099));
#67067=CARTESIAN_POINT('Ctrl Pts',(0.656469942626458,0.460660744118596,
-0.55370580366902));
#67068=CARTESIAN_POINT('Ctrl Pts',(0.564547284633123,0.554285256664192,
-0.548425099192942));
#67069=CARTESIAN_POINT('Ctrl Pts',(0.472624626639786,0.647909769209791,
-0.543144394716863));
#67070=CARTESIAN_POINT('Ctrl Pts',(0.356910625763784,0.718175404731173,
-0.537863690240785));
#67071=CARTESIAN_POINT('Ctrl Pts',(0.231443072534656,0.756557920134102,
-0.532582985764707));
#67072=CARTESIAN_POINT('Ctrl Pts',(0.105975519305528,0.794940435537032,
-0.527302281288628));
#67073=CARTESIAN_POINT('Ctrl Pts',(-0.0292455862767264,0.80143983082151,
-0.52202157681255));
#67074=CARTESIAN_POINT('Ctrl Pts',(-0.157815958291974,0.775267634852832,
-0.516740872336471));
#67075=CARTESIAN_POINT('Ctrl Pts',(-0.286386330307222,0.749095438884155,
-0.511460167860393));
#67076=CARTESIAN_POINT('Ctrl Pts',(-0.408305968755463,0.690251651662321,
-0.506179463384315));
#67077=CARTESIAN_POINT('Ctrl Pts',(-0.508784249053499,0.605874880034648,
-0.500898758908236));
#67078=CARTESIAN_POINT('Ctrl Pts',(-0.609262529351534,0.521498108406975,
-0.495618054432158));
#67079=CARTESIAN_POINT('Ctrl Pts',(-0.688299451499364,0.411588352373463,
-0.490337349956079));
#67080=CARTESIAN_POINT('Ctrl Pts',(-0.736306687820121,0.289479263183488,
-0.48505664548));
#67081=CARTESIAN_POINT('Ctrl Pts',(-0.772439116004476,0.197574412291118,
-0.481082147261235));
#67082=CARTESIAN_POINT('Ctrl Pts',(-0.790993997334175,0.0987589419568265,
-0.477107649042469));
#67083=CARTESIAN_POINT('Ctrl Pts',(-0.791093201014614,-2.03057722054419E-5,
-0.473133150823703));
#67084=CARTESIAN_POINT('Origin',(0.,0.,-1.425));
#67085=CARTESIAN_POINT('',(-0.791058280240756,1.64158700123596E-5,-0.244666849176296));
#67086=CARTESIAN_POINT('',(-0.791048813772023,1.36328575649638E-5,-0.273133150823704));
#67087=CARTESIAN_POINT('',(-0.7911,-9.68818082805471E-17,-1.425));
#67088=CARTESIAN_POINT('Ctrl Pts',(-0.791058280240756,1.64158700123596E-5,
-0.244666849176296));
#67089=CARTESIAN_POINT('Ctrl Pts',(-0.791092359377555,0.0450770503401576,
-0.246479686497138));
#67090=CARTESIAN_POINT('Ctrl Pts',(-0.787306067959793,0.0901320191018208,
-0.248292523817981));
#67091=CARTESIAN_POINT('Ctrl Pts',(-0.779647639886365,0.134518896239813,
-0.250105361138824));
#67092=CARTESIAN_POINT('Ctrl Pts',(-0.757339021820034,0.26381565005596,
-0.255386065614902));
#67093=CARTESIAN_POINT('Ctrl Pts',(-0.702174248899364,0.387443460909541,
-0.260666770090981));
#67094=CARTESIAN_POINT('Ctrl Pts',(-0.620845581003012,0.490404481077766,
-0.265947474567059));
#67095=CARTESIAN_POINT('Ctrl Pts',(-0.539516913106655,0.593365501245996,
-0.271228179043138));
#67096=CARTESIAN_POINT('Ctrl Pts',(-0.432024350234614,0.675659730728867,
-0.276508883519216));
#67097=CARTESIAN_POINT('Ctrl Pts',(-0.311408317767632,0.727303681583887,
-0.281789587995295));
#67098=CARTESIAN_POINT('Ctrl Pts',(-0.190792285300657,0.778947632438904,
-0.287070292471373));
#67099=CARTESIAN_POINT('Ctrl Pts',(-0.0570527832387434,0.799941304666074,
-0.292350996947451));
#67100=CARTESIAN_POINT('Ctrl Pts',(0.0735856500869722,0.787737861403673,
-0.29763170142353));
#67101=CARTESIAN_POINT('Ctrl Pts',(0.204224083412692,0.775534418141272,
-0.302912405899608));
#67102=CARTESIAN_POINT('Ctrl Pts',(0.331761448002213,0.730133859389297,
-0.308193110375687));
#67103=CARTESIAN_POINT('Ctrl Pts',(0.440725603578711,0.657043932549396,
-0.313473814851765));
#67104=CARTESIAN_POINT('Ctrl Pts',(0.549689759155209,0.583954005709496,
-0.318754519327844));
#67105=CARTESIAN_POINT('Ctrl Pts',(0.640080705718686,0.483174710781668,
-0.324035223803922));
#67106=CARTESIAN_POINT('Ctrl Pts',(0.700932709326926,0.366932041549318,
-0.32931592828));
#67107=CARTESIAN_POINT('Ctrl Pts',(0.761784712935166,0.250689372316969,
-0.334596632756079));
#67108=CARTESIAN_POINT('Ctrl Pts',(0.793097773588171,0.118983328780098,
-0.339877337232157));
#67109=CARTESIAN_POINT('Ctrl Pts',(0.791073160808736,-0.0122082313716788,
-0.345158041708236));
#67110=CARTESIAN_POINT('Ctrl Pts',(0.789048548029301,-0.143399791523455,
-0.350438746184314));
#67111=CARTESIAN_POINT('Ctrl Pts',(0.753686261817425,-0.274076868290138,
-0.355719450660393));
#67112=CARTESIAN_POINT('Ctrl Pts',(0.689276262087855,-0.38838643245431,
-0.361000155136471));
#67113=CARTESIAN_POINT('Ctrl Pts',(0.624866262358284,-0.502695996618483,
-0.36628085961255));
#67114=CARTESIAN_POINT('Ctrl Pts',(0.531408549111018,-0.600638048180145,
-0.371561564088628));
#67115=CARTESIAN_POINT('Ctrl Pts',(0.420240901370344,-0.670330792452888,
-0.376842268564706));
#67116=CARTESIAN_POINT('Ctrl Pts',(0.309073253629671,-0.74002353672563,
-0.382122973040785));
#67117=CARTESIAN_POINT('Ctrl Pts',(0.180195671395589,-0.781466973709453,
-0.387403677516863));
#67118=CARTESIAN_POINT('Ctrl Pts',(0.049242879117497,-0.789633411989491,
-0.392684381992942));
#67119=CARTESIAN_POINT('Ctrl Pts',(-0.0817099131605952,-0.79779985026953,
-0.39796508646902));
#67120=CARTESIAN_POINT('Ctrl Pts',(-0.214737915482698,-0.772689289845784,
-0.403245790945098));
#67121=CARTESIAN_POINT('Ctrl Pts',(-0.333702897304227,-0.717348006756114,
-0.408526495421177));
#67122=CARTESIAN_POINT('Ctrl Pts',(-0.452667879125756,-0.662006723666444,
-0.413807199897256));
#67123=CARTESIAN_POINT('Ctrl Pts',(-0.557569840446711,-0.576434717910848,
-0.419087904373334));
#67124=CARTESIAN_POINT('Ctrl Pts',(-0.635682648284223,-0.471013117809877,
-0.424368608849413));
#67125=CARTESIAN_POINT('Ctrl Pts',(-0.713795456121733,-0.365591517708909,
-0.429649313325491));
#67126=CARTESIAN_POINT('Ctrl Pts',(-0.765119110475802,-0.240320323262568,
-0.434930017801569));
#67127=CARTESIAN_POINT('Ctrl Pts',(-0.783427305959389,-0.110396751522529,
-0.440210722277647));
#67128=CARTESIAN_POINT('Ctrl Pts',(-0.788577101327898,-0.0738513798824403,
-0.44169609791053));
#67129=CARTESIAN_POINT('Ctrl Pts',(-0.791114698046889,-0.0369379099605336,
-0.443181473543413));
#67130=CARTESIAN_POINT('Ctrl Pts',(-0.791079804116067,-1.96820758422422E-5,
-0.444666849176296));
#67131=CARTESIAN_POINT('Ctrl Pts',(-0.791093201014614,-2.03057722054419E-5,
-0.473133150823703));
#67132=CARTESIAN_POINT('Ctrl Pts',(-0.791125803990136,-0.0324837928275328,
-0.471826944566391));
#67133=CARTESIAN_POINT('Ctrl Pts',(-0.789165032446283,-0.0649433675248466,
-0.470520738309078));
#67134=CARTESIAN_POINT('Ctrl Pts',(-0.785179715610441,-0.0971524396805776,
-0.469214532051765));
#67135=CARTESIAN_POINT('Ctrl Pts',(-0.76906795658632,-0.227366631008214,
-0.463933827575687));
#67136=CARTESIAN_POINT('Ctrl Pts',(-0.719866888044401,-0.353486591317053,
-0.458653123099608));
#67137=CARTESIAN_POINT('Ctrl Pts',(-0.643545314872834,-0.460212135918921,
-0.45337241862353));
#67138=CARTESIAN_POINT('Ctrl Pts',(-0.567223741701267,-0.566937680520788,
-0.448091714147451));
#67139=CARTESIAN_POINT('Ctrl Pts',(-0.463781663900054,-0.654268809415684,
-0.442811009671373));
#67140=CARTESIAN_POINT('Ctrl Pts',(-0.345768109322771,-0.711610987069034,
-0.437530305195295));
#67141=CARTESIAN_POINT('Ctrl Pts',(-0.227754554745487,-0.768953164722383,
-0.432249600719217));
#67142=CARTESIAN_POINT('Ctrl Pts',(-0.0951695233921332,-0.796306391134186,
-0.426968896243139));
#67143=CARTESIAN_POINT('Ctrl Pts',(0.0359024929425398,-0.790352322285754,
-0.42168819176706));
#67144=CARTESIAN_POINT('Ctrl Pts',(0.16697450927722,-0.784398253437322,
-0.416407487290981));
#67145=CARTESIAN_POINT('Ctrl Pts',(0.29653351059322,-0.74513688932865,-0.411126782814903));
#67146=CARTESIAN_POINT('Ctrl Pts',(0.408862106534589,-0.67733120419888,
-0.405846078338824));
#67147=CARTESIAN_POINT('Ctrl Pts',(0.521190702475954,-0.609525519069113,
-0.400565373862746));
#67148=CARTESIAN_POINT('Ctrl Pts',(0.616288893042691,-0.513175512918248,
-0.395284669386668));
#67149=CARTESIAN_POINT('Ctrl Pts',(0.682619885199034,-0.399969842206072,
-0.390003964910589));
#67150=CARTESIAN_POINT('Ctrl Pts',(0.748950877355374,-0.286764171493899,
-0.384723260434511));
#67151=CARTESIAN_POINT('Ctrl Pts',(0.786514671101322,-0.156702836220414,
-0.379442555958432));
#67152=CARTESIAN_POINT('Ctrl Pts',(0.790754232170835,-0.025564167156415,
-0.374161851482354));
#67153=CARTESIAN_POINT('Ctrl Pts',(0.794993793240347,0.105574501907587,
-0.368881147006275));
#67154=CARTESIAN_POINT('Ctrl Pts',(0.765909121633421,0.237790504762104,
-0.363600442530197));
#67155=CARTESIAN_POINT('Ctrl Pts',(0.707028610824429,0.355044118136598,
-0.358319738054119));
#67156=CARTESIAN_POINT('Ctrl Pts',(0.648148100015436,0.472297731511095,
-0.35303903357804));
#67157=CARTESIAN_POINT('Ctrl Pts',(0.559471750004376,0.57458895540557,-0.347758329101962));
#67158=CARTESIAN_POINT('Ctrl Pts',(0.451757291238583,0.6495083772731,-0.342477624625883));
#67159=CARTESIAN_POINT('Ctrl Pts',(0.34404283247279,0.72442779914063,-0.337196920149804));
#67160=CARTESIAN_POINT('Ctrl Pts',(0.217290264952266,0.771975418981217,
-0.331916215673726));
#67161=CARTESIAN_POINT('Ctrl Pts',(0.086876517748351,0.786383019276778,
-0.326635511197647));
#67162=CARTESIAN_POINT('Ctrl Pts',(-0.0435372294555523,0.800790619572338,
-0.321354806721569));
#67163=CARTESIAN_POINT('Ctrl Pts',(-0.177612156342845,0.782058200322878,
-0.316074102245491));
#67164=CARTESIAN_POINT('Ctrl Pts',(-0.299083024998013,0.732458276301435,
-0.310793397769413));
#67165=CARTESIAN_POINT('Ctrl Pts',(-0.420553893653188,0.682858352279989,
-0.305512693293334));
#67166=CARTESIAN_POINT('Ctrl Pts',(-0.529420704076237,0.602390923486555,
-0.300231988817256));
#67167=CARTESIAN_POINT('Ctrl Pts',(-0.612476329745163,0.500817858869168,
-0.294951284341177));
#67168=CARTESIAN_POINT('Ctrl Pts',(-0.69553195541409,0.399244794251781,
-0.289670579865099));
#67169=CARTESIAN_POINT('Ctrl Pts',(-0.752776396328893,0.276566093810441,
-0.284389875389021));
#67170=CARTESIAN_POINT('Ctrl Pts',(-0.777265069084892,0.147664467346652,
-0.279109170912942));
#67171=CARTESIAN_POINT('Ctrl Pts',(-0.786502775973659,0.0990397233835045,
-0.277117164216529));
#67172=CARTESIAN_POINT('Ctrl Pts',(-0.791079412605933,0.049529471400793,
-0.275125157520117));
#67173=CARTESIAN_POINT('Ctrl Pts',(-0.791048813772023,1.36328575649638E-5,
-0.273133150823704));
#67174=CARTESIAN_POINT('Origin',(0.,0.,-1.425));
#67175=CARTESIAN_POINT('',(-0.7911,-9.68818082805471E-17,-0.0600000000000001));
#67176=CARTESIAN_POINT('',(-0.79116656670867,1.93884184799344E-7,-0.0731331508237035));
#67177=CARTESIAN_POINT('',(-0.7911,-9.68818082805471E-17,-1.425));
#67178=CARTESIAN_POINT('',(-0.701077753000064,0.366509473613413,-0.0600000000000001));
#67179=CARTESIAN_POINT('Origin',(0.,0.,-0.0600000000000001));
#67180=CARTESIAN_POINT('Ctrl Pts',(-0.701077753000059,0.366509473613423,
-0.0600000000000005));
#67181=CARTESIAN_POINT('Ctrl Pts',(-0.640274482293033,0.4828170276367,-0.0652807044760789));
#67182=CARTESIAN_POINT('Ctrl Pts',(-0.550002542754869,0.58364484092056,
-0.0705614089521573));
#67183=CARTESIAN_POINT('Ctrl Pts',(-0.441098388580055,0.656795701812313,
-0.0758421134282357));
#67184=CARTESIAN_POINT('Ctrl Pts',(-0.332194234405237,0.729946562704068,
-0.0811228179043143));
#67185=CARTESIAN_POINT('Ctrl Pts',(-0.204657865593779,0.775420471203709,
-0.0864035223803925));
#67186=CARTESIAN_POINT('Ctrl Pts',(-0.0740199674866195,0.787697328927234,
-0.0916842268564711));
#67187=CARTESIAN_POINT('Ctrl Pts',(0.0566179306205331,0.799974186650757,
-0.0969649313325495));
#67188=CARTESIAN_POINT('Ctrl Pts',(0.190357358023387,0.77905399359816,-0.102245635808628));
#67189=CARTESIAN_POINT('Ctrl Pts',(0.310999283790884,0.727477099691021,
-0.107526340284706));
#67190=CARTESIAN_POINT('Ctrl Pts',(0.431641209558384,0.67590020578388,-0.112807044760785));
#67191=CARTESIAN_POINT('Ctrl Pts',(0.539185633690539,0.593666611022195,
-0.118087749236863));
#67192=CARTESIAN_POINT('Ctrl Pts',(0.620573231636201,0.490751159083177,
-0.123368453712942));
#67193=CARTESIAN_POINT('Ctrl Pts',(0.701960829581863,0.387835707144159,
-0.12864915818902));
#67194=CARTESIAN_POINT('Ctrl Pts',(0.757191601341032,0.264238398027809,
-0.133929862665099));
#67195=CARTESIAN_POINT('Ctrl Pts',(0.779571649374987,0.134954042504121,
-0.139210567141177));
#67196=CARTESIAN_POINT('Ctrl Pts',(0.801951697408941,0.0056696869804328,
-0.144491271617255));
#67197=CARTESIAN_POINT('Ctrl Pts',(0.791481021717682,-0.129301714950592,
-0.149771976093334));
#67198=CARTESIAN_POINT('Ctrl Pts',(0.749426610355531,-0.253586506955687,
-0.155052680569412));
#67199=CARTESIAN_POINT('Ctrl Pts',(0.70737219899338,-0.377871298960781,
-0.160333385045491));
#67200=CARTESIAN_POINT('Ctrl Pts',(0.633734051960338,-0.491469481039944,
-0.165614089521569));
#67201=CARTESIAN_POINT('Ctrl Pts',(0.537447206462403,-0.580599770531476,
-0.170894793997648));
#67202=CARTESIAN_POINT('Ctrl Pts',(0.441160360964469,-0.669730060023005,
-0.176175498473726));
#67203=CARTESIAN_POINT('Ctrl Pts',(0.322224817001643,-0.734392456926904,
-0.181456202949804));
#67204=CARTESIAN_POINT('Ctrl Pts',(0.195068339550481,-0.766742559953149,
-0.186736907425883));
#67205=CARTESIAN_POINT('Ctrl Pts',(0.0679118620993177,-0.799092662979395,
-0.192017611901961));
#67206=CARTESIAN_POINT('Ctrl Pts',(-0.0674655488401824,-0.799130472127987,
-0.197298316378039));
#67207=CARTESIAN_POINT('Ctrl Pts',(-0.194640214369627,-0.766851356011745,
-0.202579020854118));
#67208=CARTESIAN_POINT('Ctrl Pts',(-0.321814879899078,-0.734572239895501,
-0.207859725330196));
#67209=CARTESIAN_POINT('Ctrl Pts',(-0.440786800018474,-0.669976198514418,
-0.213140429806275));
#67210=CARTESIAN_POINT('Ctrl Pts',(-0.537123170784641,-0.580899693490615,
-0.218421134282353));
#67211=CARTESIAN_POINT('Ctrl Pts',(-0.633459541550805,-0.491823188466814,
-0.223701838758432));
#67212=CARTESIAN_POINT('Ctrl Pts',(-0.707160362963742,-0.378266219800294,
-0.22898254323451));
#67213=CARTESIAN_POINT('Ctrl Pts',(-0.749284542064215,-0.254004887077675,
-0.234263247710589));
#67214=CARTESIAN_POINT('Ctrl Pts',(-0.776947718029759,-0.172401798632439,
-0.237731114865824));
#67215=CARTESIAN_POINT('Ctrl Pts',(-0.790993088555972,-0.0861823248975552,
-0.24119898202106));
#67216=CARTESIAN_POINT('Ctrl Pts',(-0.791058280240756,1.64158700123596E-5,
-0.244666849176296));
#67217=CARTESIAN_POINT('Ctrl Pts',(-0.791048813772023,1.36328575649638E-5,
-0.273133150823704));
#67218=CARTESIAN_POINT('Ctrl Pts',(-0.790998296714364,-0.0817343997010853,
-0.269844453044038));
#67219=CARTESIAN_POINT('Ctrl Pts',(-0.778390176603752,-0.163497659137093,
-0.266555755264372));
#67220=CARTESIAN_POINT('Ctrl Pts',(-0.753466702744765,-0.24131661741456,
-0.263267057484707));
#67221=CARTESIAN_POINT('Ctrl Pts',(-0.713446759051444,-0.366271523225744,
-0.257986353008628));
#67222=CARTESIAN_POINT('Ctrl Pts',(-0.641673967067604,-0.481056782361877,
-0.25270564853255));
#67223=CARTESIAN_POINT('Ctrl Pts',(-0.546855407894365,-0.571747274308673,
-0.247424944056471));
#67224=CARTESIAN_POINT('Ctrl Pts',(-0.452036848721127,-0.662437766255469,
-0.242144239580393));
#67225=CARTESIAN_POINT('Ctrl Pts',(-0.334172522358488,-0.72903349101293,
-0.236863535104314));
#67226=CARTESIAN_POINT('Ctrl Pts',(-0.20756108896749,-0.763455418739467,
-0.231582830628236));
#67227=CARTESIAN_POINT('Ctrl Pts',(-0.0809496555764887,-0.797877346466006,
-0.226302126152158));
#67228=CARTESIAN_POINT('Ctrl Pts',(0.0544088848428741,-0.800125477161621,
-0.221021421676079));
#67229=CARTESIAN_POINT('Ctrl Pts',(0.18209358115504,-0.769927080430184,
-0.2157407172));
#67230=CARTESIAN_POINT('Ctrl Pts',(0.309778277467199,-0.739728683698749,
-0.210460012723922));
#67231=CARTESIAN_POINT('Ctrl Pts',(0.429789129672164,-0.677083759540267,
-0.205179308247844));
#67232=CARTESIAN_POINT('Ctrl Pts',(0.52756706174467,-0.589592046913208,
-0.199898603771765));
#67233=CARTESIAN_POINT('Ctrl Pts',(0.625344993817177,-0.50210033428615,
-0.194617899295687));
#67234=CARTESIAN_POINT('Ctrl Pts',(0.700890005757226,-0.389761833190513,
-0.189337194819609));
#67235=CARTESIAN_POINT('Ctrl Pts',(0.745037418710249,-0.266204839038066,
-0.18405649034353));
#67236=CARTESIAN_POINT('Ctrl Pts',(0.789184831663272,-0.142647844885616,
-0.178775785867452));
#67237=CARTESIAN_POINT('Ctrl Pts',(0.801934645629268,-0.00787235767636212,
-0.173495081391374));
#67238=CARTESIAN_POINT('Ctrl Pts',(0.781740065251379,0.121771400732141,
-0.168214376915295));
#67239=CARTESIAN_POINT('Ctrl Pts',(0.76154548487349,0.251415159140645,-0.162933672439217));
#67240=CARTESIAN_POINT('Ctrl Pts',(0.708406510151714,0.37592718874839,-0.157652967963138));
#67241=CARTESIAN_POINT('Ctrl Pts',(0.628769784162815,0.480202362242657,
-0.15237226348706));
#67242=CARTESIAN_POINT('Ctrl Pts',(0.549133058173913,0.584477535736926,
-0.147091559010981));
#67243=CARTESIAN_POINT('Ctrl Pts',(0.442998580917885,0.668515853117719,
-0.141810854534903));
#67244=CARTESIAN_POINT('Ctrl Pts',(0.323241785950906,0.722122260438018,
-0.136530150058825));
#67245=CARTESIAN_POINT('Ctrl Pts',(0.203484990983934,0.775728667758313,
-0.131249445582746));
#67246=CARTESIAN_POINT('Ctrl Pts',(0.0701058783059993,0.79890316501812,
-0.125968741106667));
#67247=CARTESIAN_POINT('Ctrl Pts',(-0.0607142922230027,0.788834318036469,
-0.120688036630589));
#67248=CARTESIAN_POINT('Ctrl Pts',(-0.191534462752012,0.778765471054817,
-0.11540733215451));
#67249=CARTESIAN_POINT('Ctrl Pts',(-0.319795691132091,0.735453279831711,
-0.110126627678432));
#67250=CARTESIAN_POINT('Ctrl Pts',(-0.429938877917322,0.664152203157782,
-0.104845923202354));
#67251=CARTESIAN_POINT('Ctrl Pts',(-0.54008206470255,0.592851126483854,
-0.0995652187262753));
#67252=CARTESIAN_POINT('Ctrl Pts',(-0.632107209892923,0.493561164359106,
-0.0942845142501968));
#67253=CARTESIAN_POINT('Ctrl Pts',(-0.694848653928772,0.378327514286356,
-0.0890038097741183));
#67254=CARTESIAN_POINT('Ctrl Pts',(-0.757703150259721,0.262886227478213,
-0.0837135901239801));
#67255=CARTESIAN_POINT('Ctrl Pts',(-0.791168292937371,0.13144374384189,
-0.0784233704738418));
#67256=CARTESIAN_POINT('Ctrl Pts',(-0.79116656670867,1.93884184799344E-7,
-0.0731331508237035));
#67257=CARTESIAN_POINT('Origin',(0.,0.,-3.278617978381));
#67258=CARTESIAN_POINT('',(-0.676664313283933,1.40419911898121E-5,-0.178617978381002));
#67259=CARTESIAN_POINT('',(-0.676756940578634,1.65846773781623E-7,-0.139182021618995));
#67260=CARTESIAN_POINT('',(-0.6767,-6.21087748740391E-14,-3.278617978381));
#67261=CARTESIAN_POINT('',(0.564220937616133,0.373642629516334,-0.06));
#67262=CARTESIAN_POINT('Ctrl Pts',(-0.676664313283933,1.40419911898067E-5,
-0.178617978381002));
#67263=CARTESIAN_POINT('Ctrl Pts',(-0.676608548888669,-0.0737196046747348,
-0.175150111225766));
#67264=CARTESIAN_POINT('Ctrl Pts',(-0.646299473199053,-0.259776109946148,
-0.166401539594452));
#67265=CARTESIAN_POINT('Ctrl Pts',(-0.478812698669308,-0.517836875656849,
-0.15237226348706));
#67266=CARTESIAN_POINT('Ctrl Pts',(-0.173510088336382,-0.683601537024222,
-0.136530150058825));
#67267=CARTESIAN_POINT('Ctrl Pts',(0.173891860782926,-0.683504512182157,
-0.120688036630589));
#67268=CARTESIAN_POINT('Ctrl Pts',(0.479101123580215,-0.517569571018445,
-0.104845923202354));
#67269=CARTESIAN_POINT('Ctrl Pts',(0.668069398503454,-0.226056905819471,
-0.0890038097741189));
#67270=CARTESIAN_POINT('Ctrl Pts',(0.693423565747112,0.100768945594041,
-0.0740551687066675));
#67271=CARTESIAN_POINT('Ctrl Pts',(0.615633638736097,0.295835894939612,
-0.0643872321152945));
#67272=CARTESIAN_POINT('Ctrl Pts',(0.564220937616133,0.373642629516334,
-0.06));
#67273=CARTESIAN_POINT('',(0.5370608629359,-0.411689834101531,-0.0600000000000001));
#67274=CARTESIAN_POINT('Origin',(0.,0.,-0.0600000000000001));
#67275=CARTESIAN_POINT('Ctrl Pts',(-0.676756940578634,1.65846773778668E-7,
-0.139182021618995));
#67276=CARTESIAN_POINT('Ctrl Pts',(-0.67675546928947,-0.112031032267847,
-0.133910832316977));
#67277=CARTESIAN_POINT('Ctrl Pts',(-0.619882615330693,-0.336297451995222,
-0.123358938538881));
#67278=CARTESIAN_POINT('Ctrl Pts',(-0.384315741505486,-0.591363827723695,
-0.107526340284706));
#67279=CARTESIAN_POINT('Ctrl Pts',(-0.055404374357266,-0.703098282770509,
-0.091684226856471));
#67280=CARTESIAN_POINT('Ctrl Pts',(0.287037892597339,-0.644247893625522,
-0.0758421134282355));
#67281=CARTESIAN_POINT('Ctrl Pts',(0.468762250669717,-0.500787277377127,
-0.0652807044760785));
#67282=CARTESIAN_POINT('Ctrl Pts',(0.5370608629359,-0.411689834101531,-0.0600000000000001));
#67283=CARTESIAN_POINT('Origin',(0.,0.,-3.278617978381));
#67284=CARTESIAN_POINT('',(-0.676682724618054,-1.68358750310745E-5,-0.378617978381002));
#67285=CARTESIAN_POINT('',(-0.676656215749625,1.16614266989223E-5,-0.339182021618995));
#67286=CARTESIAN_POINT('',(-0.6767,-6.21087748740391E-14,-3.278617978381));
#67287=CARTESIAN_POINT('Ctrl Pts',(-0.676682724618054,-1.68358750310751E-5,
-0.378617978381002));
#67288=CARTESIAN_POINT('Ctrl Pts',(-0.676712572580368,-0.031596364138927,
-0.377132602748119));
#67289=CARTESIAN_POINT('Ctrl Pts',(-0.666825032969671,-0.175426703014129,
-0.370366522639158));
#67290=CARTESIAN_POINT('Ctrl Pts',(-0.566672567635157,-0.419879657837779,
-0.358319738054119));
#67291=CARTESIAN_POINT('Ctrl Pts',(-0.297475915280626,-0.639472286942102,
-0.342477624625884));
#67292=CARTESIAN_POINT('Ctrl Pts',(0.043897043275945,-0.703910346247173,
-0.326635511197648));
#67293=CARTESIAN_POINT('Ctrl Pts',(0.374619303032495,-0.597559288958764,
-0.310793397769413));
#67294=CARTESIAN_POINT('Ctrl Pts',(0.614448027167589,-0.346222973859112,
-0.294951284341178));
#67295=CARTESIAN_POINT('Ctrl Pts',(0.70519379538744,-0.0108828985917093,
-0.279109170912942));
#67296=CARTESIAN_POINT('Ctrl Pts',(0.624839043230104,0.327097684121224,
-0.263267057484707));
#67297=CARTESIAN_POINT('Ctrl Pts',(0.392880175048439,0.585714858477159,
-0.247424944056472));
#67298=CARTESIAN_POINT('Ctrl Pts',(0.0655971465397984,0.70222057750431,
-0.231582830628236));
#67299=CARTESIAN_POINT('Ctrl Pts',(-0.277601643923981,0.6483471683419,-0.215740717200002));
#67300=CARTESIAN_POINT('Ctrl Pts',(-0.553446229800004,0.437165882444832,
-0.199898603771766));
#67301=CARTESIAN_POINT('Ctrl Pts',(-0.664020356520139,0.189362139227846,
-0.187524357498766));
#67302=CARTESIAN_POINT('Ctrl Pts',(-0.676693464278589,0.0385585134182499,
-0.180430815701845));
#67303=CARTESIAN_POINT('Ctrl Pts',(-0.676664313283933,1.40419911898067E-5,
-0.178617978381002));
#67304=CARTESIAN_POINT('Ctrl Pts',(-0.676656215749625,1.16614266988981E-5,
-0.339182021618994));
#67305=CARTESIAN_POINT('Ctrl Pts',(-0.676613003901662,-0.0699148884815599,
-0.33589332383933));
#67306=CARTESIAN_POINT('Ctrl Pts',(-0.648510715023198,-0.25215734145285,
-0.327323921583586));
#67307=CARTESIAN_POINT('Ctrl Pts',(-0.487488465654378,-0.509678055216417,
-0.313473814851765));
#67308=CARTESIAN_POINT('Ctrl Pts',(-0.185028133270616,-0.680574251437019,
-0.297631701423529));
#67309=CARTESIAN_POINT('Ctrl Pts',(0.162325390816526,-0.68634334526228,
-0.281789587995294));
#67310=CARTESIAN_POINT('Ctrl Pts',(0.470294081325063,-0.525585589562447,
-0.265947474567059));
#67311=CARTESIAN_POINT('Ctrl Pts',(0.664155702788206,-0.237305484551378,
-0.250105361138824));
#67312=CARTESIAN_POINT('Ctrl Pts',(0.696873939840873,0.108551823732687,
-0.234263247710588));
#67313=CARTESIAN_POINT('Ctrl Pts',(0.560510101409974,0.428071317231208,
-0.218421134282353));
#67314=CARTESIAN_POINT('Ctrl Pts',(0.288150599099951,0.643728235591383,
-0.202579020854118));
#67315=CARTESIAN_POINT('Ctrl Pts',(-0.0541233696112858,0.703198020558049,
-0.186736907425882));
#67316=CARTESIAN_POINT('Ctrl Pts',(-0.383263958328779,0.592051415322255,
-0.170894793997647));
#67317=CARTESIAN_POINT('Ctrl Pts',(-0.61941646401829,0.337256127609639,
-0.155052680569412));
#67318=CARTESIAN_POINT('Ctrl Pts',(-0.676706952231611,0.112638054466167,
-0.144481756443194));
#67319=CARTESIAN_POINT('Ctrl Pts',(-0.6767569432345,0.000202396555859588,
-0.139191536793055));
#67320=CARTESIAN_POINT('Ctrl Pts',(-0.676756940578634,1.65846773778668E-7,
-0.139182021618995));
#67321=CARTESIAN_POINT('Origin',(0.,0.,-3.278617978381));
#67322=CARTESIAN_POINT('',(-0.676744415355718,1.02840190608962E-5,-0.578617978381002));
#67323=CARTESIAN_POINT('',(-0.676694184207546,-1.73693794768559E-5,-0.539182021618994));
#67324=CARTESIAN_POINT('',(-0.6767,-6.21087748740391E-14,-3.278617978381));
#67325=CARTESIAN_POINT('Ctrl Pts',(-0.676744415355718,1.02840190609223E-5,
-0.578617978381002));
#67326=CARTESIAN_POINT('Ctrl Pts',(-0.676669814511743,-0.101663497973202,
-0.573834389794394));
#67327=CARTESIAN_POINT('Ctrl Pts',(-0.62778641803666,-0.315646428609378,
-0.563770096731707));
#67328=CARTESIAN_POINT('Ctrl Pts',(-0.411086852200351,-0.573083175383003,
-0.548425099192943));
#67329=CARTESIAN_POINT('Ctrl Pts',(-0.0876254735054571,-0.699813191038862,
-0.532582985764706));
#67330=CARTESIAN_POINT('Ctrl Pts',(0.257096392819387,-0.656748179105437,
-0.516740872336472));
#67331=CARTESIAN_POINT('Ctrl Pts',(0.539439199031029,-0.454336963616046,
-0.500898758908236));
#67332=CARTESIAN_POINT('Ctrl Pts',(0.690898371074035,-0.141690390662916,
-0.485056645480001));
#67333=CARTESIAN_POINT('Ctrl Pts',(0.67472551005466,0.205334390789043,-0.469214532051766));
#67334=CARTESIAN_POINT('Ctrl Pts',(0.494844622289992,0.502539078828164,
-0.45337241862353));
#67335=CARTESIAN_POINT('Ctrl Pts',(0.194900041286442,0.67781317475087,-0.437530305195295));
#67336=CARTESIAN_POINT('Ctrl Pts',(-0.152332956558304,0.688630086697795,
-0.42168819176706));
#67337=CARTESIAN_POINT('Ctrl Pts',(-0.462605549975718,0.532365317323737,
-0.405846078338825));
#67338=CARTESIAN_POINT('Ctrl Pts',(-0.642068958012134,0.273695698164427,
-0.391489340543472));
#67339=CARTESIAN_POINT('Ctrl Pts',(-0.676606459173965,0.080672985488116,
-0.382413307224198));
#67340=CARTESIAN_POINT('Ctrl Pts',(-0.676682724618054,-1.68358750310751E-5,
-0.378617978381002));
#67341=CARTESIAN_POINT('Ctrl Pts',(-0.676694184207546,-1.73693794768663E-5,
-0.539182021618994));
#67342=CARTESIAN_POINT('Ctrl Pts',(-0.676722072506792,-0.0277863514175533,
-0.537875815361682));
#67343=CARTESIAN_POINT('Ctrl Pts',(-0.668264186930468,-0.167802341299913,
-0.531288904628292));
#67344=CARTESIAN_POINT('Ctrl Pts',(-0.573681658522724,-0.410251236866699,
-0.519421289418823));
#67345=CARTESIAN_POINT('Ctrl Pts',(-0.308231320835643,-0.634358081474877,
-0.503579175990589));
#67346=CARTESIAN_POINT('Ctrl Pts',(0.032004897278945,-0.704551211216498,
-0.487737062562353));
#67347=CARTESIAN_POINT('Ctrl Pts',(0.364475796750062,-0.603799731912975,
-0.471894949134118));
#67348=CARTESIAN_POINT('Ctrl Pts',(0.60851427060865,-0.356548881847406,
-0.456052835705882));
#67349=CARTESIAN_POINT('Ctrl Pts',(0.704909489523639,-0.0227889061948828,
-0.440210722277648));
#67350=CARTESIAN_POINT('Ctrl Pts',(0.630273170690079,0.316500320697992,
-0.424368608849411));
#67351=CARTESIAN_POINT('Ctrl Pts',(0.402714255056845,0.578997367377502,
-0.408526495421177));
#67352=CARTESIAN_POINT('Ctrl Pts',(0.0774451521325488,0.701012818064358,
-0.39268438199294));
#67353=CARTESIAN_POINT('Ctrl Pts',(-0.26661439669049,0.652942176782176,
-0.376842268564707));
#67354=CARTESIAN_POINT('Ctrl Pts',(-0.545985540464761,0.446448778736983,
-0.36100015513647));
#67355=CARTESIAN_POINT('Ctrl Pts',(-0.662389607688161,0.196987006295065,
-0.348446739487901));
#67356=CARTESIAN_POINT('Ctrl Pts',(-0.676682389723724,0.0423670753341918,
-0.341174028315408));
#67357=CARTESIAN_POINT('Ctrl Pts',(-0.676656215749625,1.16614266988981E-5,
-0.339182021618994));
#67358=CARTESIAN_POINT('Origin',(0.,0.,-3.278617978381));
#67359=CARTESIAN_POINT('',(-0.67664350881809,3.14251806171502E-6,-0.778617978381002));
#67360=CARTESIAN_POINT('',(-0.676734930268368,1.31228392115518E-5,-0.739182021618995));
#67361=CARTESIAN_POINT('',(-0.6767,-6.21087748740391E-14,-3.278617978381));
#67362=CARTESIAN_POINT('Ctrl Pts',(-0.67664350881809,3.14251806169882E-6,
-0.778617978381002));
#67363=CARTESIAN_POINT('Ctrl Pts',(-0.676633824259794,-0.0595589089414728,
-0.775816881316747));
#67364=CARTESIAN_POINT('Ctrl Pts',(-0.654163529573119,-0.231416130782925,
-0.767735079776413));
#67365=CARTESIAN_POINT('Ctrl Pts',(-0.510387952556461,-0.48674517341652,
-0.754372573760001));
#67366=CARTESIAN_POINT('Ctrl Pts',(-0.216097768239373,-0.671355703424805,
-0.738530460331765));
#67367=CARTESIAN_POINT('Ctrl Pts',(0.13062401781091,-0.693075819755666,
-0.722688346903532));
#67368=CARTESIAN_POINT('Ctrl Pts',(0.445652619177005,-0.546635590663221,
-0.706846233475294));
#67369=CARTESIAN_POINT('Ctrl Pts',(0.652552937542223,-0.267565673553371,
-0.69100412004706));
#67370=CARTESIAN_POINT('Ctrl Pts',(0.701124939933614,0.0764234555757611,
-0.675162006618824));
#67371=CARTESIAN_POINT('Ctrl Pts',(0.579583646314047,0.401870032329318,
-0.659319893190589));
#67372=CARTESIAN_POINT('Ctrl Pts',(0.317418508393823,0.629811254653404,
-0.643477779762354));
#67373=CARTESIAN_POINT('Ctrl Pts',(-0.0217615887758392,0.704941954499094,
-0.627635666334118));
#67374=CARTESIAN_POINT('Ctrl Pts',(-0.355661691778637,0.609033239618506,
-0.611793552905885));
#67375=CARTESIAN_POINT('Ctrl Pts',(-0.603267927301802,0.365355352838904,
-0.595951439477647));
#67376=CARTESIAN_POINT('Ctrl Pts',(-0.673935245528764,0.133378091047515,
-0.584892914636021));
#67377=CARTESIAN_POINT('Ctrl Pts',(-0.676752167959069,0.0105763374443912,
-0.579115094270472));
#67378=CARTESIAN_POINT('Ctrl Pts',(-0.676744415355718,1.02840190609223E-5,
-0.578617978381002));
#67379=CARTESIAN_POINT('Ctrl Pts',(-0.676734930268368,1.31228392115622E-5,
-0.739182021618995));
#67380=CARTESIAN_POINT('Ctrl Pts',(-0.676648595874367,-0.0978564382041463,
-0.734577602407957));
#67381=CARTESIAN_POINT('Ctrl Pts',(-0.630547679361052,-0.30804907633827,
-0.724692478720841));
#67382=CARTESIAN_POINT('Ctrl Pts',(-0.420705045567162,-0.56606005627552,
-0.709526650557648));
#67383=CARTESIAN_POINT('Ctrl Pts',(-0.0994296853315642,-0.69823381495827,
-0.693684537129411));
#67384=CARTESIAN_POINT('Ctrl Pts',(0.245970207536815,-0.660995748610087,
-0.677842423701176));
#67385=CARTESIAN_POINT('Ctrl Pts',(0.531690576341267,-0.46338089484376,
-0.662000310272941));
#67386=CARTESIAN_POINT('Ctrl Pts',(0.688407352137116,-0.153336362940691,
-0.646158196844705));
#67387=CARTESIAN_POINT('Ctrl Pts',(0.678096488492109,0.193912028948647,
-0.630316083416472));
#67388=CARTESIAN_POINT('Ctrl Pts',(0.503259700720423,0.494111724518966,
-0.614473969988234));
#67389=CARTESIAN_POINT('Ctrl Pts',(0.206317477008665,0.674425549158015,
-0.598631856560001));
#67390=CARTESIAN_POINT('Ctrl Pts',(-0.140683365416483,0.691104126287348,
-0.582789743131764));
#67391=CARTESIAN_POINT('Ctrl Pts',(-0.453550332947481,0.540100748156837,
-0.56694762970353));
#67392=CARTESIAN_POINT('Ctrl Pts',(-0.639649782541237,0.281308470484841,
-0.552411722532606));
#67393=CARTESIAN_POINT('Ctrl Pts',(-0.67660932624958,0.0844775325776096,
-0.543156519837761));
#67394=CARTESIAN_POINT('Ctrl Pts',(-0.676694184207546,-1.73693794768663E-5,
-0.539182021618994));
#67395=CARTESIAN_POINT('Origin',(0.,0.,-3.278617978381));
#67396=CARTESIAN_POINT('',(-0.676726354840372,-1.49018706585343E-5,-0.978617978381004));
#67397=CARTESIAN_POINT('',(-0.676642658803801,-3.62091512329243E-7,-0.939182021618995));
#67398=CARTESIAN_POINT('',(-0.6767,-6.21087748740391E-14,-3.278617978381));
#67399=CARTESIAN_POINT('Ctrl Pts',(-0.676726354840372,-1.49018706585916E-5,
-0.978617978381004));
#67400=CARTESIAN_POINT('Ctrl Pts',(-0.676743078776964,-0.0174154680940201,
-0.977799372839101));
#67401=CARTESIAN_POINT('Ctrl Pts',(-0.6718429949253,-0.14705514285169,-0.97170006282112));
#67402=CARTESIAN_POINT('Ctrl Pts',(-0.591922568453257,-0.383463686565954,
-0.960320048327059));
#67403=CARTESIAN_POINT('Ctrl Pts',(-0.337047750540382,-0.619528481843024,
-0.944477934898826));
#67404=CARTESIAN_POINT('Ctrl Pts',(-0.000395348502580347,-0.705277654302627,
-0.928635821470588));
#67405=CARTESIAN_POINT('Ctrl Pts',(0.336352976576915,-0.619905961502954,
-0.912793708042355));
#67406=CARTESIAN_POINT('Ctrl Pts',(0.59149228989595,-0.384127058344892,
-0.896951594614118));
#67407=CARTESIAN_POINT('Ctrl Pts',(0.703118375731167,-0.0551477621324492,
-0.881109481185884));
#67408=CARTESIAN_POINT('Ctrl Pts',(0.644147500070733,0.287211984624038,
-0.865267367757648));
#67409=CARTESIAN_POINT('Ctrl Pts',(0.428887711959651,0.559885753068489,
-0.849425254329413));
#67410=CARTESIAN_POINT('Ctrl Pts',(0.109567294787274,0.696714958840452,
-0.833583140901177));
#67411=CARTESIAN_POINT('Ctrl Pts',(-0.236337333828263,0.664500858237221,
-0.817741027472942));
#67412=CARTESIAN_POINT('Ctrl Pts',(-0.524899653622529,0.471059528707363,
-0.801898914044707));
#67413=CARTESIAN_POINT('Ctrl Pts',(-0.657602612550172,0.217736950995035,
-0.788857897680726));
#67414=CARTESIAN_POINT('Ctrl Pts',(-0.676652081852862,0.0527290926991997,
-0.781097585792825));
#67415=CARTESIAN_POINT('Ctrl Pts',(-0.67664350881809,3.14251806169882E-6,
-0.778617978381002));
#67416=CARTESIAN_POINT('Ctrl Pts',(-0.676642658803801,-3.62091512332713E-7,
-0.939182021618995));
#67417=CARTESIAN_POINT('Ctrl Pts',(-0.676643701727751,-0.0557527860905397,
-0.93656009393031));
#67418=CARTESIAN_POINT('Ctrl Pts',(-0.656108130744977,-0.223792859010719,
-0.928657461765547));
#67419=CARTESIAN_POINT('Ctrl Pts',(-0.518534126716599,-0.478057613794162,
-0.915474125124705));
#67420=CARTESIAN_POINT('Ctrl Pts',(-0.22740314400511,-0.66761106399827,
-0.89963201169647));
#67421=CARTESIAN_POINT('Ctrl Pts',(0.118902453310195,-0.695182658927227,
-0.883789898268235));
#67422=CARTESIAN_POINT('Ctrl Pts',(0.436358858299948,-0.55408272799238,
-0.86794778484));
#67423=CARTESIAN_POINT('Ctrl Pts',(0.647941916898673,-0.278546216994571,
-0.852105671411764));
#67424=CARTESIAN_POINT('Ctrl Pts',(0.702315427199591,0.0645737051265365,
-0.836263557983531));
#67425=CARTESIAN_POINT('Ctrl Pts',(0.586286794664772,0.392026168868892,
-0.820421444555292));
#67426=CARTESIAN_POINT('Ctrl Pts',(0.328007939141782,0.624361685672875,
-0.804579331127061));
#67427=CARTESIAN_POINT('Ctrl Pts',(-0.00985517942347469,0.705208903882278,
-0.788737217698822));
#67428=CARTESIAN_POINT('Ctrl Pts',(-0.345327144915973,0.614951937683339,
-0.772895104270589));
#67429=CARTESIAN_POINT('Ctrl Pts',(-0.597012704480207,0.375489751345548,
-0.757052990842353));
#67430=CARTESIAN_POINT('Ctrl Pts',(-0.672795249619501,0.141000208336555,
-0.745815296625156));
#67431=CARTESIAN_POINT('Ctrl Pts',(-0.676747610842367,0.0143879525399922,
-0.739858306884036));
#67432=CARTESIAN_POINT('Ctrl Pts',(-0.676734930268368,1.31228392115622E-5,
-0.739182021618995));
#67433=CARTESIAN_POINT('Origin',(0.,0.,-3.278617978381));
#67434=CARTESIAN_POINT('',(-0.676703646557406,1.72471476807506E-5,-1.178617978381));
#67435=CARTESIAN_POINT('',(-0.676737017697599,-1.25909068602881E-5,-1.139182021619));
#67436=CARTESIAN_POINT('',(-0.6767,-6.21087748740391E-14,-3.278617978381));
#67437=CARTESIAN_POINT('Ctrl Pts',(-0.676703646557406,1.72471476807406E-5,
-1.178617978381));
#67438=CARTESIAN_POINT('Ctrl Pts',(-0.676613962442266,-0.087499758462613,
-1.17450115988537));
#67439=CARTESIAN_POINT('Ctrl Pts',(-0.637674973361225,-0.287353613941579,
-1.16510363691367));
#67440=CARTESIAN_POINT('Ctrl Pts',(-0.446265180001859,-0.546135619674237,
-1.15042540946588));
#67441=CARTESIAN_POINT('Ctrl Pts',(-0.13140095282778,-0.692928939758619,
-1.13458329603765));
#67442=CARTESIAN_POINT('Ctrl Pts',(0.215344966055381,-0.671597551777596,
-1.11874118260941));
#67443=CARTESIAN_POINT('Ctrl Pts',(0.509841934903309,-0.487317070676889,
-1.10289906918118));
#67444=CARTESIAN_POINT('Ctrl Pts',(0.680636426416433,-0.184799299225192,
-1.08705695575294));
#67445=CARTESIAN_POINT('Ctrl Pts',(0.686288731012368,0.162556155357116,
-1.07121484232471));
#67446=CARTESIAN_POINT('Ctrl Pts',(0.52542743525236,0.470470760242527,-1.05537272889647));
#67447=CARTESIAN_POINT('Ctrl Pts',(0.237082166616096,0.664235479503821,
-1.03953061546824));
#67448=CARTESIAN_POINT('Ctrl Pts',(-0.108786128932179,0.696837358435242,
-1.02368850204));
#67449=CARTESIAN_POINT('Ctrl Pts',(-0.428259746586556,0.560366233290937,
-1.00784638861177));
#67450=CARTESIAN_POINT('Ctrl Pts',(-0.632686243670446,0.302011290964289,
-0.992822880725432));
#67451=CARTESIAN_POINT('Ctrl Pts',(-0.676635195111024,0.0948330365135053,
-0.983080077315179));
#67452=CARTESIAN_POINT('Ctrl Pts',(-0.676726354840372,-1.49018706585916E-5,
-0.978617978381004));
#67453=CARTESIAN_POINT('Ctrl Pts',(-0.6767370176976,-1.25909068602707E-5,
-1.139182021619));
#67454=CARTESIAN_POINT('Ctrl Pts',(-0.676748654703403,-0.0136040506252591,
-1.13854258545266));
#67455=CARTESIAN_POINT('Ctrl Pts',(-0.673035053480589,-0.139432545494104,
-1.13262244481025));
#67456=CARTESIAN_POINT('Ctrl Pts',(-0.598313157002194,-0.373414098333714,
-1.12142159969176));
#67457=CARTESIAN_POINT('Ctrl Pts',(-0.347460752777172,-0.613748929087322,
-1.10557948626353));
#67458=CARTESIAN_POINT('Ctrl Pts',(-0.0123042673209635,-0.705170424565585,
-1.08973737283529));
#67459=CARTESIAN_POINT('Ctrl Pts',(0.32583759114047,-0.625497071836542,
-1.07389525940706));
#67460=CARTESIAN_POINT('Ctrl Pts',(0.584921776088787,-0.394059942817653,
-1.05805314597882));
#67461=CARTESIAN_POINT('Ctrl Pts',(0.702086931244113,-0.0670124141673551,
-1.04221103255059));
#67462=CARTESIAN_POINT('Ctrl Pts',(0.648905383326142,0.276294274581765,
-1.02636891912235));
#67463=CARTESIAN_POINT('Ctrl Pts',(0.438280522141762,0.552563938913369,
-1.01052680569412));
#67464=CARTESIAN_POINT('Ctrl Pts',(0.121316063044922,0.694765525572184,
-0.994684692265882));
#67465=CARTESIAN_POINT('Ctrl Pts',(-0.225083200276113,0.668396795047505,
-0.978842578837647));
#67466=CARTESIAN_POINT('Ctrl Pts',(-0.51687073479559,0.479855568049576,
-0.963000465409411));
#67467=CARTESIAN_POINT('Ctrl Pts',(-0.655713957784839,0.225360770249037,
-0.949780279669861));
#67468=CARTESIAN_POINT('Ctrl Pts',(-0.676641601222389,0.0565356176798869,
-0.941840798406389));
#67469=CARTESIAN_POINT('Ctrl Pts',(-0.676642658803801,-3.62091512332713E-7,
-0.939182021618995));
#67470=CARTESIAN_POINT('Origin',(0.,0.,-3.278617978381));
#67471=CARTESIAN_POINT('',(-0.676651018322484,-9.42764808053333E-6,-1.378617978381));
#67472=CARTESIAN_POINT('',(-0.676691774264851,1.73213003940714E-5,-1.339182021619));
#67473=CARTESIAN_POINT('',(-0.6767,-6.21087748740391E-14,-3.278617978381));
#67474=CARTESIAN_POINT('Ctrl Pts',(-0.676651018322484,-9.42764808054344E-6,
-1.378617978381));
#67475=CARTESIAN_POINT('Ctrl Pts',(-0.67667346476596,-0.045391951814263,
-1.37648365140773));
#67476=CARTESIAN_POINT('Ctrl Pts',(-0.661045351089367,-0.203043660447462,
-1.36906861995837));
#67477=CARTESIAN_POINT('Ctrl Pts',(-0.539948223619144,-0.453731905170425,
-1.35637288403294));
#67478=CARTESIAN_POINT('Ctrl Pts',(-0.257832520922968,-0.65645953196946,
-1.34053077060471));
#67479=CARTESIAN_POINT('Ctrl Pts',(0.0868408479677307,-0.699910989400294,
-1.32468865717647));
#67480=CARTESIAN_POINT('Ctrl Pts',(0.4104441021973,-0.57354369051582,-1.30884654374824));
#67481=CARTESIAN_POINT('Ctrl Pts',(0.634461683351754,-0.308018016222288,
-1.29300443032));
#67482=CARTESIAN_POINT('Ctrl Pts',(0.70454041281189,0.0322417845955294,
-1.27716231689176));
#67483=CARTESIAN_POINT('Ctrl Pts',(0.603677153234099,0.364678791023317,
-1.26132020346353));
#67484=CARTESIAN_POINT('Ctrl Pts',(0.356344264045233,0.608634119517723,
-1.2454780900353));
#67485=CARTESIAN_POINT('Ctrl Pts',(0.022551895498706,0.7049171142542,-1.22963597660706));
#67486=CARTESIAN_POINT('Ctrl Pts',(-0.316712218604248,0.630166721230049,
-1.21379386317883));
#67487=CARTESIAN_POINT('Ctrl Pts',(-0.579132739896463,0.402519559200629,
-1.19795174975059));
#67488=CARTESIAN_POINT('Ctrl Pts',(-0.669359637244422,0.16174631842112,
-1.18622645481798));
#67489=CARTESIAN_POINT('Ctrl Pts',(-0.676729001594164,0.024759609724268,
-1.17978186436145));
#67490=CARTESIAN_POINT('Ctrl Pts',(-0.676703646557406,1.72471476807406E-5,
-1.178617978381));
#67491=CARTESIAN_POINT('Ctrl Pts',(-0.676691774264851,1.73213003940645E-5,
-1.339182021619));
#67492=CARTESIAN_POINT('Ctrl Pts',(-0.676608477074042,-0.0836950532711893,
-1.33524437249894));
#67493=CARTESIAN_POINT('Ctrl Pts',(-0.640153403921032,-0.279742992602309,
-1.3260260189028));
#67494=CARTESIAN_POINT('Ctrl Pts',(-0.455423334553543,-0.538522338460017,
-1.31152696083059));
#67495=CARTESIAN_POINT('Ctrl Pts',(-0.143082679303674,-0.690611373754874,
-1.29568484740235));
#67496=CARTESIAN_POINT('Ctrl Pts',(0.203973994150782,-0.675138009881304,
-1.27984273397412));
#67497=CARTESIAN_POINT('Ctrl Pts',(0.501540645971156,-0.495856534811379,
-1.26400062054588));
#67498=CARTESIAN_POINT('Ctrl Pts',(0.677418954516088,-0.196265847101944,
-1.24815850711765));
#67499=CARTESIAN_POINT('Ctrl Pts',(0.688935728376574,0.150944641649023,
-1.23231639368941));
#67500=CARTESIAN_POINT('Ctrl Pts',(0.533296663357694,0.461531571539655,
-1.21647428026118));
#67501=CARTESIAN_POINT('Ctrl Pts',(0.248264321922183,0.660137522897185,
-1.20063216683294));
#67502=CARTESIAN_POINT('Ctrl Pts',(-0.0970041624297474,0.698574917347893,
-1.1847900534047));
#67503=CARTESIAN_POINT('Ctrl Pts',(-0.418736616528254,0.567517725410213,
-1.16894793997647));
#67504=CARTESIAN_POINT('Ctrl Pts',(-0.629986079414507,0.30961194562541,
-1.15374526271457));
#67505=CARTESIAN_POINT('Ctrl Pts',(-0.676652551930573,0.0986393380825266,
-1.14382328992874));
#67506=CARTESIAN_POINT('Ctrl Pts',(-0.6767370176976,-1.25909068602707E-5,
-1.139182021619));
#67507=CARTESIAN_POINT('Origin',(0.,0.,-3.278617978381));
#67508=CARTESIAN_POINT('',(-0.676756207239106,-3.37313647904859E-6,-1.578617978381));
#67509=CARTESIAN_POINT('',(-0.676657745381425,-1.21934319496919E-5,-1.539182021619));
#67510=CARTESIAN_POINT('',(-0.6767,-6.21087748740391E-14,-3.278617978381));
#67511=CARTESIAN_POINT('Ctrl Pts',(-0.676756207239105,-3.37313647901958E-6,
-1.578617978381));
#67512=CARTESIAN_POINT('Ctrl Pts',(-0.676757103819284,-0.00323042804578434,
-1.57846614293008));
#67513=CARTESIAN_POINT('Ctrl Pts',(-0.675948430935335,-0.118691185533526,
-1.57303360300308));
#67514=CARTESIAN_POINT('Ctrl Pts',(-0.614835796701285,-0.345533889877317,
-1.5623203586));
#67515=CARTESIAN_POINT('Ctrl Pts',(-0.375288999670649,-0.597138922433682,
-1.54647824517177));
#67516=CARTESIAN_POINT('Ctrl Pts',(-0.0446861795912879,-0.703860690273713,
-1.53063613174353));
#67517=CARTESIAN_POINT('Ctrl Pts',(0.296758806931518,-0.639805389526875,
-1.5147940183153));
#67518=CARTESIAN_POINT('Ctrl Pts',(0.566201478471519,-0.420514698596517,
-1.49895190488706));
#67519=CARTESIAN_POINT('Ctrl Pts',(0.698267208723158,-0.0991949150966095,
-1.48310979145883));
#67520=CARTESIAN_POINT('Ctrl Pts',(0.660913011645563,0.246192438951009,
-1.46726767803059));
#67521=CARTESIAN_POINT('Ctrl Pts',(0.46320210154304,0.53184634913212,-1.45142556460235));
#67522=CARTESIAN_POINT('Ctrl Pts',(0.153104893757042,0.688458871296389,
-1.43558345117412));
#67523=CARTESIAN_POINT('Ctrl Pts',(-0.194140012861185,0.678031253973823,
-1.41974133774588));
#67524=CARTESIAN_POINT('Ctrl Pts',(-0.494280907634458,0.503093540315427,
-1.40389922431765));
#67525=CARTESIAN_POINT('Ctrl Pts',(-0.650215574940587,0.246104379942304,
-1.39019143786269));
#67526=CARTESIAN_POINT('Ctrl Pts',(-0.676617928273182,0.0668924832797416,
-1.38176435588381));
#67527=CARTESIAN_POINT('Ctrl Pts',(-0.676651018322484,-9.42764808054344E-6,
-1.378617978381));
#67528=CARTESIAN_POINT('Ctrl Pts',(-0.676657745381425,-1.21934319497544E-5,
-1.539182021619));
#67529=CARTESIAN_POINT('Ctrl Pts',(-0.676684688084094,-0.0415838273109365,
-1.53722686402129));
#67530=CARTESIAN_POINT('Ctrl Pts',(-0.662730591069265,-0.195418828189768,
-1.52999100194751));
#67531=CARTESIAN_POINT('Ctrl Pts',(-0.54753273728204,-0.444549912024228,
-1.51747443539765));
#67532=CARTESIAN_POINT('Ctrl Pts',(-0.268880416908177,-0.652012303625934,
-1.50163232196941));
#67533=CARTESIAN_POINT('Ctrl Pts',(0.0750101104497115,-0.701277552761128,
-1.48579020854118));
#67534=CARTESIAN_POINT('Ctrl Pts',(0.400701004053372,-0.580392477576107,
-1.46994809511294));
#67535=CARTESIAN_POINT('Ctrl Pts',(0.629170183477428,-0.318687312109054,
-1.45410598168471));
#67536=CARTESIAN_POINT('Ctrl Pts',(0.70498438292987,0.0203406612799057,
-1.43826386825647));
#67537=CARTESIAN_POINT('Ctrl Pts',(0.609748873285091,0.354433398826739,
-1.42242175482824));
#67538=CARTESIAN_POINT('Ctrl Pts',(0.366570558206358,0.602530288477345,
-1.4065796414));
#67539=CARTESIAN_POINT('Ctrl Pts',(0.034451567471494,0.704435811252572,
-1.39073752797176));
#67540=CARTESIAN_POINT('Ctrl Pts',(-0.306026375229727,0.63542472436951,
-1.37489541454353));
#67541=CARTESIAN_POINT('Ctrl Pts',(-0.57225342141949,0.412241124040289,
-1.35905330111529));
#67542=CARTESIAN_POINT('Ctrl Pts',(-0.667973682251133,0.169370387447164,
-1.34714883680712));
#67543=CARTESIAN_POINT('Ctrl Pts',(-0.676720185312876,0.0285699804139074,
-1.34052507697502));
#67544=CARTESIAN_POINT('Ctrl Pts',(-0.676691774264851,1.73213003940645E-5,
-1.339182021619));
#67545=CARTESIAN_POINT('Origin',(0.,0.,-3.278617978381));
#67546=CARTESIAN_POINT('',(-0.676663433474933,1.38299030018566E-5,-1.778617978381));
#67547=CARTESIAN_POINT('',(-0.676757588646615,6.12124814511891E-7,-1.739182021619));
#67548=CARTESIAN_POINT('',(-0.6767,-6.21087748740391E-14,-3.278617978381));
#67549=CARTESIAN_POINT('Ctrl Pts',(-0.676663433474933,1.38299030018468E-5,
-1.778617978381));
#67550=CARTESIAN_POINT('Ctrl Pts',(-0.67660888674756,-0.0733412266291114,
-1.77516792997636));
#67551=CARTESIAN_POINT('Ctrl Pts',(-0.646522617464707,-0.259018482991803,
-1.76643717709563));
#67552=CARTESIAN_POINT('Ctrl Pts',(-0.479681756700353,-0.517032047602386,
-1.75242571973882));
#67553=CARTESIAN_POINT('Ctrl Pts',(-0.174657691759948,-0.683309166240393,
-1.73658360631059));
#67554=CARTESIAN_POINT('Ctrl Pts',(0.172743407467333,-0.683795613568578,
-1.72074149288235));
#67555=CARTESIAN_POINT('Ctrl Pts',(0.478231933435968,-0.518373363321409,
-1.70489937945412));
#67556=CARTESIAN_POINT('Ctrl Pts',(0.667687487503493,-0.227178663149353,
-1.68905726602588));
#67557=CARTESIAN_POINT('Ctrl Pts',(0.695142643731443,0.119136186044015,
-1.67321515259765));
#67558=CARTESIAN_POINT('Ctrl Pts',(0.553935982945549,0.436545132554703,
-1.65737303916941));
#67559=CARTESIAN_POINT('Ctrl Pts',(0.278328346711741,0.648035537124133,
-1.64153092574118));
#67560=CARTESIAN_POINT('Ctrl Pts',(-0.0648098389800511,0.702293678406998,
-1.62568881231294));
#67561=CARTESIAN_POINT('Ctrl Pts',(-0.392223273354511,0.58615495374357,
-1.60984669888471));
#67562=CARTESIAN_POINT('Ctrl Pts',(-0.622245998352018,0.330274163232033,
-1.59415642090739));
#67563=CARTESIAN_POINT('Ctrl Pts',(-0.676725921543111,0.109003725444774,
-1.58374684740616));
#67564=CARTESIAN_POINT('Ctrl Pts',(-0.676756207239105,-3.37313647901958E-6,
-1.578617978381));
#67565=CARTESIAN_POINT('Ctrl Pts',(-0.676757566361161,6.11887936561055E-7,
-1.739182021619));
#67566=CARTESIAN_POINT('Ctrl Pts',(-0.676751570191694,-0.11165194125938,
-1.73392865106757));
#67567=CARTESIAN_POINT('Ctrl Pts',(-0.620176730411514,-0.335543843334032,
-1.72339457604006));
#67568=CARTESIAN_POINT('Ctrl Pts',(-0.385318490507109,-0.590716838721934,
-1.70757979653647));
#67569=CARTESIAN_POINT('Ctrl Pts',(-0.0565648575352245,-0.70300578914283,
-1.69173768310824));
#67570=CARTESIAN_POINT('Ctrl Pts',(0.285913054528226,-0.644725094847914,
-1.67589556968));
#67571=CARTESIAN_POINT('Ctrl Pts',(0.559020146487969,-0.430015346815531,
-1.66005345625177));
#67572=CARTESIAN_POINT('Ctrl Pts',(0.696492697099633,-0.110971372719233,
-1.64421134282353));
#67573=CARTESIAN_POINT('Ctrl Pts',(0.664975868496808,0.234997482950838,
-1.6283692293953));
#67574=CARTESIAN_POINT('Ctrl Pts',(0.472116559667202,0.523949116579385,
-1.61252711596706));
#67575=CARTESIAN_POINT('Ctrl Pts',(0.164708046420555,0.685775460424648,
-1.59668500253882));
#67576=CARTESIAN_POINT('Ctrl Pts',(-0.182663427862365,0.681212738282163,
-1.58084288911059));
#67577=CARTESIAN_POINT('Ctrl Pts',(-0.4857154435089,0.51136799920729,-1.56500077568235));
#67578=CARTESIAN_POINT('Ctrl Pts',(-0.648061864522484,0.253724400305278,
-1.55111381985182));
#67579=CARTESIAN_POINT('Ctrl Pts',(-0.676611918272213,0.07069740943459,
-1.54250756849737));
#67580=CARTESIAN_POINT('Ctrl Pts',(-0.676657745381425,-1.21934319497544E-5,
-1.539182021619));
#67581=CARTESIAN_POINT('Origin',(0.,0.,-3.278617978381));
#67582=CARTESIAN_POINT('',(-0.67668383139274,-1.69222484240121E-5,-1.978617978381));
#67583=CARTESIAN_POINT('',(-0.676655502517796,1.13969305124695E-5,-1.939182021619));
#67584=CARTESIAN_POINT('',(-0.6767,-6.21087748740391E-14,-3.278617978381));
#67585=CARTESIAN_POINT('Ctrl Pts',(-0.67668383139274,-1.69222484240131E-5,
-1.978617978381));
#67586=CARTESIAN_POINT('Ctrl Pts',(-0.676713552715602,-0.0312174719885095,
-1.97715042149871));
#67587=CARTESIAN_POINT('Ctrl Pts',(-0.66697116919625,-0.174668430854932,
-1.97040216014034));
#67588=CARTESIAN_POINT('Ctrl Pts',(-0.567376904718818,-0.418927408927545,
-1.95837319430588));
#67589=CARTESIAN_POINT('Ctrl Pts',(-0.298549410801028,-0.638971811013141,
-1.94253108087765));
#67590=CARTESIAN_POINT('Ctrl Pts',(0.0427148506610781,-0.703983073299391,
-1.92668896744941));
#67591=CARTESIAN_POINT('Ctrl Pts',(0.373615247395648,-0.598187573318388,
-1.91084685402117));
#67592=CARTESIAN_POINT('Ctrl Pts',(0.613865722048657,-0.347254375426338,
-1.89500474059294));
#67593=CARTESIAN_POINT('Ctrl Pts',(0.705174524058082,-0.0120671694489478,
-1.87916262716471));
#67594=CARTESIAN_POINT('Ctrl Pts',(0.625387483204131,0.326047882696172,
-1.86332051373647));
#67595=CARTESIAN_POINT('Ctrl Pts',(0.393863255448903,0.585054238482422,
-1.84747840030823));
#67596=CARTESIAN_POINT('Ctrl Pts',(0.0667763501367175,0.702109425247569,
-1.83163628688));
#67597=CARTESIAN_POINT('Ctrl Pts',(-0.276512439276773,0.648812451240159,
-1.81579417345177));
#67598=CARTESIAN_POINT('Ctrl Pts',(-0.552711271174482,0.438094711992443,
-1.79995206002353));
#67599=CARTESIAN_POINT('Ctrl Pts',(-0.663861249737369,0.190120444840065,
-1.78755999499994));
#67600=CARTESIAN_POINT('Ctrl Pts',(-0.676692376923236,0.0389373068692174,
-1.78044863445243));
#67601=CARTESIAN_POINT('Ctrl Pts',(-0.676663433474933,1.38299030018468E-5,
-1.778617978381));
#67602=CARTESIAN_POINT('Ctrl Pts',(-0.676655502517796,1.13969305124799E-5,
-1.939182021619));
#67603=CARTESIAN_POINT('Ctrl Pts',(-0.67661355821236,-0.0695364884621566,
-1.93591114258992));
#67604=CARTESIAN_POINT('Ctrl Pts',(-0.648726662967375,-0.251399550700432,
-1.92735955908476));
#67605=CARTESIAN_POINT('Ctrl Pts',(-0.488343718173467,-0.50885865974436,
-1.91352727110353));
#67606=CARTESIAN_POINT('Ctrl Pts',(-0.186170816147377,-0.680262559524874,
-1.8976851576753));
#67607=CARTESIAN_POINT('Ctrl Pts',(0.161172538892235,-0.686614983366474,
-1.88184304424706));
#67608=CARTESIAN_POINT('Ctrl Pts',(0.469410749818722,-0.526374648545063,
-1.86600093081882));
#67609=CARTESIAN_POINT('Ctrl Pts',(0.663756264470278,-0.238420519361853,
-1.85015881739059));
#67610=CARTESIAN_POINT('Ctrl Pts',(0.697055210292531,0.107381360022812,
-1.83431670396235));
#67611=CARTESIAN_POINT('Ctrl Pts',(0.561228294844321,0.427129399295399,
-1.81847459053412));
#67612=CARTESIAN_POINT('Ctrl Pts',(0.289231077053685,0.643243427282921,
-1.80263247710588));
#67613=CARTESIAN_POINT('Ctrl Pts',(-0.0529420095786137,0.703287897164517,
-1.78679036367765));
#67614=CARTESIAN_POINT('Ctrl Pts',(-0.382269825369864,0.592694274721806,
-1.77094825024941));
#67615=CARTESIAN_POINT('Ctrl Pts',(-0.618847866826519,0.338295788328172,
-1.75510613682118));
#67616=CARTESIAN_POINT('Ctrl Pts',(-0.676615359036302,0.113395975047391,
-1.74451739394437));
#67617=CARTESIAN_POINT('Ctrl Pts',(-0.676757597559959,0.000581553674673004,
-1.73920935554364));
#67618=CARTESIAN_POINT('Ctrl Pts',(-0.676757566361161,6.11887936561055E-7,
-1.739182021619));
#67619=CARTESIAN_POINT('Origin',(0.,0.,-3.278617978381));
#67620=CARTESIAN_POINT('',(-0.676743554268804,1.05936162663817E-5,-2.178617978381));
#67621=CARTESIAN_POINT('',(-0.676695356965443,-1.73809590335028E-5,-2.139182021619));
#67622=CARTESIAN_POINT('',(-0.6767,-6.21087748740391E-14,-3.278617978381));
#67623=CARTESIAN_POINT('Ctrl Pts',(-0.676743554268804,1.05936162663918E-5,
-2.178617978381));
#67624=CARTESIAN_POINT('Ctrl Pts',(-0.676667476509358,-0.1012848297298,
-2.17385220854498));
#67625=CARTESIAN_POINT('Ctrl Pts',(-0.628064490957334,-0.314891053553278,
-2.16380573423288));
#67626=CARTESIAN_POINT('Ctrl Pts',(-0.412048695144598,-0.572391997488336,
-2.14847855544471));
#67627=CARTESIAN_POINT('Ctrl Pts',(-0.0888006000396183,-0.699665047999155,
-2.13263644201647));
#67628=CARTESIAN_POINT('Ctrl Pts',(0.255993102559969,-0.657179014729453,
-2.11679432858824));
#67629=CARTESIAN_POINT('Ctrl Pts',(0.538675435341973,-0.455242244654634,
-2.10095221516));
#67630=CARTESIAN_POINT('Ctrl Pts',(0.690659445233286,-0.142850469614568,
-2.08511010173177));
#67631=CARTESIAN_POINT('Ctrl Pts',(0.675069392417806,0.204200982807891,
-2.06926798830353));
#67632=CARTESIAN_POINT('Ctrl Pts',(0.495687876997698,0.501707339548235,
-2.0534258748753));
#67633=CARTESIAN_POINT('Ctrl Pts',(0.196038070227499,0.67748490830463,-2.03758376144706));
#67634=CARTESIAN_POINT('Ctrl Pts',(-0.151176272291756,0.688884940069836,
-2.02174164801882));
#67635=CARTESIAN_POINT('Ctrl Pts',(-0.461710855621964,0.533141455675591,
-2.00589953459059));
#67636=CARTESIAN_POINT('Ctrl Pts',(-0.641831692782511,0.274452916762815,
-1.99152497804465));
#67637=CARTESIAN_POINT('Ctrl Pts',(-0.676606606589992,0.0810513501991045,
-1.98243112597479));
#67638=CARTESIAN_POINT('Ctrl Pts',(-0.67668383139274,-1.69222484240131E-5,
-1.978617978381));
#67639=CARTESIAN_POINT('Ctrl Pts',(-0.676695356965443,-1.73809590334646E-5,
-2.139182021619));
#67640=CARTESIAN_POINT('Ctrl Pts',(-0.676722971761624,-0.0274074129671462,
-2.13789363411227));
#67641=CARTESIAN_POINT('Ctrl Pts',(-0.668403647596514,-0.167044102559928,
-2.13132454212947));
#67642=CARTESIAN_POINT('Ctrl Pts',(-0.574369815989129,-0.409287230630185,
-2.11947474567059));
#67643=CARTESIAN_POINT('Ctrl Pts',(-0.309296212482741,-0.633839550375444,
-2.10363263224235));
#67644=CARTESIAN_POINT('Ctrl Pts',(0.0308216451249593,-0.704603965975287,
-2.08779051881412));
#67645=CARTESIAN_POINT('Ctrl Pts',(0.363461275469507,-0.60441097269192,
-2.07194840538588));
#67646=CARTESIAN_POINT('Ctrl Pts',(0.607914632553942,-0.357570303860817,
-2.05610629195764));
#67647=CARTESIAN_POINT('Ctrl Pts',(0.704870224337332,-0.0239726827650286,
-2.04026417852942));
#67648=CARTESIAN_POINT('Ctrl Pts',(0.630803805217274,0.315441408188147,
-2.02442206510117));
#67649=CARTESIAN_POINT('Ctrl Pts',(0.403686041993089,0.578320241887024,
-2.00857995167294));
#67650=CARTESIAN_POINT('Ctrl Pts',(0.0786223075935471,0.700881769933403,
-1.9927378382447));
#67651=CARTESIAN_POINT('Ctrl Pts',(-0.265517484613883,0.653389002081171,
-1.97689572481647));
#67652=CARTESIAN_POINT('Ctrl Pts',(-0.545235014990942,0.44736506468894,
-1.96105361138823));
#67653=CARTESIAN_POINT('Ctrl Pts',(-0.662223680273716,0.197745313637455,
-1.94848237698908));
#67654=CARTESIAN_POINT('Ctrl Pts',(-0.676681275630061,0.0427458143775428,
-1.941191847066));
#67655=CARTESIAN_POINT('Ctrl Pts',(-0.676655502517796,1.13969305124799E-5,
-1.939182021619));
#67656=CARTESIAN_POINT('Origin',(0.,0.,-3.278617978381));
#67657=CARTESIAN_POINT('',(-0.676643329184379,2.79728545575858E-6,-2.378617978381));
#67658=CARTESIAN_POINT('',(-0.67673389899023,1.33698385852213E-5,-2.339182021619));
#67659=CARTESIAN_POINT('',(-0.6767,-6.21087748740391E-14,-3.278617978381));
#67660=CARTESIAN_POINT('Ctrl Pts',(-0.676643329184379,2.7972854557759E-6,
-2.378617978381));
#67661=CARTESIAN_POINT('Ctrl Pts',(-0.67663476616155,-0.0591804042446534,
-2.37583470006734));
#67662=CARTESIAN_POINT('Ctrl Pts',(-0.654360090959969,-0.230658017222057,
-2.36777071727759));
#67663=CARTESIAN_POINT('Ctrl Pts',(-0.511204661425697,-0.485887353298784,
-2.35442603001177));
#67664=CARTESIAN_POINT('Ctrl Pts',(-0.217224922760744,-0.6709918471119,
-2.33858391658353));
#67665=CARTESIAN_POINT('Ctrl Pts',(0.129459898096913,-0.693294209368428,
-2.32274180315529));
#67666=CARTESIAN_POINT('Ctrl Pts',(0.4447339835604,-0.54738323853179,-2.30689968972706));
#67667=CARTESIAN_POINT('Ctrl Pts',(0.652102673733417,-0.268661178566577,
-2.29105757629882));
#67668=CARTESIAN_POINT('Ctrl Pts',(0.701252295024287,0.0752458947865185,
-2.27521546287059));
#67669=CARTESIAN_POINT('Ctrl Pts',(0.580257720256285,0.400896126249721,
-2.25937334944235));
#67670=CARTESIAN_POINT('Ctrl Pts',(0.318475751250181,0.629277301215201,
-2.24353123601412));
#67671=CARTESIAN_POINT('Ctrl Pts',(-0.0205776948622204,0.70497750633138,
-2.22768912258588));
#67672=CARTESIAN_POINT('Ctrl Pts',(-0.354638393893549,0.609629670813075,
-2.21184700915765));
#67673=CARTESIAN_POINT('Ctrl Pts',(-0.602653507265104,0.366367951846396,
-2.19600489572941));
#67674=CARTESIAN_POINT('Ctrl Pts',(-0.673824797868241,0.134136097894605,
-2.1849285521372));
#67675=CARTESIAN_POINT('Ctrl Pts',(-0.676751774362309,0.0109554197734116,
-2.17913291302106));
#67676=CARTESIAN_POINT('Ctrl Pts',(-0.676743554268804,1.05936162663918E-5,
-2.178617978381));
#67677=CARTESIAN_POINT('Ctrl Pts',(-0.67673389899023,1.33698385852126E-5,
-2.339182021619));
#67678=CARTESIAN_POINT('Ctrl Pts',(-0.676646756100591,-0.0974778733276775,
-2.33459542115855));
#67679=CARTESIAN_POINT('Ctrl Pts',(-0.630818080222992,-0.307293272594146,
-2.32472811622202));
#67680=CARTESIAN_POINT('Ctrl Pts',(-0.42165508048436,-0.565352735712883,
-2.30958010680941));
#67681=CARTESIAN_POINT('Ctrl Pts',(-0.100602142852268,-0.698065850425191,
-2.29373799338118));
#67682=CARTESIAN_POINT('Ctrl Pts',(0.244859799696957,-0.661407893185951,
-2.27789587995294));
#67683=CARTESIAN_POINT('Ctrl Pts',(0.530911635409909,-0.46427315027114,
-2.26205376652471));
#67684=CARTESIAN_POINT('Ctrl Pts',(0.688148871832329,-0.154492242110101,
-2.24621165309647));
#67685=CARTESIAN_POINT('Ctrl Pts',(0.678421183651292,0.192772975931516,
-2.23036953966824));
#67686=CARTESIAN_POINT('Ctrl Pts',(0.50408879085726,0.493265865034647,-2.21452742624));
#67687=CARTESIAN_POINT('Ctrl Pts',(0.207449800749737,0.674078113311214,
-2.19868531281176));
#67688=CARTESIAN_POINT('Ctrl Pts',(-0.13952254273371,0.691339412116387,
-2.18284319938353));
#67689=CARTESIAN_POINT('Ctrl Pts',(-0.45264266065732,0.540861668478527,
-2.1670010859553));
#67690=CARTESIAN_POINT('Ctrl Pts',(-0.639405118876778,0.282065431530378,
-2.15244736003378));
#67691=CARTESIAN_POINT('Ctrl Pts',(-0.676609787197944,0.0848559114366436,
-2.14317433858835));
#67692=CARTESIAN_POINT('Ctrl Pts',(-0.676695356965443,-1.73809590334646E-5,
-2.139182021619));
#67693=CARTESIAN_POINT('Origin',(0.,0.,-3.278617978381));
#67694=CARTESIAN_POINT('',(-0.676727467248305,-1.47039215481353E-5,-2.57861797838101));
#67695=CARTESIAN_POINT('',(-0.676642691248942,-7.12134560654221E-7,-2.539182021619));
#67696=CARTESIAN_POINT('',(-0.6767,-6.21087748740391E-14,-3.278617978381));
#67697=CARTESIAN_POINT('Ctrl Pts',(-0.676727467248305,-1.47039215481135E-5,
-2.57861797838101));
#67698=CARTESIAN_POINT('Ctrl Pts',(-0.676743689334983,-0.0170364276983481,
-2.57781719158969));
#67699=CARTESIAN_POINT('Ctrl Pts',(-0.671964491487141,-0.14629703446376,
-2.5717357003223));
#67700=CARTESIAN_POINT('Ctrl Pts',(-0.592565713804986,-0.382469084713778,
-2.56037350457882));
#67701=CARTESIAN_POINT('Ctrl Pts',(-0.338087697064974,-0.618961578023624,
-2.54453139115059));
#67702=CARTESIAN_POINT('Ctrl Pts',(-0.00157977493823928,-0.705275995805936,
-2.52868927772235));
#67703=CARTESIAN_POINT('Ctrl Pts',(0.335311446522369,-0.62046995075891,
-2.51284716429412));
#67704=CARTESIAN_POINT('Ctrl Pts',(0.590846361696255,-0.385119855146208,
-2.49700505086588));
#67705=CARTESIAN_POINT('Ctrl Pts',(0.703024770348556,-0.0563284851169273,
-2.48116293743765));
#67706=CARTESIAN_POINT('Ctrl Pts',(0.644628928892509,0.286129813186614,
-2.46532082400941));
#67707=CARTESIAN_POINT('Ctrl Pts',(0.429827366355921,0.559164699431498,
-2.44947871058118));
#67708=CARTESIAN_POINT('Ctrl Pts',(0.110737187280514,0.696529971582292,
-2.43363659715294));
#67709=CARTESIAN_POINT('Ctrl Pts',(-0.235221053172144,0.664896820644794,
-2.41779448372471));
#67710=CARTESIAN_POINT('Ctrl Pts',(-0.524107826947175,0.471940368788045,
-2.40195237029647));
#67711=CARTESIAN_POINT('Ctrl Pts',(-0.657417924147744,0.218495181204277,
-2.3888935351819));
#67712=CARTESIAN_POINT('Ctrl Pts',(-0.676651012755633,0.053107682682907,
-2.38111540454342));
#67713=CARTESIAN_POINT('Ctrl Pts',(-0.676643329184379,2.7972854557759E-6,
-2.378617978381));
#67714=CARTESIAN_POINT('Ctrl Pts',(-0.676642691248942,-7.12134560688915E-7,
-2.539182021619));
#67715=CARTESIAN_POINT('Ctrl Pts',(-0.676644728573157,-0.0553742322995621,
-2.5365779126809));
#67716=CARTESIAN_POINT('Ctrl Pts',(-0.656297668877348,-0.22303466957631,
-2.52869309926673));
#67717=CARTESIAN_POINT('Ctrl Pts',(-0.519336234411588,-0.477186125430353,
-2.51552758137647));
#67718=CARTESIAN_POINT('Ctrl Pts',(-0.228523993923267,-0.667228226979231,
-2.49968546794824));
#67719=CARTESIAN_POINT('Ctrl Pts',(0.117734811948404,-0.69538136064443,
-2.48384335452));
#67720=CARTESIAN_POINT('Ctrl Pts',(0.435427729238652,-0.554814757632145,
-2.46800124109176));
#67721=CARTESIAN_POINT('Ctrl Pts',(0.647473219121237,-0.279633962881997,
-2.45215912766353));
#67722=CARTESIAN_POINT('Ctrl Pts',(0.702422880414448,0.0633941617704607,
-2.43631701423529));
#67723=CARTESIAN_POINT('Ctrl Pts',(0.586944327597745,0.391041019558242,
-2.42047490080706));
#67724=CARTESIAN_POINT('Ctrl Pts',(0.329056015185207,0.623809956274138,
-2.40463278737882));
#67725=CARTESIAN_POINT('Ctrl Pts',(-0.0086708539911011,0.705224459989427,
-2.38879067395059));
#67726=CARTESIAN_POINT('Ctrl Pts',(-0.344293921879448,0.615531004932474,
-2.37294856052235));
#67727=CARTESIAN_POINT('Ctrl Pts',(-0.5963812737897,0.376491831185336,-2.35710644709412));
#67728=CARTESIAN_POINT('Ctrl Pts',(-0.672678295201022,0.141758276520581,
-2.34585093412633));
#67729=CARTESIAN_POINT('Ctrl Pts',(-0.676747086585303,0.0147670123138463,
-2.33987612563463));
#67730=CARTESIAN_POINT('Ctrl Pts',(-0.67673389899023,1.33698385852126E-5,
-2.339182021619));
#67731=CARTESIAN_POINT('Origin',(0.,0.,-3.278617978381));
#67732=CARTESIAN_POINT('',(-0.676702457484846,1.74000875470074E-5,-2.778617978381));
#67733=CARTESIAN_POINT('',(-0.676738003850817,-1.23232206216684E-5,-2.739182021619));
#67734=CARTESIAN_POINT('',(-0.6767,-6.21087748740391E-14,-3.278617978381));
#67735=CARTESIAN_POINT('Ctrl Pts',(-0.676702457484846,1.74000875470086E-5,
-2.778617978381));
#67736=CARTESIAN_POINT('Ctrl Pts',(-0.676613263759165,-0.0871212590025935,
-2.77451897863596));
#67737=CARTESIAN_POINT('Ctrl Pts',(-0.637924808175174,-0.286597009727134,
-2.76513927441484));
#67738=CARTESIAN_POINT('Ctrl Pts',(-0.447181721367947,-0.545385311748889,
-2.75047886571765));
#67739=CARTESIAN_POINT('Ctrl Pts',(-0.132564454783822,-0.692707336942753,
-2.73463675228941));
#67740=CARTESIAN_POINT('Ctrl Pts',(0.214216796165651,-0.67195822661804,
-2.71879463886118));
#67741=CARTESIAN_POINT('Ctrl Pts',(0.509022827335671,-0.488172612202699,
-2.70295252543294));
#67742=CARTESIAN_POINT('Ctrl Pts',(0.680325118730706,-0.185942077621786,
-2.68711041200471));
#67743=CARTESIAN_POINT('Ctrl Pts',(0.686560756397345,0.161403385589515,
-2.67126829857647));
#67744=CARTESIAN_POINT('Ctrl Pts',(0.526216791985425,0.469587707696419,
-2.65542618514823));
#67745=CARTESIAN_POINT('Ctrl Pts',(0.238197334034658,0.663836391711814,
-2.63958407172001));
#67746=CARTESIAN_POINT('Ctrl Pts',(-0.107615722986078,0.697019069108502,
-2.62374195829176));
#67747=CARTESIAN_POINT('Ctrl Pts',(-0.427318076565427,0.561084652399629,
-2.60789984486353));
#67748=CARTESIAN_POINT('Ctrl Pts',(-0.632421136632355,0.302767367517842,
-2.59285851822661));
#67749=CARTESIAN_POINT('Ctrl Pts',(-0.67663671448642,0.0952115438137001,
-2.58309789606577));
#67750=CARTESIAN_POINT('Ctrl Pts',(-0.676727467248305,-1.47039215481135E-5,
-2.57861797838101));
#67751=CARTESIAN_POINT('Ctrl Pts',(-0.676738003850817,-1.23232206217291E-5,
-2.739182021619));
#67752=CARTESIAN_POINT('Ctrl Pts',(-0.676749139750634,-0.0132249827090495,
-2.73856040420325));
#67753=CARTESIAN_POINT('Ctrl Pts',(-0.673150018663119,-0.138674493910342,
-2.73265808231143));
#67754=CARTESIAN_POINT('Ctrl Pts',(-0.598939416511963,-0.372408780057021,
-2.72147505594353));
#67755=CARTESIAN_POINT('Ctrl Pts',(-0.348490978460388,-0.613164545241514,
-2.7056329425153));
#67756=CARTESIAN_POINT('Ctrl Pts',(-0.0134884969402019,-0.705148767075711,
-2.68979082908706));
#67757=CARTESIAN_POINT('Ctrl Pts',(0.324786686361382,-0.626043393699459,
-2.67394871565883));
#67758=CARTESIAN_POINT('Ctrl Pts',(0.584259176083316,-0.395041691351842,
-2.65810660223059));
#67759=CARTESIAN_POINT('Ctrl Pts',(0.701973402101012,-0.068191388181339,
-2.64226448880235));
#67760=CARTESIAN_POINT('Ctrl Pts',(0.649368470484853,0.275204128232534,
-2.62642237537412));
#67761=CARTESIAN_POINT('Ctrl Pts',(0.439207867209178,0.551827121547341,
-2.61058026194588));
#67762=CARTESIAN_POINT('Ctrl Pts',(0.122482665136422,0.69456081044579,-2.59473814851765));
#67763=CARTESIAN_POINT('Ctrl Pts',(-0.223960392743318,0.668773852033162,
-2.57889603508941));
#67764=CARTESIAN_POINT('Ctrl Pts',(-0.516064147577321,0.480722912143853,
-2.56305392166118));
#67765=CARTESIAN_POINT('Ctrl Pts',(-0.65552228228443,0.226118938747654,
-2.54981591717104));
#67766=CARTESIAN_POINT('Ctrl Pts',(-0.676640597214846,0.0569141560676507,
-2.54185861715698));
#67767=CARTESIAN_POINT('Ctrl Pts',(-0.676642691248942,-7.12134560688915E-7,
-2.539182021619));
#67768=CARTESIAN_POINT('Ctrl Pts',(-0.291609820351005,0.201568937301636,
1.));
#67769=CARTESIAN_POINT('Ctrl Pts',(-0.291609820351005,0.201568937301636,
0.96));
#67770=CARTESIAN_POINT('Ctrl Pts',(-0.32673942707479,0.201568937301636,
1.));
#67771=CARTESIAN_POINT('Ctrl Pts',(-0.32673942707479,0.201568937301636,
0.96));
#67772=CARTESIAN_POINT('Ctrl Pts',(-0.349931773170829,0.179058706760406,
1.));
#67773=CARTESIAN_POINT('Ctrl Pts',(-0.349931773170829,0.179058706760406,
0.96));
#67774=CARTESIAN_POINT('',(-0.291609820351005,0.201568937301636,1.));
#67775=CARTESIAN_POINT('',(-0.349931773170829,0.179058706760406,1.));
#67776=CARTESIAN_POINT('Ctrl Pts',(-0.291609820351005,0.201568937301636,
1.));
#67777=CARTESIAN_POINT('Ctrl Pts',(-0.32673942707479,0.201568937301636,
1.));
#67778=CARTESIAN_POINT('Ctrl Pts',(-0.349931773170829,0.179058706760406,
1.));
#67779=CARTESIAN_POINT('',(-0.291609820351005,0.201568937301636,0.96));
#67780=CARTESIAN_POINT('',(-0.291609820351005,0.201568937301636,1.));
#67781=CARTESIAN_POINT('',(-0.349931773170829,0.179058706760406,0.96));
#67782=CARTESIAN_POINT('Ctrl Pts',(-0.291609820351005,0.201568937301636,
0.96));
#67783=CARTESIAN_POINT('Ctrl Pts',(-0.32673942707479,0.201568937301636,
0.96));
#67784=CARTESIAN_POINT('Ctrl Pts',(-0.349931773170829,0.179058706760406,
0.96));
#67785=CARTESIAN_POINT('',(-0.349931773170829,0.179058706760406,1.));
#67786=CARTESIAN_POINT('Ctrl Pts',(-0.23345836661756,0.178547120094299,
1.));
#67787=CARTESIAN_POINT('Ctrl Pts',(-0.23345836661756,0.178547120094299,
0.96));
#67788=CARTESIAN_POINT('Ctrl Pts',(-0.256821271404624,0.201568937301636,
1.));
#67789=CARTESIAN_POINT('Ctrl Pts',(-0.256821271404624,0.201568937301636,
0.96));
#67790=CARTESIAN_POINT('Ctrl Pts',(-0.291609820351005,0.201568937301636,
1.));
#67791=CARTESIAN_POINT('Ctrl Pts',(-0.291609820351005,0.201568937301636,
0.96));
#67792=CARTESIAN_POINT('',(-0.23345836661756,0.178547120094299,1.));
#67793=CARTESIAN_POINT('Ctrl Pts',(-0.23345836661756,0.178547120094299,
1.));
#67794=CARTESIAN_POINT('Ctrl Pts',(-0.256821271404624,0.201568937301636,
1.));
#67795=CARTESIAN_POINT('Ctrl Pts',(-0.291609820351005,0.201568937301636,
1.));
#67796=CARTESIAN_POINT('',(-0.23345836661756,0.178547120094299,0.96));
#67797=CARTESIAN_POINT('',(-0.23345836661756,0.178547120094299,1.));
#67798=CARTESIAN_POINT('Ctrl Pts',(-0.23345836661756,0.178547120094299,
0.96));
#67799=CARTESIAN_POINT('Ctrl Pts',(-0.256821271404624,0.201568937301636,
0.96));
#67800=CARTESIAN_POINT('Ctrl Pts',(-0.291609820351005,0.201568937301636,
0.96));
#67801=CARTESIAN_POINT('Ctrl Pts',(-0.210095491632819,0.121759927272797,
1.));
#67802=CARTESIAN_POINT('Ctrl Pts',(-0.210095491632819,0.121759927272797,
0.96));
#67803=CARTESIAN_POINT('Ctrl Pts',(-0.210095491632819,0.15552527308464,
1.));
#67804=CARTESIAN_POINT('Ctrl Pts',(-0.210095491632819,0.15552527308464,
0.96));
#67805=CARTESIAN_POINT('Ctrl Pts',(-0.23345836661756,0.178547120094299,
1.));
#67806=CARTESIAN_POINT('Ctrl Pts',(-0.23345836661756,0.178547120094299,
0.96));
#67807=CARTESIAN_POINT('',(-0.210095491632819,0.121759927272797,1.));
#67808=CARTESIAN_POINT('Ctrl Pts',(-0.210095491632819,0.121759927272797,
1.));
#67809=CARTESIAN_POINT('Ctrl Pts',(-0.210095491632819,0.15552527308464,
1.));
#67810=CARTESIAN_POINT('Ctrl Pts',(-0.23345836661756,0.178547120094299,
1.));
#67811=CARTESIAN_POINT('',(-0.210095491632819,0.121759927272797,0.96));
#67812=CARTESIAN_POINT('',(-0.210095491632819,0.121759927272797,1.));
#67813=CARTESIAN_POINT('Ctrl Pts',(-0.210095491632819,0.121759927272797,
0.96));
#67814=CARTESIAN_POINT('Ctrl Pts',(-0.210095491632819,0.15552527308464,
0.96));
#67815=CARTESIAN_POINT('Ctrl Pts',(-0.23345836661756,0.178547120094299,
0.96));
#67816=CARTESIAN_POINT('Ctrl Pts',(-0.232776251062751,0.0670191407203674,
1.));
#67817=CARTESIAN_POINT('Ctrl Pts',(-0.232776251062751,0.0670191407203674,
0.96));
#67818=CARTESIAN_POINT('Ctrl Pts',(-0.210095491632819,0.0893588423728943,
1.));
#67819=CARTESIAN_POINT('Ctrl Pts',(-0.210095491632819,0.0893588423728943,
0.96));
#67820=CARTESIAN_POINT('Ctrl Pts',(-0.210095491632819,0.121759927272797,
1.));
#67821=CARTESIAN_POINT('Ctrl Pts',(-0.210095491632819,0.121759927272797,
0.96));
#67822=CARTESIAN_POINT('',(-0.232776251062751,0.0670191407203674,1.));
#67823=CARTESIAN_POINT('Ctrl Pts',(-0.232776251062751,0.0670191407203674,
1.));
#67824=CARTESIAN_POINT('Ctrl Pts',(-0.210095491632819,0.0893588423728943,
1.));
#67825=CARTESIAN_POINT('Ctrl Pts',(-0.210095491632819,0.121759927272797,
1.));
#67826=CARTESIAN_POINT('',(-0.232776251062751,0.0670191407203674,0.96));
#67827=CARTESIAN_POINT('',(-0.232776251062751,0.0670191407203674,1.));
#67828=CARTESIAN_POINT('Ctrl Pts',(-0.232776251062751,0.0670191407203674,
0.96));
#67829=CARTESIAN_POINT('Ctrl Pts',(-0.210095491632819,0.0893588423728943,
0.96));
#67830=CARTESIAN_POINT('Ctrl Pts',(-0.210095491632819,0.121759927272797,
0.96));
#67831=CARTESIAN_POINT('Ctrl Pts',(-0.290927674993873,0.0446794390678406,
1.));
#67832=CARTESIAN_POINT('Ctrl Pts',(-0.290927674993873,0.0446794390678406,
0.96));
#67833=CARTESIAN_POINT('Ctrl Pts',(-0.255457010492682,0.0446794390678406,
1.));
#67834=CARTESIAN_POINT('Ctrl Pts',(-0.255457010492682,0.0446794390678406,
0.96));
#67835=CARTESIAN_POINT('Ctrl Pts',(-0.232776251062751,0.0670191407203674,
1.));
#67836=CARTESIAN_POINT('Ctrl Pts',(-0.232776251062751,0.0670191407203674,
0.96));
#67837=CARTESIAN_POINT('',(-0.290927674993873,0.0446794390678406,1.));
#67838=CARTESIAN_POINT('Ctrl Pts',(-0.290927674993873,0.0446794390678406,
1.));
#67839=CARTESIAN_POINT('Ctrl Pts',(-0.255457010492682,0.0446794390678406,
1.));
#67840=CARTESIAN_POINT('Ctrl Pts',(-0.232776251062751,0.0670191407203674,
1.));
#67841=CARTESIAN_POINT('',(-0.290927674993873,0.0446794390678406,0.96));
#67842=CARTESIAN_POINT('',(-0.290927674993873,0.0446794390678406,1.));
#67843=CARTESIAN_POINT('Ctrl Pts',(-0.290927674993873,0.0446794390678406,
0.96));
#67844=CARTESIAN_POINT('Ctrl Pts',(-0.255457010492682,0.0446794390678406,
0.96));
#67845=CARTESIAN_POINT('Ctrl Pts',(-0.232776251062751,0.0670191407203674,
0.96));
#67846=CARTESIAN_POINT('Ctrl Pts',(-0.350272860750556,0.0671896696090698,
1.));
#67847=CARTESIAN_POINT('Ctrl Pts',(-0.350272860750556,0.0671896696090698,
0.96));
#67848=CARTESIAN_POINT('Ctrl Pts',(-0.3274215426296,0.0446794390678406,
1.));
#67849=CARTESIAN_POINT('Ctrl Pts',(-0.3274215426296,0.0446794390678406,
0.96));
#67850=CARTESIAN_POINT('Ctrl Pts',(-0.290927674993873,0.0446794390678406,
1.));
#67851=CARTESIAN_POINT('Ctrl Pts',(-0.290927674993873,0.0446794390678406,
0.96));
#67852=CARTESIAN_POINT('',(-0.350272860750556,0.0671896696090698,1.));
#67853=CARTESIAN_POINT('Ctrl Pts',(-0.350272860750556,0.0671896696090698,
1.));
#67854=CARTESIAN_POINT('Ctrl Pts',(-0.3274215426296,0.0446794390678406,
1.));
#67855=CARTESIAN_POINT('Ctrl Pts',(-0.290927674993873,0.0446794390678406,
1.));
#67856=CARTESIAN_POINT('',(-0.350272860750556,0.0671896696090698,0.96));
#67857=CARTESIAN_POINT('',(-0.350272860750556,0.0671896696090698,1.));
#67858=CARTESIAN_POINT('Ctrl Pts',(-0.350272860750556,0.0671896696090698,
0.96));
#67859=CARTESIAN_POINT('Ctrl Pts',(-0.3274215426296,0.0446794390678406,
0.96));
#67860=CARTESIAN_POINT('Ctrl Pts',(-0.290927674993873,0.0446794390678406,
0.96));
#67861=CARTESIAN_POINT('Ctrl Pts',(-0.37312414906919,0.125170594453812,
1.));
#67862=CARTESIAN_POINT('Ctrl Pts',(-0.37312414906919,0.125170594453812,
0.96));
#67863=CARTESIAN_POINT('Ctrl Pts',(-0.37312414906919,0.0896999001502991,
1.));
#67864=CARTESIAN_POINT('Ctrl Pts',(-0.37312414906919,0.0896999001502991,
0.96));
#67865=CARTESIAN_POINT('Ctrl Pts',(-0.350272860750556,0.0671896696090698,
1.));
#67866=CARTESIAN_POINT('Ctrl Pts',(-0.350272860750556,0.0671896696090698,
0.96));
#67867=CARTESIAN_POINT('',(-0.37312414906919,0.125170594453812,1.));
#67868=CARTESIAN_POINT('Ctrl Pts',(-0.37312414906919,0.125170594453812,
1.));
#67869=CARTESIAN_POINT('Ctrl Pts',(-0.37312414906919,0.0896999001502991,
1.));
#67870=CARTESIAN_POINT('Ctrl Pts',(-0.350272860750556,0.0671896696090698,
1.));
#67871=CARTESIAN_POINT('',(-0.37312414906919,0.125170594453812,0.96));
#67872=CARTESIAN_POINT('',(-0.37312414906919,0.125170594453812,1.));
#67873=CARTESIAN_POINT('Ctrl Pts',(-0.37312414906919,0.125170594453812,
0.96));
#67874=CARTESIAN_POINT('Ctrl Pts',(-0.37312414906919,0.0896999001502991,
0.96));
#67875=CARTESIAN_POINT('Ctrl Pts',(-0.350272860750556,0.0671896696090698,
0.96));
#67876=CARTESIAN_POINT('Ctrl Pts',(-0.349931773170829,0.179058706760406,
1.));
#67877=CARTESIAN_POINT('Ctrl Pts',(-0.349931773170829,0.179058706760406,
0.96));
#67878=CARTESIAN_POINT('Ctrl Pts',(-0.37312414906919,0.156548476219177,
1.));
#67879=CARTESIAN_POINT('Ctrl Pts',(-0.37312414906919,0.156548476219177,
0.96));
#67880=CARTESIAN_POINT('Ctrl Pts',(-0.37312414906919,0.125170594453812,
1.));
#67881=CARTESIAN_POINT('Ctrl Pts',(-0.37312414906919,0.125170594453812,
0.96));
#67882=CARTESIAN_POINT('Ctrl Pts',(-0.349931773170829,0.179058706760406,
1.));
#67883=CARTESIAN_POINT('Ctrl Pts',(-0.37312414906919,0.156548476219177,
1.));
#67884=CARTESIAN_POINT('Ctrl Pts',(-0.37312414906919,0.125170594453812,
1.));
#67885=CARTESIAN_POINT('Ctrl Pts',(-0.349931773170829,0.179058706760406,
0.96));
#67886=CARTESIAN_POINT('Ctrl Pts',(-0.37312414906919,0.156548476219177,
0.96));
#67887=CARTESIAN_POINT('Ctrl Pts',(-0.37312414906919,0.125170594453812,
0.96));
#67888=CARTESIAN_POINT('Ctrl Pts',(-0.292633023485541,-0.00545700788497927,
1.));
#67889=CARTESIAN_POINT('Ctrl Pts',(-0.292633023485541,-0.00545700788497927,
0.96));
#67890=CARTESIAN_POINT('Ctrl Pts',(-0.335948136076331,-0.00545700788497927,
1.));
#67891=CARTESIAN_POINT('Ctrl Pts',(-0.335948136076331,-0.00545700788497927,
0.96));
#67892=CARTESIAN_POINT('Ctrl Pts',(-0.364426996931434,-0.0341063976287842,
1.));
#67893=CARTESIAN_POINT('Ctrl Pts',(-0.364426996931434,-0.0341063976287842,
0.96));
#67894=CARTESIAN_POINT('',(-0.292633023485541,-0.00545700788497927,1.));
#67895=CARTESIAN_POINT('',(-0.364426996931434,-0.0341063976287842,1.));
#67896=CARTESIAN_POINT('Ctrl Pts',(-0.292633023485541,-0.00545700788497927,
1.));
#67897=CARTESIAN_POINT('Ctrl Pts',(-0.335948136076331,-0.00545700788497927,
1.));
#67898=CARTESIAN_POINT('Ctrl Pts',(-0.364426996931434,-0.0341063976287842,
1.));
#67899=CARTESIAN_POINT('',(-0.292633023485541,-0.00545700788497927,0.96));
#67900=CARTESIAN_POINT('',(-0.292633023485541,-0.00545700788497927,1.));
#67901=CARTESIAN_POINT('',(-0.364426996931434,-0.0341063976287842,0.96));
#67902=CARTESIAN_POINT('Ctrl Pts',(-0.292633023485541,-0.00545700788497927,
0.96));
#67903=CARTESIAN_POINT('Ctrl Pts',(-0.335948136076331,-0.00545700788497927,
0.96));
#67904=CARTESIAN_POINT('Ctrl Pts',(-0.364426996931434,-0.0341063976287842,
0.96));
#67905=CARTESIAN_POINT('',(-0.364426996931434,-0.0341063976287842,1.));
#67906=CARTESIAN_POINT('Ctrl Pts',(-0.218792613968253,-0.034447455406189,
1.));
#67907=CARTESIAN_POINT('Ctrl Pts',(-0.218792613968253,-0.034447455406189,
0.96));
#67908=CARTESIAN_POINT('Ctrl Pts',(-0.248294677957892,-0.00545700788497927,
1.));
#67909=CARTESIAN_POINT('Ctrl Pts',(-0.248294677957892,-0.00545700788497927,
0.96));
#67910=CARTESIAN_POINT('Ctrl Pts',(-0.292633023485541,-0.00545700788497927,
1.));
#67911=CARTESIAN_POINT('Ctrl Pts',(-0.292633023485541,-0.00545700788497927,
0.96));
#67912=CARTESIAN_POINT('',(-0.218792613968253,-0.034447455406189,1.));
#67913=CARTESIAN_POINT('Ctrl Pts',(-0.218792613968253,-0.034447455406189,
1.));
#67914=CARTESIAN_POINT('Ctrl Pts',(-0.248294677957892,-0.00545700788497927,
1.));
#67915=CARTESIAN_POINT('Ctrl Pts',(-0.292633023485541,-0.00545700788497927,
1.));
#67916=CARTESIAN_POINT('',(-0.218792613968253,-0.034447455406189,0.96));
#67917=CARTESIAN_POINT('',(-0.218792613968253,-0.034447455406189,1.));
#67918=CARTESIAN_POINT('Ctrl Pts',(-0.218792613968253,-0.034447455406189,
0.96));
#67919=CARTESIAN_POINT('Ctrl Pts',(-0.248294677957892,-0.00545700788497927,
0.96));
#67920=CARTESIAN_POINT('Ctrl Pts',(-0.292633023485541,-0.00545700788497927,
0.96));
#67921=CARTESIAN_POINT('Ctrl Pts',(-0.189290579780936,-0.107776248455048,
1.));
#67922=CARTESIAN_POINT('Ctrl Pts',(-0.189290579780936,-0.107776248455048,
0.96));
#67923=CARTESIAN_POINT('Ctrl Pts',(-0.189290579780936,-0.0634379029273987,
1.));
#67924=CARTESIAN_POINT('Ctrl Pts',(-0.189290579780936,-0.0634379029273987,
0.96));
#67925=CARTESIAN_POINT('Ctrl Pts',(-0.218792613968253,-0.034447455406189,
1.));
#67926=CARTESIAN_POINT('Ctrl Pts',(-0.218792613968253,-0.034447455406189,
0.96));
#67927=CARTESIAN_POINT('',(-0.189290579780936,-0.107776248455048,1.));
#67928=CARTESIAN_POINT('Ctrl Pts',(-0.189290579780936,-0.107776248455048,
1.));
#67929=CARTESIAN_POINT('Ctrl Pts',(-0.189290579780936,-0.0634379029273987,
1.));
#67930=CARTESIAN_POINT('Ctrl Pts',(-0.218792613968253,-0.034447455406189,
1.));
#67931=CARTESIAN_POINT('',(-0.189290579780936,-0.107776248455048,0.96));
#67932=CARTESIAN_POINT('',(-0.189290579780936,-0.107776248455048,1.));
#67933=CARTESIAN_POINT('Ctrl Pts',(-0.189290579780936,-0.107776248455048,
0.96));
#67934=CARTESIAN_POINT('Ctrl Pts',(-0.189290579780936,-0.0634379029273987,
0.96));
#67935=CARTESIAN_POINT('Ctrl Pts',(-0.218792613968253,-0.034447455406189,
0.96));
#67936=CARTESIAN_POINT('Ctrl Pts',(-0.217939969524741,-0.179740750789642,
1.));
#67937=CARTESIAN_POINT('Ctrl Pts',(-0.217939969524741,-0.179740750789642,
0.96));
#67938=CARTESIAN_POINT('Ctrl Pts',(-0.189290579780936,-0.151432418823242,
1.));
#67939=CARTESIAN_POINT('Ctrl Pts',(-0.189290579780936,-0.151432418823242,
0.96));
#67940=CARTESIAN_POINT('Ctrl Pts',(-0.189290579780936,-0.107776248455048,
1.));
#67941=CARTESIAN_POINT('Ctrl Pts',(-0.189290579780936,-0.107776248455048,
0.96));
#67942=CARTESIAN_POINT('',(-0.217939969524741,-0.179740750789642,1.));
#67943=CARTESIAN_POINT('Ctrl Pts',(-0.217939969524741,-0.179740750789642,
1.));
#67944=CARTESIAN_POINT('Ctrl Pts',(-0.189290579780936,-0.151432418823242,
1.));
#67945=CARTESIAN_POINT('Ctrl Pts',(-0.189290579780936,-0.107776248455048,
1.));
#67946=CARTESIAN_POINT('',(-0.217939969524741,-0.179740750789642,0.96));
#67947=CARTESIAN_POINT('',(-0.217939969524741,-0.179740750789642,1.));
#67948=CARTESIAN_POINT('Ctrl Pts',(-0.217939969524741,-0.179740750789642,
0.96));
#67949=CARTESIAN_POINT('Ctrl Pts',(-0.189290579780936,-0.151432418823242,
0.96));
#67950=CARTESIAN_POINT('Ctrl Pts',(-0.189290579780936,-0.107776248455048,
0.96));
#67951=CARTESIAN_POINT('Ctrl Pts',(-0.290586617216468,-0.208049082756043,
1.));
#67952=CARTESIAN_POINT('Ctrl Pts',(-0.290586617216468,-0.208049082756043,
0.96));
#67953=CARTESIAN_POINT('Ctrl Pts',(-0.246589359268546,-0.208049082756043,
1.));
#67954=CARTESIAN_POINT('Ctrl Pts',(-0.246589359268546,-0.208049082756043,
0.96));
#67955=CARTESIAN_POINT('Ctrl Pts',(-0.217939969524741,-0.179740750789642,
1.));
#67956=CARTESIAN_POINT('Ctrl Pts',(-0.217939969524741,-0.179740750789642,
0.96));
#67957=CARTESIAN_POINT('',(-0.290586617216468,-0.208049082756043,1.));
#67958=CARTESIAN_POINT('Ctrl Pts',(-0.290586617216468,-0.208049082756043,
1.));
#67959=CARTESIAN_POINT('Ctrl Pts',(-0.246589359268546,-0.208049082756043,
1.));
#67960=CARTESIAN_POINT('Ctrl Pts',(-0.217939969524741,-0.179740750789642,
1.));
#67961=CARTESIAN_POINT('',(-0.290586617216468,-0.208049082756043,0.96));
#67962=CARTESIAN_POINT('',(-0.290586617216468,-0.208049082756043,1.));
#67963=CARTESIAN_POINT('Ctrl Pts',(-0.290586617216468,-0.208049082756043,
0.96));
#67964=CARTESIAN_POINT('Ctrl Pts',(-0.246589359268546,-0.208049082756043,
0.96));
#67965=CARTESIAN_POINT('Ctrl Pts',(-0.217939969524741,-0.179740750789642,
0.96));
#67966=CARTESIAN_POINT('Ctrl Pts',(-0.343451556190848,-0.194577062129974,
1.));
#67967=CARTESIAN_POINT('Ctrl Pts',(-0.343451556190848,-0.194577062129974,
0.96));
#67968=CARTESIAN_POINT('Ctrl Pts',(-0.318894949182868,-0.208049082756043,
1.));
#67969=CARTESIAN_POINT('Ctrl Pts',(-0.318894949182868,-0.208049082756043,
0.96));
#67970=CARTESIAN_POINT('Ctrl Pts',(-0.290586617216468,-0.208049082756043,
1.));
#67971=CARTESIAN_POINT('Ctrl Pts',(-0.290586617216468,-0.208049082756043,
0.96));
#67972=CARTESIAN_POINT('',(-0.343451556190848,-0.194577062129974,1.));
#67973=CARTESIAN_POINT('Ctrl Pts',(-0.343451556190848,-0.194577062129974,
1.));
#67974=CARTESIAN_POINT('Ctrl Pts',(-0.318894949182868,-0.208049082756043,
1.));
#67975=CARTESIAN_POINT('Ctrl Pts',(-0.290586617216468,-0.208049082756043,
1.));
#67976=CARTESIAN_POINT('',(-0.343451556190848,-0.194577062129974,0.96));
#67977=CARTESIAN_POINT('',(-0.343451556190848,-0.194577062129974,1.));
#67978=CARTESIAN_POINT('Ctrl Pts',(-0.343451556190848,-0.194577062129974,
0.96));
#67979=CARTESIAN_POINT('Ctrl Pts',(-0.318894949182868,-0.208049082756043,
0.96));
#67980=CARTESIAN_POINT('Ctrl Pts',(-0.290586617216468,-0.208049082756043,
0.96));
#67981=CARTESIAN_POINT('Ctrl Pts',(-0.380457010492682,-0.156548404693604,
1.));
#67982=CARTESIAN_POINT('Ctrl Pts',(-0.380457010492682,-0.156548404693604,
0.96));
#67983=CARTESIAN_POINT('Ctrl Pts',(-0.368008163198829,-0.181104981899261,
1.));
#67984=CARTESIAN_POINT('Ctrl Pts',(-0.368008163198829,-0.181104981899261,
0.96));
#67985=CARTESIAN_POINT('Ctrl Pts',(-0.343451556190848,-0.194577062129974,
1.));
#67986=CARTESIAN_POINT('Ctrl Pts',(-0.343451556190848,-0.194577062129974,
0.96));
#67987=CARTESIAN_POINT('',(-0.380457010492682,-0.156548404693604,1.));
#67988=CARTESIAN_POINT('Ctrl Pts',(-0.380457010492682,-0.156548404693604,
1.));
#67989=CARTESIAN_POINT('Ctrl Pts',(-0.368008163198829,-0.181104981899261,
1.));
#67990=CARTESIAN_POINT('Ctrl Pts',(-0.343451556190848,-0.194577062129974,
1.));
#67991=CARTESIAN_POINT('',(-0.380457010492682,-0.156548404693604,0.96));
#67992=CARTESIAN_POINT('',(-0.380457010492682,-0.156548404693604,1.));
#67993=CARTESIAN_POINT('Ctrl Pts',(-0.380457010492682,-0.156548404693604,
0.96));
#67994=CARTESIAN_POINT('Ctrl Pts',(-0.368008163198829,-0.181104981899261,
0.96));
#67995=CARTESIAN_POINT('Ctrl Pts',(-0.343451556190848,-0.194577062129974,
0.96));
#67996=CARTESIAN_POINT('Ctrl Pts',(-0.392905857786536,-0.105729842185974,
1.));
#67997=CARTESIAN_POINT('Ctrl Pts',(-0.392905857786536,-0.105729842185974,
0.96));
#67998=CARTESIAN_POINT('Ctrl Pts',(-0.392905857786536,-0.131991767883301,
1.));
#67999=CARTESIAN_POINT('Ctrl Pts',(-0.392905857786536,-0.131991767883301,
0.96));
#68000=CARTESIAN_POINT('Ctrl Pts',(-0.380457010492682,-0.156548404693604,
1.));
#68001=CARTESIAN_POINT('Ctrl Pts',(-0.380457010492682,-0.156548404693604,
0.96));
#68002=CARTESIAN_POINT('',(-0.392905857786536,-0.105729842185974,1.));
#68003=CARTESIAN_POINT('Ctrl Pts',(-0.392905857786536,-0.105729842185974,
1.));
#68004=CARTESIAN_POINT('Ctrl Pts',(-0.392905857786536,-0.131991767883301,
1.));
#68005=CARTESIAN_POINT('Ctrl Pts',(-0.380457010492682,-0.156548404693604,
1.));
#68006=CARTESIAN_POINT('',(-0.392905857786536,-0.105729842185974,0.96));
#68007=CARTESIAN_POINT('',(-0.392905857786536,-0.105729842185974,1.));
#68008=CARTESIAN_POINT('Ctrl Pts',(-0.392905857786536,-0.105729842185974,
0.96));
#68009=CARTESIAN_POINT('Ctrl Pts',(-0.392905857786536,-0.131991767883301,
0.96));
#68010=CARTESIAN_POINT('Ctrl Pts',(-0.380457010492682,-0.156548404693604,
0.96));
#68011=CARTESIAN_POINT('Ctrl Pts',(-0.364426996931434,-0.0341063976287842,
1.));
#68012=CARTESIAN_POINT('Ctrl Pts',(-0.364426996931434,-0.0341063976287842,
0.96));
#68013=CARTESIAN_POINT('Ctrl Pts',(-0.392905857786536,-0.0627557873725891,
1.));
#68014=CARTESIAN_POINT('Ctrl Pts',(-0.392905857786536,-0.0627557873725891,
0.96));
#68015=CARTESIAN_POINT('Ctrl Pts',(-0.392905857786536,-0.105729842185974,
1.));
#68016=CARTESIAN_POINT('Ctrl Pts',(-0.392905857786536,-0.105729842185974,
0.96));
#68017=CARTESIAN_POINT('Ctrl Pts',(-0.364426996931434,-0.0341063976287842,
1.));
#68018=CARTESIAN_POINT('Ctrl Pts',(-0.392905857786536,-0.0627557873725891,
1.));
#68019=CARTESIAN_POINT('Ctrl Pts',(-0.392905857786536,-0.105729842185974,
1.));
#68020=CARTESIAN_POINT('Ctrl Pts',(-0.364426996931434,-0.0341063976287842,
0.96));
#68021=CARTESIAN_POINT('Ctrl Pts',(-0.392905857786536,-0.0627557873725891,
0.96));
#68022=CARTESIAN_POINT('Ctrl Pts',(-0.392905857786536,-0.105729842185974,
0.96));
#68023=CARTESIAN_POINT('Ctrl Pts',(-0.410641190037131,-0.214699828624725,
1.));
#68024=CARTESIAN_POINT('Ctrl Pts',(-0.410641190037131,-0.214699828624725,
0.96));
#68025=CARTESIAN_POINT('Ctrl Pts',(-0.456002723798156,-0.170873069763184,
1.));
#68026=CARTESIAN_POINT('Ctrl Pts',(-0.456002723798156,-0.170873069763184,
0.96));
#68027=CARTESIAN_POINT('Ctrl Pts',(-0.456002723798156,-0.105388784408569,
1.));
#68028=CARTESIAN_POINT('Ctrl Pts',(-0.456002723798156,-0.105388784408569,
0.96));
#68029=CARTESIAN_POINT('',(-0.410641190037131,-0.214699828624725,1.));
#68030=CARTESIAN_POINT('',(-0.456002723798156,-0.105388784408569,1.));
#68031=CARTESIAN_POINT('Ctrl Pts',(-0.410641190037131,-0.214699828624725,
1.));
#68032=CARTESIAN_POINT('Ctrl Pts',(-0.456002723798156,-0.170873069763184,
1.));
#68033=CARTESIAN_POINT('Ctrl Pts',(-0.456002723798156,-0.105388784408569,
1.));
#68034=CARTESIAN_POINT('',(-0.410641190037131,-0.214699828624725,0.96));
#68035=CARTESIAN_POINT('',(-0.410641190037131,-0.214699828624725,1.));
#68036=CARTESIAN_POINT('',(-0.456002723798156,-0.105388784408569,0.96));
#68037=CARTESIAN_POINT('Ctrl Pts',(-0.410641190037131,-0.214699828624725,
0.96));
#68038=CARTESIAN_POINT('Ctrl Pts',(-0.456002723798156,-0.170873069763184,
0.96));
#68039=CARTESIAN_POINT('Ctrl Pts',(-0.456002723798156,-0.105388784408569,
0.96));
#68040=CARTESIAN_POINT('',(-0.456002723798156,-0.105388784408569,1.));
#68041=CARTESIAN_POINT('Ctrl Pts',(-0.291268732771277,-0.258526587486267,
1.));
#68042=CARTESIAN_POINT('Ctrl Pts',(-0.291268732771277,-0.258526587486267,
0.96));
#68043=CARTESIAN_POINT('Ctrl Pts',(-0.365279641374946,-0.258526587486267,
1.));
#68044=CARTESIAN_POINT('Ctrl Pts',(-0.365279641374946,-0.258526587486267,
0.96));
#68045=CARTESIAN_POINT('Ctrl Pts',(-0.410641190037131,-0.214699828624725,
1.));
#68046=CARTESIAN_POINT('Ctrl Pts',(-0.410641190037131,-0.214699828624725,
0.96));
#68047=CARTESIAN_POINT('',(-0.291268732771277,-0.258526587486267,1.));
#68048=CARTESIAN_POINT('Ctrl Pts',(-0.291268732771277,-0.258526587486267,
1.));
#68049=CARTESIAN_POINT('Ctrl Pts',(-0.365279641374946,-0.258526587486267,
1.));
#68050=CARTESIAN_POINT('Ctrl Pts',(-0.410641190037131,-0.214699828624725,
1.));
#68051=CARTESIAN_POINT('',(-0.291268732771277,-0.258526587486267,0.96));
#68052=CARTESIAN_POINT('',(-0.291268732771277,-0.258526587486267,1.));
#68053=CARTESIAN_POINT('Ctrl Pts',(-0.291268732771277,-0.258526587486267,
0.96));
#68054=CARTESIAN_POINT('Ctrl Pts',(-0.365279641374946,-0.258526587486267,
0.96));
#68055=CARTESIAN_POINT('Ctrl Pts',(-0.410641190037131,-0.214699828624725,
0.96));
#68056=CARTESIAN_POINT('Ctrl Pts',(-0.171896305307746,-0.214870357513428,
1.));
#68057=CARTESIAN_POINT('Ctrl Pts',(-0.171896305307746,-0.214870357513428,
0.96));
#68058=CARTESIAN_POINT('Ctrl Pts',(-0.217257824167609,-0.258526587486267,
1.));
#68059=CARTESIAN_POINT('Ctrl Pts',(-0.217257824167609,-0.258526587486267,
0.96));
#68060=CARTESIAN_POINT('Ctrl Pts',(-0.291268732771277,-0.258526587486267,
1.));
#68061=CARTESIAN_POINT('Ctrl Pts',(-0.291268732771277,-0.258526587486267,
0.96));
#68062=CARTESIAN_POINT('',(-0.171896305307746,-0.214870357513428,1.));
#68063=CARTESIAN_POINT('Ctrl Pts',(-0.171896305307746,-0.214870357513428,
1.));
#68064=CARTESIAN_POINT('Ctrl Pts',(-0.217257824167609,-0.258526587486267,
1.));
#68065=CARTESIAN_POINT('Ctrl Pts',(-0.291268732771277,-0.258526587486267,
1.));
#68066=CARTESIAN_POINT('',(-0.171896305307746,-0.214870357513428,0.96));
#68067=CARTESIAN_POINT('',(-0.171896305307746,-0.214870357513428,1.));
#68068=CARTESIAN_POINT('Ctrl Pts',(-0.171896305307746,-0.214870357513428,
0.96));
#68069=CARTESIAN_POINT('Ctrl Pts',(-0.217257824167609,-0.258526587486267,
0.96));
#68070=CARTESIAN_POINT('Ctrl Pts',(-0.291268732771277,-0.258526587486267,
0.96));
#68071=CARTESIAN_POINT('Ctrl Pts',(-0.126534726843238,-0.107094132900238,
1.));
#68072=CARTESIAN_POINT('Ctrl Pts',(-0.126534726843238,-0.107094132900238,
0.96));
#68073=CARTESIAN_POINT('Ctrl Pts',(-0.126534726843238,-0.171214127540588,
1.));
#68074=CARTESIAN_POINT('Ctrl Pts',(-0.126534726843238,-0.171214127540588,
0.96));
#68075=CARTESIAN_POINT('Ctrl Pts',(-0.171896305307746,-0.214870357513428,
1.));
#68076=CARTESIAN_POINT('Ctrl Pts',(-0.171896305307746,-0.214870357513428,
0.96));
#68077=CARTESIAN_POINT('',(-0.126534726843238,-0.107094132900238,1.));
#68078=CARTESIAN_POINT('Ctrl Pts',(-0.126534726843238,-0.107094132900238,
1.));
#68079=CARTESIAN_POINT('Ctrl Pts',(-0.126534726843238,-0.171214127540588,
1.));
#68080=CARTESIAN_POINT('Ctrl Pts',(-0.171896305307746,-0.214870357513428,
1.));
#68081=CARTESIAN_POINT('',(-0.126534726843238,-0.107094132900238,0.96));
#68082=CARTESIAN_POINT('',(-0.126534726843238,-0.107094132900238,1.));
#68083=CARTESIAN_POINT('Ctrl Pts',(-0.126534726843238,-0.107094132900238,
0.96));
#68084=CARTESIAN_POINT('Ctrl Pts',(-0.126534726843238,-0.171214127540588,
0.96));
#68085=CARTESIAN_POINT('Ctrl Pts',(-0.171896305307746,-0.214870357513428,
0.96));
#68086=CARTESIAN_POINT('Ctrl Pts',(-0.150579776987433,-0.0272850632667542,
1.));
#68087=CARTESIAN_POINT('Ctrl Pts',(-0.150579776987433,-0.0272850632667542,
0.96));
#68088=CARTESIAN_POINT('Ctrl Pts',(-0.126534726843238,-0.0607093811035156,
1.));
#68089=CARTESIAN_POINT('Ctrl Pts',(-0.126534726843238,-0.0607093811035156,
0.96));
#68090=CARTESIAN_POINT('Ctrl Pts',(-0.126534726843238,-0.107094132900238,
1.));
#68091=CARTESIAN_POINT('Ctrl Pts',(-0.126534726843238,-0.107094132900238,
0.96));
#68092=CARTESIAN_POINT('',(-0.150579776987433,-0.0272850632667542,1.));
#68093=CARTESIAN_POINT('Ctrl Pts',(-0.150579776987433,-0.0272850632667542,
1.));
#68094=CARTESIAN_POINT('Ctrl Pts',(-0.126534726843238,-0.0607093811035156,
1.));
#68095=CARTESIAN_POINT('Ctrl Pts',(-0.126534726843238,-0.107094132900238,
1.));
#68096=CARTESIAN_POINT('',(-0.150579776987433,-0.0272850632667542,0.96));
#68097=CARTESIAN_POINT('',(-0.150579776987433,-0.0272850632667542,1.));
#68098=CARTESIAN_POINT('Ctrl Pts',(-0.150579776987433,-0.0272850632667542,
0.96));
#68099=CARTESIAN_POINT('Ctrl Pts',(-0.126534726843238,-0.0607093811035156,
0.96));
#68100=CARTESIAN_POINT('Ctrl Pts',(-0.126534726843238,-0.107094132900238,
0.96));
#68101=CARTESIAN_POINT('Ctrl Pts',(-0.220668461546302,0.021146035194397,
1.));
#68102=CARTESIAN_POINT('Ctrl Pts',(-0.220668461546302,0.021146035194397,
0.96));
#68103=CARTESIAN_POINT('Ctrl Pts',(-0.174624797329307,0.00613919496536253,
1.));
#68104=CARTESIAN_POINT('Ctrl Pts',(-0.174624797329307,0.00613919496536253,
0.96));
#68105=CARTESIAN_POINT('Ctrl Pts',(-0.150579776987433,-0.0272850632667542,
1.));
#68106=CARTESIAN_POINT('Ctrl Pts',(-0.150579776987433,-0.0272850632667542,
0.96));
#68107=CARTESIAN_POINT('',(-0.220668461546302,0.021146035194397,1.));
#68108=CARTESIAN_POINT('Ctrl Pts',(-0.220668461546302,0.021146035194397,
1.));
#68109=CARTESIAN_POINT('Ctrl Pts',(-0.174624797329307,0.00613919496536253,
1.));
#68110=CARTESIAN_POINT('Ctrl Pts',(-0.150579776987433,-0.0272850632667542,
1.));
#68111=CARTESIAN_POINT('',(-0.220668461546302,0.021146035194397,0.96));
#68112=CARTESIAN_POINT('',(-0.220668461546302,0.021146035194397,1.));
#68113=CARTESIAN_POINT('Ctrl Pts',(-0.220668461546302,0.021146035194397,
0.96));
#68114=CARTESIAN_POINT('Ctrl Pts',(-0.174624797329307,0.00613919496536253,
0.96));
#68115=CARTESIAN_POINT('Ctrl Pts',(-0.150579776987433,-0.0272850632667542,
0.96));
#68116=CARTESIAN_POINT('Ctrl Pts',(-0.165245559439063,0.0608799815177917,
1.));
#68117=CARTESIAN_POINT('Ctrl Pts',(-0.165245559439063,0.0608799815177917,
0.96));
#68118=CARTESIAN_POINT('Ctrl Pts',(-0.183492478355765,0.0351296424865722,
1.));
#68119=CARTESIAN_POINT('Ctrl Pts',(-0.183492478355765,0.0351296424865722,
0.96));
#68120=CARTESIAN_POINT('Ctrl Pts',(-0.220668461546302,0.021146035194397,
1.));
#68121=CARTESIAN_POINT('Ctrl Pts',(-0.220668461546302,0.021146035194397,
0.96));
#68122=CARTESIAN_POINT('',(-0.165245559439063,0.0608799815177917,1.));
#68123=CARTESIAN_POINT('Ctrl Pts',(-0.165245559439063,0.0608799815177917,
1.));
#68124=CARTESIAN_POINT('Ctrl Pts',(-0.183492478355765,0.0351296424865722,
1.));
#68125=CARTESIAN_POINT('Ctrl Pts',(-0.220668461546302,0.021146035194397,
1.));
#68126=CARTESIAN_POINT('',(-0.165245559439063,0.0608799815177917,0.96));
#68127=CARTESIAN_POINT('',(-0.165245559439063,0.0608799815177917,1.));
#68128=CARTESIAN_POINT('Ctrl Pts',(-0.165245559439063,0.0608799815177917,
0.96));
#68129=CARTESIAN_POINT('Ctrl Pts',(-0.183492478355765,0.0351296424865722,
0.96));
#68130=CARTESIAN_POINT('Ctrl Pts',(-0.220668461546302,0.021146035194397,
0.96));
#68131=CARTESIAN_POINT('Ctrl Pts',(-0.146998610720038,0.121418869495392,
1.));
#68132=CARTESIAN_POINT('Ctrl Pts',(-0.146998610720038,0.121418869495392,
0.96));
#68133=CARTESIAN_POINT('Ctrl Pts',(-0.146998610720038,0.0866303205490112,
1.));
#68134=CARTESIAN_POINT('Ctrl Pts',(-0.146998610720038,0.0866303205490112,
0.96));
#68135=CARTESIAN_POINT('Ctrl Pts',(-0.165245559439063,0.0608799815177917,
1.));
#68136=CARTESIAN_POINT('Ctrl Pts',(-0.165245559439063,0.0608799815177917,
0.96));
#68137=CARTESIAN_POINT('',(-0.146998610720038,0.121418869495392,1.));
#68138=CARTESIAN_POINT('Ctrl Pts',(-0.146998610720038,0.121418869495392,
1.));
#68139=CARTESIAN_POINT('Ctrl Pts',(-0.146998610720038,0.0866303205490112,
1.));
#68140=CARTESIAN_POINT('Ctrl Pts',(-0.165245559439063,0.0608799815177917,
1.));
#68141=CARTESIAN_POINT('',(-0.146998610720038,0.121418869495392,0.96));
#68142=CARTESIAN_POINT('',(-0.146998610720038,0.121418869495392,1.));
#68143=CARTESIAN_POINT('Ctrl Pts',(-0.146998610720038,0.121418869495392,
0.96));
#68144=CARTESIAN_POINT('Ctrl Pts',(-0.146998610720038,0.0866303205490112,
0.96));
#68145=CARTESIAN_POINT('Ctrl Pts',(-0.165245559439063,0.0608799815177917,
0.96));
#68146=CARTESIAN_POINT('Ctrl Pts',(-0.186903115734458,0.214017784595489,
1.));
#68147=CARTESIAN_POINT('Ctrl Pts',(-0.186903115734458,0.214017784595489,
0.96));
#68148=CARTESIAN_POINT('Ctrl Pts',(-0.146998610720038,0.175989127159119,
1.));
#68149=CARTESIAN_POINT('Ctrl Pts',(-0.146998610720038,0.175989127159119,
0.96));
#68150=CARTESIAN_POINT('Ctrl Pts',(-0.146998610720038,0.121418869495392,
1.));
#68151=CARTESIAN_POINT('Ctrl Pts',(-0.146998610720038,0.121418869495392,
0.96));
#68152=CARTESIAN_POINT('',(-0.186903115734458,0.214017784595489,1.));
#68153=CARTESIAN_POINT('Ctrl Pts',(-0.186903115734458,0.214017784595489,
1.));
#68154=CARTESIAN_POINT('Ctrl Pts',(-0.146998610720038,0.175989127159119,
1.));
#68155=CARTESIAN_POINT('Ctrl Pts',(-0.146998610720038,0.121418869495392,
1.));
#68156=CARTESIAN_POINT('',(-0.186903115734458,0.214017784595489,0.96));
#68157=CARTESIAN_POINT('',(-0.186903115734458,0.214017784595489,1.));
#68158=CARTESIAN_POINT('Ctrl Pts',(-0.186903115734458,0.214017784595489,
0.96));
#68159=CARTESIAN_POINT('Ctrl Pts',(-0.146998610720038,0.175989127159119,
0.96));
#68160=CARTESIAN_POINT('Ctrl Pts',(-0.146998610720038,0.121418869495392,
0.96));
#68161=CARTESIAN_POINT('Ctrl Pts',(-0.292291965708137,0.252046382427216,
1.));
#68162=CARTESIAN_POINT('Ctrl Pts',(-0.292291965708137,0.252046382427216,
0.96));
#68163=CARTESIAN_POINT('Ctrl Pts',(-0.226807620748878,0.252046382427216,
1.));
#68164=CARTESIAN_POINT('Ctrl Pts',(-0.226807620748878,0.252046382427216,
0.96));
#68165=CARTESIAN_POINT('Ctrl Pts',(-0.186903115734458,0.214017784595489,
1.));
#68166=CARTESIAN_POINT('Ctrl Pts',(-0.186903115734458,0.214017784595489,
0.96));
#68167=CARTESIAN_POINT('',(-0.292291965708137,0.252046382427216,1.));
#68168=CARTESIAN_POINT('Ctrl Pts',(-0.292291965708137,0.252046382427216,
1.));
#68169=CARTESIAN_POINT('Ctrl Pts',(-0.226807620748878,0.252046382427216,
1.));
#68170=CARTESIAN_POINT('Ctrl Pts',(-0.186903115734458,0.214017784595489,
1.));
#68171=CARTESIAN_POINT('',(-0.292291965708137,0.252046382427216,0.96));
#68172=CARTESIAN_POINT('',(-0.292291965708137,0.252046382427216,1.));
#68173=CARTESIAN_POINT('Ctrl Pts',(-0.292291965708137,0.252046382427216,
0.96));
#68174=CARTESIAN_POINT('Ctrl Pts',(-0.226807620748878,0.252046382427216,
0.96));
#68175=CARTESIAN_POINT('Ctrl Pts',(-0.186903115734458,0.214017784595489,
0.96));
#68176=CARTESIAN_POINT('Ctrl Pts',(-0.396657552942634,0.214870429039001,
1.));
#68177=CARTESIAN_POINT('Ctrl Pts',(-0.396657552942634,0.214870429039001,
0.96));
#68178=CARTESIAN_POINT('Ctrl Pts',(-0.357435193285346,0.252046382427216,
1.));
#68179=CARTESIAN_POINT('Ctrl Pts',(-0.357435193285346,0.252046382427216,
0.96));
#68180=CARTESIAN_POINT('Ctrl Pts',(-0.292291965708137,0.252046382427216,
1.));
#68181=CARTESIAN_POINT('Ctrl Pts',(-0.292291965708137,0.252046382427216,
0.96));
#68182=CARTESIAN_POINT('',(-0.396657552942634,0.214870429039001,1.));
#68183=CARTESIAN_POINT('Ctrl Pts',(-0.396657552942634,0.214870429039001,
1.));
#68184=CARTESIAN_POINT('Ctrl Pts',(-0.357435193285346,0.252046382427216,
1.));
#68185=CARTESIAN_POINT('Ctrl Pts',(-0.292291965708137,0.252046382427216,
1.));
#68186=CARTESIAN_POINT('',(-0.396657552942634,0.214870429039001,0.96));
#68187=CARTESIAN_POINT('',(-0.396657552942634,0.214870429039001,1.));
#68188=CARTESIAN_POINT('Ctrl Pts',(-0.396657552942634,0.214870429039001,
0.96));
#68189=CARTESIAN_POINT('Ctrl Pts',(-0.357435193285346,0.252046382427216,
0.96));
#68190=CARTESIAN_POINT('Ctrl Pts',(-0.292291965708137,0.252046382427216,
0.96));
#68191=CARTESIAN_POINT('Ctrl Pts',(-0.435879942402244,0.123124188184738,
1.));
#68192=CARTESIAN_POINT('Ctrl Pts',(-0.435879942402244,0.123124188184738,
0.96));
#68193=CARTESIAN_POINT('Ctrl Pts',(-0.435879942402244,0.177694445848465,
1.));
#68194=CARTESIAN_POINT('Ctrl Pts',(-0.435879942402244,0.177694445848465,
0.96));
#68195=CARTESIAN_POINT('Ctrl Pts',(-0.396657552942634,0.214870429039001,
1.));
#68196=CARTESIAN_POINT('Ctrl Pts',(-0.396657552942634,0.214870429039001,
0.96));
#68197=CARTESIAN_POINT('',(-0.435879942402244,0.123124188184738,1.));
#68198=CARTESIAN_POINT('Ctrl Pts',(-0.435879942402244,0.123124188184738,
1.));
#68199=CARTESIAN_POINT('Ctrl Pts',(-0.435879942402244,0.177694445848465,
1.));
#68200=CARTESIAN_POINT('Ctrl Pts',(-0.396657552942634,0.214870429039001,
1.));
#68201=CARTESIAN_POINT('',(-0.435879942402244,0.123124188184738,0.96));
#68202=CARTESIAN_POINT('',(-0.435879942402244,0.123124188184738,1.));
#68203=CARTESIAN_POINT('Ctrl Pts',(-0.435879942402244,0.123124188184738,
0.96));
#68204=CARTESIAN_POINT('Ctrl Pts',(-0.435879942402244,0.177694445848465,
0.96));
#68205=CARTESIAN_POINT('Ctrl Pts',(-0.396657552942634,0.214870429039001,
0.96));
#68206=CARTESIAN_POINT('Ctrl Pts',(-0.417462464794517,0.0610505104064941,
1.));
#68207=CARTESIAN_POINT('Ctrl Pts',(-0.417462464794517,0.0610505104064941,
0.96));
#68208=CARTESIAN_POINT('Ctrl Pts',(-0.435879942402244,0.0869714081287384,
1.));
#68209=CARTESIAN_POINT('Ctrl Pts',(-0.435879942402244,0.0869714081287384,
0.96));
#68210=CARTESIAN_POINT('Ctrl Pts',(-0.435879942402244,0.123124188184738,
1.));
#68211=CARTESIAN_POINT('Ctrl Pts',(-0.435879942402244,0.123124188184738,
0.96));
#68212=CARTESIAN_POINT('',(-0.417462464794517,0.0610505104064941,1.));
#68213=CARTESIAN_POINT('Ctrl Pts',(-0.417462464794517,0.0610505104064941,
1.));
#68214=CARTESIAN_POINT('Ctrl Pts',(-0.435879942402244,0.0869714081287384,
1.));
#68215=CARTESIAN_POINT('Ctrl Pts',(-0.435879942402244,0.123124188184738,
1.));
#68216=CARTESIAN_POINT('',(-0.417462464794517,0.0610505104064941,0.96));
#68217=CARTESIAN_POINT('',(-0.417462464794517,0.0610505104064941,1.));
#68218=CARTESIAN_POINT('Ctrl Pts',(-0.417462464794517,0.0610505104064941,
0.96));
#68219=CARTESIAN_POINT('Ctrl Pts',(-0.435879942402244,0.0869714081287384,
0.96));
#68220=CARTESIAN_POINT('Ctrl Pts',(-0.435879942402244,0.123124188184738,
0.96));
#68221=CARTESIAN_POINT('Ctrl Pts',(-0.360845830664039,0.021146035194397,
1.));
#68222=CARTESIAN_POINT('Ctrl Pts',(-0.360845830664039,0.021146035194397,
0.96));
#68223=CARTESIAN_POINT('Ctrl Pts',(-0.399045016989112,0.0351296424865722,
1.));
#68224=CARTESIAN_POINT('Ctrl Pts',(-0.399045016989112,0.0351296424865722,
0.96));
#68225=CARTESIAN_POINT('Ctrl Pts',(-0.417462464794517,0.0610505104064941,
1.));
#68226=CARTESIAN_POINT('Ctrl Pts',(-0.417462464794517,0.0610505104064941,
0.96));
#68227=CARTESIAN_POINT('',(-0.360845830664039,0.021146035194397,1.));
#68228=CARTESIAN_POINT('Ctrl Pts',(-0.360845830664039,0.021146035194397,
1.));
#68229=CARTESIAN_POINT('Ctrl Pts',(-0.399045016989112,0.0351296424865722,
1.));
#68230=CARTESIAN_POINT('Ctrl Pts',(-0.417462464794517,0.0610505104064941,
1.));
#68231=CARTESIAN_POINT('',(-0.360845830664039,0.021146035194397,0.96));
#68232=CARTESIAN_POINT('',(-0.360845830664039,0.021146035194397,1.));
#68233=CARTESIAN_POINT('Ctrl Pts',(-0.360845830664039,0.021146035194397,
0.96));
#68234=CARTESIAN_POINT('Ctrl Pts',(-0.399045016989112,0.0351296424865722,
0.96));
#68235=CARTESIAN_POINT('Ctrl Pts',(-0.417462464794517,0.0610505104064941,
0.96));
#68236=CARTESIAN_POINT('Ctrl Pts',(-0.431275573000312,-0.0237038969993592,
1.));
#68237=CARTESIAN_POINT('Ctrl Pts',(-0.431275573000312,-0.0237038969993592,
0.96));
#68238=CARTESIAN_POINT('Ctrl Pts',(-0.406548422202468,0.00920877456665037,
1.));
#68239=CARTESIAN_POINT('Ctrl Pts',(-0.406548422202468,0.00920877456665037,
0.96));
#68240=CARTESIAN_POINT('Ctrl Pts',(-0.360845830664039,0.021146035194397,
1.));
#68241=CARTESIAN_POINT('Ctrl Pts',(-0.360845830664039,0.021146035194397,
0.96));
#68242=CARTESIAN_POINT('',(-0.431275573000312,-0.0237038969993592,1.));
#68243=CARTESIAN_POINT('Ctrl Pts',(-0.431275573000312,-0.0237038969993592,
1.));
#68244=CARTESIAN_POINT('Ctrl Pts',(-0.406548422202468,0.00920877456665037,
1.));
#68245=CARTESIAN_POINT('Ctrl Pts',(-0.360845830664039,0.021146035194397,
1.));
#68246=CARTESIAN_POINT('',(-0.431275573000312,-0.0237038969993592,0.96));
#68247=CARTESIAN_POINT('',(-0.431275573000312,-0.0237038969993592,1.));
#68248=CARTESIAN_POINT('Ctrl Pts',(-0.431275573000312,-0.0237038969993592,
0.96));
#68249=CARTESIAN_POINT('Ctrl Pts',(-0.406548422202468,0.00920877456665037,
0.96));
#68250=CARTESIAN_POINT('Ctrl Pts',(-0.360845830664039,0.021146035194397,
0.96));
#68251=CARTESIAN_POINT('Ctrl Pts',(-0.456002723798156,-0.105388784408569,
1.));
#68252=CARTESIAN_POINT('Ctrl Pts',(-0.456002723798156,-0.105388784408569,
0.96));
#68253=CARTESIAN_POINT('Ctrl Pts',(-0.456002723798156,-0.0566166281700134,
1.));
#68254=CARTESIAN_POINT('Ctrl Pts',(-0.456002723798156,-0.0566166281700134,
0.96));
#68255=CARTESIAN_POINT('Ctrl Pts',(-0.431275573000312,-0.0237038969993592,
1.));
#68256=CARTESIAN_POINT('Ctrl Pts',(-0.431275573000312,-0.0237038969993592,
0.96));
#68257=CARTESIAN_POINT('Ctrl Pts',(-0.456002723798156,-0.105388784408569,
1.));
#68258=CARTESIAN_POINT('Ctrl Pts',(-0.456002723798156,-0.0566166281700134,
1.));
#68259=CARTESIAN_POINT('Ctrl Pts',(-0.431275573000312,-0.0237038969993592,
1.));
#68260=CARTESIAN_POINT('Ctrl Pts',(-0.456002723798156,-0.105388784408569,
0.96));
#68261=CARTESIAN_POINT('Ctrl Pts',(-0.456002723798156,-0.0566166281700134,
0.96));
#68262=CARTESIAN_POINT('Ctrl Pts',(-0.431275573000312,-0.0237038969993592,
0.96));
#68263=CARTESIAN_POINT('Origin',(-0.291268725320697,-0.00324010252952578,
0.96));
#68264=CARTESIAN_POINT('Origin',(-0.0324011113494634,-0.180081808567047,
1.));
#68265=CARTESIAN_POINT('',(-0.0324011113494634,-0.180081808567047,1.));
#68266=CARTESIAN_POINT('',(0.0375170443207026,-0.180081808567047,1.));
#68267=CARTESIAN_POINT('',(-0.0162005556747317,-0.180081808567047,1.));
#68268=CARTESIAN_POINT('',(-0.0324011113494634,-0.180081808567047,0.96));
#68269=CARTESIAN_POINT('',(-0.0324011113494634,-0.180081808567047,1.));
#68270=CARTESIAN_POINT('',(0.0375170443207026,-0.180081808567047,0.96));
#68271=CARTESIAN_POINT('',(-0.0324011113494634,-0.180081808567047,0.96));
#68272=CARTESIAN_POINT('',(0.0375170443207026,-0.180081808567047,1.));
#68273=CARTESIAN_POINT('Origin',(-0.0324011113494634,-0.249999964237213,
1.));
#68274=CARTESIAN_POINT('',(-0.0324011113494634,-0.249999964237213,1.));
#68275=CARTESIAN_POINT('',(-0.0324011113494634,-0.124999982118607,1.));
#68276=CARTESIAN_POINT('',(-0.0324011113494634,-0.249999964237213,0.96));
#68277=CARTESIAN_POINT('',(-0.0324011113494634,-0.249999964237213,1.));
#68278=CARTESIAN_POINT('',(-0.0324011113494634,-0.249999964237213,0.96));
#68279=CARTESIAN_POINT('Origin',(0.0375170443207026,-0.249999964237213,
1.));
#68280=CARTESIAN_POINT('',(0.0375170443207026,-0.249999964237213,1.));
#68281=CARTESIAN_POINT('',(0.0187585221603513,-0.249999964237213,1.));
#68282=CARTESIAN_POINT('',(0.0375170443207026,-0.249999964237213,0.96));
#68283=CARTESIAN_POINT('',(0.0375170443207026,-0.249999964237213,1.));
#68284=CARTESIAN_POINT('',(0.0375170443207026,-0.249999964237213,0.96));
#68285=CARTESIAN_POINT('Origin',(0.0375170443207026,-0.180081808567047,
1.));
#68286=CARTESIAN_POINT('',(0.0375170443207026,-0.0900409042835236,1.));
#68287=CARTESIAN_POINT('',(0.0375170443207026,-0.180081808567047,0.96));
#68288=CARTESIAN_POINT('Origin',(0.00255796648561957,-0.21504088640213,
0.96));
#68289=CARTESIAN_POINT('Ctrl Pts',(0.29092774130404,0.201568937301636,1.));
#68290=CARTESIAN_POINT('Ctrl Pts',(0.29092774130404,0.201568937301636,0.96));
#68291=CARTESIAN_POINT('Ctrl Pts',(0.25579807497561,0.201568937301636,1.));
#68292=CARTESIAN_POINT('Ctrl Pts',(0.25579807497561,0.201568937301636,0.96));
#68293=CARTESIAN_POINT('Ctrl Pts',(0.232605788484216,0.179058706760406,
1.));
#68294=CARTESIAN_POINT('Ctrl Pts',(0.232605788484216,0.179058706760406,
0.96));
#68295=CARTESIAN_POINT('',(0.29092774130404,0.201568937301636,1.));
#68296=CARTESIAN_POINT('',(0.232605788484216,0.179058706760406,1.));
#68297=CARTESIAN_POINT('Ctrl Pts',(0.29092774130404,0.201568937301636,1.));
#68298=CARTESIAN_POINT('Ctrl Pts',(0.25579807497561,0.201568937301636,1.));
#68299=CARTESIAN_POINT('Ctrl Pts',(0.232605788484216,0.179058706760406,
1.));
#68300=CARTESIAN_POINT('',(0.29092774130404,0.201568937301636,0.96));
#68301=CARTESIAN_POINT('',(0.29092774130404,0.201568937301636,1.));
#68302=CARTESIAN_POINT('',(0.232605788484216,0.179058706760406,0.96));
#68303=CARTESIAN_POINT('Ctrl Pts',(0.29092774130404,0.201568937301636,0.96));
#68304=CARTESIAN_POINT('Ctrl Pts',(0.25579807497561,0.201568937301636,0.96));
#68305=CARTESIAN_POINT('Ctrl Pts',(0.232605788484216,0.179058706760406,
0.96));
#68306=CARTESIAN_POINT('',(0.232605788484216,0.179058706760406,1.));
#68307=CARTESIAN_POINT('Ctrl Pts',(0.349079224839807,0.178547120094299,
1.));
#68308=CARTESIAN_POINT('Ctrl Pts',(0.349079224839807,0.178547120094299,
0.96));
#68309=CARTESIAN_POINT('Ctrl Pts',(0.325716230645776,0.201568937301636,
1.));
#68310=CARTESIAN_POINT('Ctrl Pts',(0.325716230645776,0.201568937301636,
0.96));
#68311=CARTESIAN_POINT('Ctrl Pts',(0.29092774130404,0.201568937301636,1.));
#68312=CARTESIAN_POINT('Ctrl Pts',(0.29092774130404,0.201568937301636,0.96));
#68313=CARTESIAN_POINT('',(0.349079224839807,0.178547120094299,1.));
#68314=CARTESIAN_POINT('Ctrl Pts',(0.349079224839807,0.178547120094299,
1.));
#68315=CARTESIAN_POINT('Ctrl Pts',(0.325716230645776,0.201568937301636,
1.));
#68316=CARTESIAN_POINT('Ctrl Pts',(0.29092774130404,0.201568937301636,1.));
#68317=CARTESIAN_POINT('',(0.349079224839807,0.178547120094299,0.96));
#68318=CARTESIAN_POINT('',(0.349079224839807,0.178547120094299,1.));
#68319=CARTESIAN_POINT('Ctrl Pts',(0.349079224839807,0.178547120094299,
0.96));
#68320=CARTESIAN_POINT('Ctrl Pts',(0.325716230645776,0.201568937301636,
0.96));
#68321=CARTESIAN_POINT('Ctrl Pts',(0.29092774130404,0.201568937301636,0.96));
#68322=CARTESIAN_POINT('Ctrl Pts',(0.372442099824548,0.121759927272797,
1.));
#68323=CARTESIAN_POINT('Ctrl Pts',(0.372442099824548,0.121759927272797,
0.96));
#68324=CARTESIAN_POINT('Ctrl Pts',(0.372442099824548,0.15552527308464,1.));
#68325=CARTESIAN_POINT('Ctrl Pts',(0.372442099824548,0.15552527308464,0.96));
#68326=CARTESIAN_POINT('Ctrl Pts',(0.349079224839807,0.178547120094299,
1.));
#68327=CARTESIAN_POINT('Ctrl Pts',(0.349079224839807,0.178547120094299,
0.96));
#68328=CARTESIAN_POINT('',(0.372442099824548,0.121759927272797,1.));
#68329=CARTESIAN_POINT('Ctrl Pts',(0.372442099824548,0.121759927272797,
1.));
#68330=CARTESIAN_POINT('Ctrl Pts',(0.372442099824548,0.15552527308464,1.));
#68331=CARTESIAN_POINT('Ctrl Pts',(0.349079224839807,0.178547120094299,
1.));
#68332=CARTESIAN_POINT('',(0.372442099824548,0.121759927272797,0.96));
#68333=CARTESIAN_POINT('',(0.372442099824548,0.121759927272797,1.));
#68334=CARTESIAN_POINT('Ctrl Pts',(0.372442099824548,0.121759927272797,
0.96));
#68335=CARTESIAN_POINT('Ctrl Pts',(0.372442099824548,0.15552527308464,0.96));
#68336=CARTESIAN_POINT('Ctrl Pts',(0.349079224839807,0.178547120094299,
0.96));
#68337=CARTESIAN_POINT('Ctrl Pts',(0.349761340394616,0.0670191407203674,
1.));
#68338=CARTESIAN_POINT('Ctrl Pts',(0.349761340394616,0.0670191407203674,
0.96));
#68339=CARTESIAN_POINT('Ctrl Pts',(0.372442099824548,0.0893588423728943,
1.));
#68340=CARTESIAN_POINT('Ctrl Pts',(0.372442099824548,0.0893588423728943,
0.96));
#68341=CARTESIAN_POINT('Ctrl Pts',(0.372442099824548,0.121759927272797,
1.));
#68342=CARTESIAN_POINT('Ctrl Pts',(0.372442099824548,0.121759927272797,
0.96));
#68343=CARTESIAN_POINT('',(0.349761340394616,0.0670191407203674,1.));
#68344=CARTESIAN_POINT('Ctrl Pts',(0.349761340394616,0.0670191407203674,
1.));
#68345=CARTESIAN_POINT('Ctrl Pts',(0.372442099824548,0.0893588423728943,
1.));
#68346=CARTESIAN_POINT('Ctrl Pts',(0.372442099824548,0.121759927272797,
1.));
#68347=CARTESIAN_POINT('',(0.349761340394616,0.0670191407203674,0.96));
#68348=CARTESIAN_POINT('',(0.349761340394616,0.0670191407203674,1.));
#68349=CARTESIAN_POINT('Ctrl Pts',(0.349761340394616,0.0670191407203674,
0.96));
#68350=CARTESIAN_POINT('Ctrl Pts',(0.372442099824548,0.0893588423728943,
0.96));
#68351=CARTESIAN_POINT('Ctrl Pts',(0.372442099824548,0.121759927272797,
0.96));
#68352=CARTESIAN_POINT('Ctrl Pts',(0.29160985685885,0.0446794390678406,
1.));
#68353=CARTESIAN_POINT('Ctrl Pts',(0.29160985685885,0.0446794390678406,
0.96));
#68354=CARTESIAN_POINT('Ctrl Pts',(0.327080580964685,0.0446794390678406,
1.));
#68355=CARTESIAN_POINT('Ctrl Pts',(0.327080580964685,0.0446794390678406,
0.96));
#68356=CARTESIAN_POINT('Ctrl Pts',(0.349761340394616,0.0670191407203674,
1.));
#68357=CARTESIAN_POINT('Ctrl Pts',(0.349761340394616,0.0670191407203674,
0.96));
#68358=CARTESIAN_POINT('',(0.29160985685885,0.0446794390678406,1.));
#68359=CARTESIAN_POINT('Ctrl Pts',(0.29160985685885,0.0446794390678406,
1.));
#68360=CARTESIAN_POINT('Ctrl Pts',(0.327080580964685,0.0446794390678406,
1.));
#68361=CARTESIAN_POINT('Ctrl Pts',(0.349761340394616,0.0670191407203674,
1.));
#68362=CARTESIAN_POINT('',(0.29160985685885,0.0446794390678406,0.96));
#68363=CARTESIAN_POINT('',(0.29160985685885,0.0446794390678406,1.));
#68364=CARTESIAN_POINT('Ctrl Pts',(0.29160985685885,0.0446794390678406,
0.96));
#68365=CARTESIAN_POINT('Ctrl Pts',(0.327080580964685,0.0446794390678406,
0.96));
#68366=CARTESIAN_POINT('Ctrl Pts',(0.349761340394616,0.0670191407203674,
0.96));
#68367=CARTESIAN_POINT('Ctrl Pts',(0.232264730706811,0.0671896696090698,
1.));
#68368=CARTESIAN_POINT('Ctrl Pts',(0.232264730706811,0.0671896696090698,
0.96));
#68369=CARTESIAN_POINT('Ctrl Pts',(0.2551159594208,0.0446794390678406,1.));
#68370=CARTESIAN_POINT('Ctrl Pts',(0.2551159594208,0.0446794390678406,0.96));
#68371=CARTESIAN_POINT('Ctrl Pts',(0.29160985685885,0.0446794390678406,
1.));
#68372=CARTESIAN_POINT('Ctrl Pts',(0.29160985685885,0.0446794390678406,
0.96));
#68373=CARTESIAN_POINT('',(0.232264730706811,0.0671896696090698,1.));
#68374=CARTESIAN_POINT('Ctrl Pts',(0.232264730706811,0.0671896696090698,
1.));
#68375=CARTESIAN_POINT('Ctrl Pts',(0.2551159594208,0.0446794390678406,1.));
#68376=CARTESIAN_POINT('Ctrl Pts',(0.29160985685885,0.0446794390678406,
1.));
#68377=CARTESIAN_POINT('',(0.232264730706811,0.0671896696090698,0.96));
#68378=CARTESIAN_POINT('',(0.232264730706811,0.0671896696090698,1.));
#68379=CARTESIAN_POINT('Ctrl Pts',(0.232264730706811,0.0671896696090698,
0.96));
#68380=CARTESIAN_POINT('Ctrl Pts',(0.2551159594208,0.0446794390678406,0.96));
#68381=CARTESIAN_POINT('Ctrl Pts',(0.29160985685885,0.0446794390678406,
0.96));
#68382=CARTESIAN_POINT('Ctrl Pts',(0.209413382783532,0.125170594453812,
1.));
#68383=CARTESIAN_POINT('Ctrl Pts',(0.209413382783532,0.125170594453812,
0.96));
#68384=CARTESIAN_POINT('Ctrl Pts',(0.209413382783532,0.0896999001502991,
1.));
#68385=CARTESIAN_POINT('Ctrl Pts',(0.209413382783532,0.0896999001502991,
0.96));
#68386=CARTESIAN_POINT('Ctrl Pts',(0.232264730706811,0.0671896696090698,
1.));
#68387=CARTESIAN_POINT('Ctrl Pts',(0.232264730706811,0.0671896696090698,
0.96));
#68388=CARTESIAN_POINT('',(0.209413382783532,0.125170594453812,1.));
#68389=CARTESIAN_POINT('Ctrl Pts',(0.209413382783532,0.125170594453812,
1.));
#68390=CARTESIAN_POINT('Ctrl Pts',(0.209413382783532,0.0896999001502991,
1.));
#68391=CARTESIAN_POINT('Ctrl Pts',(0.232264730706811,0.0671896696090698,
1.));
#68392=CARTESIAN_POINT('',(0.209413382783532,0.125170594453812,0.96));
#68393=CARTESIAN_POINT('',(0.209413382783532,0.125170594453812,1.));
#68394=CARTESIAN_POINT('Ctrl Pts',(0.209413382783532,0.125170594453812,
0.96));
#68395=CARTESIAN_POINT('Ctrl Pts',(0.209413382783532,0.0896999001502991,
0.96));
#68396=CARTESIAN_POINT('Ctrl Pts',(0.232264730706811,0.0671896696090698,
0.96));
#68397=CARTESIAN_POINT('Ctrl Pts',(0.232605788484216,0.179058706760406,
1.));
#68398=CARTESIAN_POINT('Ctrl Pts',(0.232605788484216,0.179058706760406,
0.96));
#68399=CARTESIAN_POINT('Ctrl Pts',(0.209413382783532,0.156548476219177,
1.));
#68400=CARTESIAN_POINT('Ctrl Pts',(0.209413382783532,0.156548476219177,
0.96));
#68401=CARTESIAN_POINT('Ctrl Pts',(0.209413382783532,0.125170594453812,
1.));
#68402=CARTESIAN_POINT('Ctrl Pts',(0.209413382783532,0.125170594453812,
0.96));
#68403=CARTESIAN_POINT('Ctrl Pts',(0.232605788484216,0.179058706760406,
1.));
#68404=CARTESIAN_POINT('Ctrl Pts',(0.209413382783532,0.156548476219177,
1.));
#68405=CARTESIAN_POINT('Ctrl Pts',(0.209413382783532,0.125170594453812,
1.));
#68406=CARTESIAN_POINT('Ctrl Pts',(0.232605788484216,0.179058706760406,
0.96));
#68407=CARTESIAN_POINT('Ctrl Pts',(0.209413382783532,0.156548476219177,
0.96));
#68408=CARTESIAN_POINT('Ctrl Pts',(0.209413382783532,0.125170594453812,
0.96));
#68409=CARTESIAN_POINT('Ctrl Pts',(0.289904567971826,-0.00545700788497927,
1.));
#68410=CARTESIAN_POINT('Ctrl Pts',(0.289904567971826,-0.00545700788497927,
0.96));
#68411=CARTESIAN_POINT('Ctrl Pts',(0.246589395776391,-0.00545700788497927,
1.));
#68412=CARTESIAN_POINT('Ctrl Pts',(0.246589395776391,-0.00545700788497927,
0.96));
#68413=CARTESIAN_POINT('Ctrl Pts',(0.218110534921289,-0.0341063976287842,
1.));
#68414=CARTESIAN_POINT('Ctrl Pts',(0.218110534921289,-0.0341063976287842,
0.96));
#68415=CARTESIAN_POINT('',(0.289904567971826,-0.00545700788497927,1.));
#68416=CARTESIAN_POINT('',(0.218110534921289,-0.0341063976287842,1.));
#68417=CARTESIAN_POINT('Ctrl Pts',(0.289904567971826,-0.00545700788497927,
1.));
#68418=CARTESIAN_POINT('Ctrl Pts',(0.246589395776391,-0.00545700788497927,
1.));
#68419=CARTESIAN_POINT('Ctrl Pts',(0.218110534921289,-0.0341063976287842,
1.));
#68420=CARTESIAN_POINT('',(0.289904567971826,-0.00545700788497927,0.96));
#68421=CARTESIAN_POINT('',(0.289904567971826,-0.00545700788497927,1.));
#68422=CARTESIAN_POINT('',(0.218110534921289,-0.0341063976287842,0.96));
#68423=CARTESIAN_POINT('Ctrl Pts',(0.289904567971826,-0.00545700788497927,
0.96));
#68424=CARTESIAN_POINT('Ctrl Pts',(0.246589395776391,-0.00545700788497927,
0.96));
#68425=CARTESIAN_POINT('Ctrl Pts',(0.218110534921289,-0.0341063976287842,
0.96));
#68426=CARTESIAN_POINT('',(0.218110534921289,-0.0341063976287842,1.));
#68427=CARTESIAN_POINT('Ctrl Pts',(0.363744947686791,-0.034447455406189,
1.));
#68428=CARTESIAN_POINT('Ctrl Pts',(0.363744947686791,-0.034447455406189,
0.96));
#68429=CARTESIAN_POINT('Ctrl Pts',(0.334242913499475,-0.00545700788497927,
1.));
#68430=CARTESIAN_POINT('Ctrl Pts',(0.334242913499475,-0.00545700788497927,
0.96));
#68431=CARTESIAN_POINT('Ctrl Pts',(0.289904567971826,-0.00545700788497927,
1.));
#68432=CARTESIAN_POINT('Ctrl Pts',(0.289904567971826,-0.00545700788497927,
0.96));
#68433=CARTESIAN_POINT('',(0.363744947686791,-0.034447455406189,1.));
#68434=CARTESIAN_POINT('Ctrl Pts',(0.363744947686791,-0.034447455406189,
1.));
#68435=CARTESIAN_POINT('Ctrl Pts',(0.334242913499475,-0.00545700788497927,
1.));
#68436=CARTESIAN_POINT('Ctrl Pts',(0.289904567971826,-0.00545700788497927,
1.));
#68437=CARTESIAN_POINT('',(0.363744947686791,-0.034447455406189,0.96));
#68438=CARTESIAN_POINT('',(0.363744947686791,-0.034447455406189,1.));
#68439=CARTESIAN_POINT('Ctrl Pts',(0.363744947686791,-0.034447455406189,
0.96));
#68440=CARTESIAN_POINT('Ctrl Pts',(0.334242913499475,-0.00545700788497927,
0.96));
#68441=CARTESIAN_POINT('Ctrl Pts',(0.289904567971826,-0.00545700788497927,
0.96));
#68442=CARTESIAN_POINT('Ctrl Pts',(0.393246981874108,-0.107776248455048,
1.));
#68443=CARTESIAN_POINT('Ctrl Pts',(0.393246981874108,-0.107776248455048,
0.96));
#68444=CARTESIAN_POINT('Ctrl Pts',(0.393246981874108,-0.0634379029273987,
1.));
#68445=CARTESIAN_POINT('Ctrl Pts',(0.393246981874108,-0.0634379029273987,
0.96));
#68446=CARTESIAN_POINT('Ctrl Pts',(0.363744947686791,-0.034447455406189,
1.));
#68447=CARTESIAN_POINT('Ctrl Pts',(0.363744947686791,-0.034447455406189,
0.96));
#68448=CARTESIAN_POINT('',(0.393246981874108,-0.107776248455048,1.));
#68449=CARTESIAN_POINT('Ctrl Pts',(0.393246981874108,-0.107776248455048,
1.));
#68450=CARTESIAN_POINT('Ctrl Pts',(0.393246981874108,-0.0634379029273987,
1.));
#68451=CARTESIAN_POINT('Ctrl Pts',(0.363744947686791,-0.034447455406189,
1.));
#68452=CARTESIAN_POINT('',(0.393246981874108,-0.107776248455048,0.96));
#68453=CARTESIAN_POINT('',(0.393246981874108,-0.107776248455048,1.));
#68454=CARTESIAN_POINT('Ctrl Pts',(0.393246981874108,-0.107776248455048,
0.96));
#68455=CARTESIAN_POINT('Ctrl Pts',(0.393246981874108,-0.0634379029273987,
0.96));
#68456=CARTESIAN_POINT('Ctrl Pts',(0.363744947686791,-0.034447455406189,
0.96));
#68457=CARTESIAN_POINT('Ctrl Pts',(0.364597532525659,-0.179740750789642,
1.));
#68458=CARTESIAN_POINT('Ctrl Pts',(0.364597532525659,-0.179740750789642,
0.96));
#68459=CARTESIAN_POINT('Ctrl Pts',(0.393246981874108,-0.151432418823242,
1.));
#68460=CARTESIAN_POINT('Ctrl Pts',(0.393246981874108,-0.151432418823242,
0.96));
#68461=CARTESIAN_POINT('Ctrl Pts',(0.393246981874108,-0.107776248455048,
1.));
#68462=CARTESIAN_POINT('Ctrl Pts',(0.393246981874108,-0.107776248455048,
0.96));
#68463=CARTESIAN_POINT('',(0.364597532525659,-0.179740750789642,1.));
#68464=CARTESIAN_POINT('Ctrl Pts',(0.364597532525659,-0.179740750789642,
1.));
#68465=CARTESIAN_POINT('Ctrl Pts',(0.393246981874108,-0.151432418823242,
1.));
#68466=CARTESIAN_POINT('Ctrl Pts',(0.393246981874108,-0.107776248455048,
1.));
#68467=CARTESIAN_POINT('',(0.364597532525659,-0.179740750789642,0.96));
#68468=CARTESIAN_POINT('',(0.364597532525659,-0.179740750789642,1.));
#68469=CARTESIAN_POINT('Ctrl Pts',(0.364597532525659,-0.179740750789642,
0.96));
#68470=CARTESIAN_POINT('Ctrl Pts',(0.393246981874108,-0.151432418823242,
0.96));
#68471=CARTESIAN_POINT('Ctrl Pts',(0.393246981874108,-0.107776248455048,
0.96));
#68472=CARTESIAN_POINT('Ctrl Pts',(0.291950914636254,-0.208049082756043,
1.));
#68473=CARTESIAN_POINT('Ctrl Pts',(0.291950914636254,-0.208049082756043,
0.96));
#68474=CARTESIAN_POINT('Ctrl Pts',(0.335948202386498,-0.208049082756043,
1.));
#68475=CARTESIAN_POINT('Ctrl Pts',(0.335948202386498,-0.208049082756043,
0.96));
#68476=CARTESIAN_POINT('Ctrl Pts',(0.364597532525659,-0.179740750789642,
1.));
#68477=CARTESIAN_POINT('Ctrl Pts',(0.364597532525659,-0.179740750789642,
0.96));
#68478=CARTESIAN_POINT('',(0.291950914636254,-0.208049082756043,1.));
#68479=CARTESIAN_POINT('Ctrl Pts',(0.291950914636254,-0.208049082756043,
1.));
#68480=CARTESIAN_POINT('Ctrl Pts',(0.335948202386498,-0.208049082756043,
1.));
#68481=CARTESIAN_POINT('Ctrl Pts',(0.364597532525659,-0.179740750789642,
1.));
#68482=CARTESIAN_POINT('',(0.291950914636254,-0.208049082756043,0.96));
#68483=CARTESIAN_POINT('',(0.291950914636254,-0.208049082756043,1.));
#68484=CARTESIAN_POINT('Ctrl Pts',(0.291950914636254,-0.208049082756043,
0.96));
#68485=CARTESIAN_POINT('Ctrl Pts',(0.335948202386498,-0.208049082756043,
0.96));
#68486=CARTESIAN_POINT('Ctrl Pts',(0.364597532525659,-0.179740750789642,
0.96));
#68487=CARTESIAN_POINT('Ctrl Pts',(0.239086005464196,-0.194577062129974,
1.));
#68488=CARTESIAN_POINT('Ctrl Pts',(0.239086005464196,-0.194577062129974,
0.96));
#68489=CARTESIAN_POINT('Ctrl Pts',(0.263642642274499,-0.208049082756043,
1.));
#68490=CARTESIAN_POINT('Ctrl Pts',(0.263642642274499,-0.208049082756043,
0.96));
#68491=CARTESIAN_POINT('Ctrl Pts',(0.291950914636254,-0.208049082756043,
1.));
#68492=CARTESIAN_POINT('Ctrl Pts',(0.291950914636254,-0.208049082756043,
0.96));
#68493=CARTESIAN_POINT('',(0.239086005464196,-0.194577062129974,1.));
#68494=CARTESIAN_POINT('Ctrl Pts',(0.239086005464196,-0.194577062129974,
1.));
#68495=CARTESIAN_POINT('Ctrl Pts',(0.263642642274499,-0.208049082756043,
1.));
#68496=CARTESIAN_POINT('Ctrl Pts',(0.291950914636254,-0.208049082756043,
1.));
#68497=CARTESIAN_POINT('',(0.239086005464196,-0.194577062129974,0.96));
#68498=CARTESIAN_POINT('',(0.239086005464196,-0.194577062129974,1.));
#68499=CARTESIAN_POINT('Ctrl Pts',(0.239086005464196,-0.194577062129974,
0.96));
#68500=CARTESIAN_POINT('Ctrl Pts',(0.263642642274499,-0.208049082756043,
0.96));
#68501=CARTESIAN_POINT('Ctrl Pts',(0.291950914636254,-0.208049082756043,
0.96));
#68502=CARTESIAN_POINT('Ctrl Pts',(0.202080580964685,-0.156548404693604,
1.));
#68503=CARTESIAN_POINT('Ctrl Pts',(0.202080580964685,-0.156548404693604,
0.96));
#68504=CARTESIAN_POINT('Ctrl Pts',(0.214529368653893,-0.181104981899261,
1.));
#68505=CARTESIAN_POINT('Ctrl Pts',(0.214529368653893,-0.181104981899261,
0.96));
#68506=CARTESIAN_POINT('Ctrl Pts',(0.239086005464196,-0.194577062129974,
1.));
#68507=CARTESIAN_POINT('Ctrl Pts',(0.239086005464196,-0.194577062129974,
0.96));
#68508=CARTESIAN_POINT('',(0.202080580964685,-0.156548404693604,1.));
#68509=CARTESIAN_POINT('Ctrl Pts',(0.202080580964685,-0.156548404693604,
1.));
#68510=CARTESIAN_POINT('Ctrl Pts',(0.214529368653893,-0.181104981899261,
1.));
#68511=CARTESIAN_POINT('Ctrl Pts',(0.239086005464196,-0.194577062129974,
1.));
#68512=CARTESIAN_POINT('',(0.202080580964685,-0.156548404693604,0.96));
#68513=CARTESIAN_POINT('',(0.202080580964685,-0.156548404693604,1.));
#68514=CARTESIAN_POINT('Ctrl Pts',(0.202080580964685,-0.156548404693604,
0.96));
#68515=CARTESIAN_POINT('Ctrl Pts',(0.214529368653893,-0.181104981899261,
0.96));
#68516=CARTESIAN_POINT('Ctrl Pts',(0.239086005464196,-0.194577062129974,
0.96));
#68517=CARTESIAN_POINT('Ctrl Pts',(0.189631674066186,-0.105729842185974,
1.));
#68518=CARTESIAN_POINT('Ctrl Pts',(0.189631674066186,-0.105729842185974,
0.96));
#68519=CARTESIAN_POINT('Ctrl Pts',(0.189631674066186,-0.131991767883301,
1.));
#68520=CARTESIAN_POINT('Ctrl Pts',(0.189631674066186,-0.131991767883301,
0.96));
#68521=CARTESIAN_POINT('Ctrl Pts',(0.202080580964685,-0.156548404693604,
1.));
#68522=CARTESIAN_POINT('Ctrl Pts',(0.202080580964685,-0.156548404693604,
0.96));
#68523=CARTESIAN_POINT('',(0.189631674066186,-0.105729842185974,1.));
#68524=CARTESIAN_POINT('Ctrl Pts',(0.189631674066186,-0.105729842185974,
1.));
#68525=CARTESIAN_POINT('Ctrl Pts',(0.189631674066186,-0.131991767883301,
1.));
#68526=CARTESIAN_POINT('Ctrl Pts',(0.202080580964685,-0.156548404693604,
1.));
#68527=CARTESIAN_POINT('',(0.189631674066186,-0.105729842185974,0.96));
#68528=CARTESIAN_POINT('',(0.189631674066186,-0.105729842185974,1.));
#68529=CARTESIAN_POINT('Ctrl Pts',(0.189631674066186,-0.105729842185974,
0.96));
#68530=CARTESIAN_POINT('Ctrl Pts',(0.189631674066186,-0.131991767883301,
0.96));
#68531=CARTESIAN_POINT('Ctrl Pts',(0.202080580964685,-0.156548404693604,
0.96));
#68532=CARTESIAN_POINT('Ctrl Pts',(0.218110534921289,-0.0341063976287842,
1.));
#68533=CARTESIAN_POINT('Ctrl Pts',(0.218110534921289,-0.0341063976287842,
0.96));
#68534=CARTESIAN_POINT('Ctrl Pts',(0.189631674066186,-0.0627557873725891,
1.));
#68535=CARTESIAN_POINT('Ctrl Pts',(0.189631674066186,-0.0627557873725891,
0.96));
#68536=CARTESIAN_POINT('Ctrl Pts',(0.189631674066186,-0.105729842185974,
1.));
#68537=CARTESIAN_POINT('Ctrl Pts',(0.189631674066186,-0.105729842185974,
0.96));
#68538=CARTESIAN_POINT('Ctrl Pts',(0.218110534921289,-0.0341063976287842,
1.));
#68539=CARTESIAN_POINT('Ctrl Pts',(0.189631674066186,-0.0627557873725891,
1.));
#68540=CARTESIAN_POINT('Ctrl Pts',(0.189631674066186,-0.105729842185974,
1.));
#68541=CARTESIAN_POINT('Ctrl Pts',(0.218110534921289,-0.0341063976287842,
0.96));
#68542=CARTESIAN_POINT('Ctrl Pts',(0.189631674066186,-0.0627557873725891,
0.96));
#68543=CARTESIAN_POINT('Ctrl Pts',(0.189631674066186,-0.105729842185974,
0.96));
#68544=CARTESIAN_POINT('Ctrl Pts',(0.171896312013268,-0.214699828624725,
1.));
#68545=CARTESIAN_POINT('Ctrl Pts',(0.171896312013268,-0.214699828624725,
0.96));
#68546=CARTESIAN_POINT('Ctrl Pts',(0.126534793153405,-0.170873069763184,
1.));
#68547=CARTESIAN_POINT('Ctrl Pts',(0.126534793153405,-0.170873069763184,
0.96));
#68548=CARTESIAN_POINT('Ctrl Pts',(0.126534793153405,-0.105388784408569,
1.));
#68549=CARTESIAN_POINT('Ctrl Pts',(0.126534793153405,-0.105388784408569,
0.96));
#68550=CARTESIAN_POINT('',(0.171896312013268,-0.214699828624725,1.));
#68551=CARTESIAN_POINT('',(0.126534793153405,-0.105388784408569,1.));
#68552=CARTESIAN_POINT('Ctrl Pts',(0.171896312013268,-0.214699828624725,
1.));
#68553=CARTESIAN_POINT('Ctrl Pts',(0.126534793153405,-0.170873069763184,
1.));
#68554=CARTESIAN_POINT('Ctrl Pts',(0.126534793153405,-0.105388784408569,
1.));
#68555=CARTESIAN_POINT('',(0.171896312013268,-0.214699828624725,0.96));
#68556=CARTESIAN_POINT('',(0.171896312013268,-0.214699828624725,1.));
#68557=CARTESIAN_POINT('',(0.126534793153405,-0.105388784408569,0.96));
#68558=CARTESIAN_POINT('Ctrl Pts',(0.171896312013268,-0.214699828624725,
0.96));
#68559=CARTESIAN_POINT('Ctrl Pts',(0.126534793153405,-0.170873069763184,
0.96));
#68560=CARTESIAN_POINT('Ctrl Pts',(0.126534793153405,-0.105388784408569,
0.96));
#68561=CARTESIAN_POINT('',(0.126534793153405,-0.105388784408569,1.));
#68562=CARTESIAN_POINT('Ctrl Pts',(0.291268799081445,-0.258526587486267,
1.));
#68563=CARTESIAN_POINT('Ctrl Pts',(0.291268799081445,-0.258526587486267,
0.96));
#68564=CARTESIAN_POINT('Ctrl Pts',(0.217257830873132,-0.258526587486267,
1.));
#68565=CARTESIAN_POINT('Ctrl Pts',(0.217257830873132,-0.258526587486267,
0.96));
#68566=CARTESIAN_POINT('Ctrl Pts',(0.171896312013268,-0.214699828624725,
1.));
#68567=CARTESIAN_POINT('Ctrl Pts',(0.171896312013268,-0.214699828624725,
0.96));
#68568=CARTESIAN_POINT('',(0.291268799081445,-0.258526587486267,1.));
#68569=CARTESIAN_POINT('Ctrl Pts',(0.291268799081445,-0.258526587486267,
1.));
#68570=CARTESIAN_POINT('Ctrl Pts',(0.217257830873132,-0.258526587486267,
1.));
#68571=CARTESIAN_POINT('Ctrl Pts',(0.171896312013268,-0.214699828624725,
1.));
#68572=CARTESIAN_POINT('',(0.291268799081445,-0.258526587486267,0.96));
#68573=CARTESIAN_POINT('',(0.291268799081445,-0.258526587486267,1.));
#68574=CARTESIAN_POINT('Ctrl Pts',(0.291268799081445,-0.258526587486267,
0.96));
#68575=CARTESIAN_POINT('Ctrl Pts',(0.217257830873132,-0.258526587486267,
0.96));
#68576=CARTESIAN_POINT('Ctrl Pts',(0.171896312013268,-0.214699828624725,
0.96));
#68577=CARTESIAN_POINT('Ctrl Pts',(0.410641286149621,-0.214870357513428,
1.));
#68578=CARTESIAN_POINT('Ctrl Pts',(0.410641286149621,-0.214870357513428,
0.96));
#68579=CARTESIAN_POINT('Ctrl Pts',(0.365279767289758,-0.258526587486267,
1.));
#68580=CARTESIAN_POINT('Ctrl Pts',(0.365279767289758,-0.258526587486267,
0.96));
#68581=CARTESIAN_POINT('Ctrl Pts',(0.291268799081445,-0.258526587486267,
1.));
#68582=CARTESIAN_POINT('Ctrl Pts',(0.291268799081445,-0.258526587486267,
0.96));
#68583=CARTESIAN_POINT('',(0.410641286149621,-0.214870357513428,1.));
#68584=CARTESIAN_POINT('Ctrl Pts',(0.410641286149621,-0.214870357513428,
1.));
#68585=CARTESIAN_POINT('Ctrl Pts',(0.365279767289758,-0.258526587486267,
1.));
#68586=CARTESIAN_POINT('Ctrl Pts',(0.291268799081445,-0.258526587486267,
1.));
#68587=CARTESIAN_POINT('',(0.410641286149621,-0.214870357513428,0.96));
#68588=CARTESIAN_POINT('',(0.410641286149621,-0.214870357513428,1.));
#68589=CARTESIAN_POINT('Ctrl Pts',(0.410641286149621,-0.214870357513428,
0.96));
#68590=CARTESIAN_POINT('Ctrl Pts',(0.365279767289758,-0.258526587486267,
0.96));
#68591=CARTESIAN_POINT('Ctrl Pts',(0.291268799081445,-0.258526587486267,
0.96));
#68592=CARTESIAN_POINT('Ctrl Pts',(0.456002805009484,-0.107094132900238,
1.));
#68593=CARTESIAN_POINT('Ctrl Pts',(0.456002805009484,-0.107094132900238,
0.96));
#68594=CARTESIAN_POINT('Ctrl Pts',(0.456002805009484,-0.171214127540588,
1.));
#68595=CARTESIAN_POINT('Ctrl Pts',(0.456002805009484,-0.171214127540588,
0.96));
#68596=CARTESIAN_POINT('Ctrl Pts',(0.410641286149621,-0.214870357513428,
1.));
#68597=CARTESIAN_POINT('Ctrl Pts',(0.410641286149621,-0.214870357513428,
0.96));
#68598=CARTESIAN_POINT('',(0.456002805009484,-0.107094132900238,1.));
#68599=CARTESIAN_POINT('Ctrl Pts',(0.456002805009484,-0.107094132900238,
1.));
#68600=CARTESIAN_POINT('Ctrl Pts',(0.456002805009484,-0.171214127540588,
1.));
#68601=CARTESIAN_POINT('Ctrl Pts',(0.410641286149621,-0.214870357513428,
1.));
#68602=CARTESIAN_POINT('',(0.456002805009484,-0.107094132900238,0.96));
#68603=CARTESIAN_POINT('',(0.456002805009484,-0.107094132900238,1.));
#68604=CARTESIAN_POINT('Ctrl Pts',(0.456002805009484,-0.107094132900238,
0.96));
#68605=CARTESIAN_POINT('Ctrl Pts',(0.456002805009484,-0.171214127540588,
0.96));
#68606=CARTESIAN_POINT('Ctrl Pts',(0.410641286149621,-0.214870357513428,
0.96));
#68607=CARTESIAN_POINT('Ctrl Pts',(0.431957814469934,-0.0272850632667542,
1.));
#68608=CARTESIAN_POINT('Ctrl Pts',(0.431957814469934,-0.0272850632667542,
0.96));
#68609=CARTESIAN_POINT('Ctrl Pts',(0.456002805009484,-0.0607093811035156,
1.));
#68610=CARTESIAN_POINT('Ctrl Pts',(0.456002805009484,-0.0607093811035156,
0.96));
#68611=CARTESIAN_POINT('Ctrl Pts',(0.456002805009484,-0.107094132900238,
1.));
#68612=CARTESIAN_POINT('Ctrl Pts',(0.456002805009484,-0.107094132900238,
0.96));
#68613=CARTESIAN_POINT('',(0.431957814469934,-0.0272850632667542,1.));
#68614=CARTESIAN_POINT('Ctrl Pts',(0.431957814469934,-0.0272850632667542,
1.));
#68615=CARTESIAN_POINT('Ctrl Pts',(0.456002805009484,-0.0607093811035156,
1.));
#68616=CARTESIAN_POINT('Ctrl Pts',(0.456002805009484,-0.107094132900238,
1.));
#68617=CARTESIAN_POINT('',(0.431957814469934,-0.0272850632667542,0.96));
#68618=CARTESIAN_POINT('',(0.431957814469934,-0.0272850632667542,1.));
#68619=CARTESIAN_POINT('Ctrl Pts',(0.431957814469934,-0.0272850632667542,
0.96));
#68620=CARTESIAN_POINT('Ctrl Pts',(0.456002805009484,-0.0607093811035156,
0.96));
#68621=CARTESIAN_POINT('Ctrl Pts',(0.456002805009484,-0.107094132900238,
0.96));
#68622=CARTESIAN_POINT('Ctrl Pts',(0.36186907030642,0.021146035194397,1.));
#68623=CARTESIAN_POINT('Ctrl Pts',(0.36186907030642,0.021146035194397,0.96));
#68624=CARTESIAN_POINT('Ctrl Pts',(0.407912704721093,0.00613919496536253,
1.));
#68625=CARTESIAN_POINT('Ctrl Pts',(0.407912704721093,0.00613919496536253,
0.96));
#68626=CARTESIAN_POINT('Ctrl Pts',(0.431957814469934,-0.0272850632667542,
1.));
#68627=CARTESIAN_POINT('Ctrl Pts',(0.431957814469934,-0.0272850632667542,
0.96));
#68628=CARTESIAN_POINT('',(0.36186907030642,0.021146035194397,1.));
#68629=CARTESIAN_POINT('Ctrl Pts',(0.36186907030642,0.021146035194397,1.));
#68630=CARTESIAN_POINT('Ctrl Pts',(0.407912704721093,0.00613919496536253,
1.));
#68631=CARTESIAN_POINT('Ctrl Pts',(0.431957814469934,-0.0272850632667542,
1.));
#68632=CARTESIAN_POINT('',(0.36186907030642,0.021146035194397,0.96));
#68633=CARTESIAN_POINT('',(0.36186907030642,0.021146035194397,1.));
#68634=CARTESIAN_POINT('Ctrl Pts',(0.36186907030642,0.021146035194397,0.96));
#68635=CARTESIAN_POINT('Ctrl Pts',(0.407912704721093,0.00613919496536253,
0.96));
#68636=CARTESIAN_POINT('Ctrl Pts',(0.431957814469934,-0.0272850632667542,
0.96));
#68637=CARTESIAN_POINT('Ctrl Pts',(0.417291972413659,0.0608799815177917,
1.));
#68638=CARTESIAN_POINT('Ctrl Pts',(0.417291972413659,0.0608799815177917,
0.96));
#68639=CARTESIAN_POINT('Ctrl Pts',(0.399045083299279,0.0351296424865722,
1.));
#68640=CARTESIAN_POINT('Ctrl Pts',(0.399045083299279,0.0351296424865722,
0.96));
#68641=CARTESIAN_POINT('Ctrl Pts',(0.36186907030642,0.021146035194397,1.));
#68642=CARTESIAN_POINT('Ctrl Pts',(0.36186907030642,0.021146035194397,0.96));
#68643=CARTESIAN_POINT('',(0.417291972413659,0.0608799815177917,1.));
#68644=CARTESIAN_POINT('Ctrl Pts',(0.417291972413659,0.0608799815177917,
1.));
#68645=CARTESIAN_POINT('Ctrl Pts',(0.399045083299279,0.0351296424865722,
1.));
#68646=CARTESIAN_POINT('Ctrl Pts',(0.36186907030642,0.021146035194397,1.));
#68647=CARTESIAN_POINT('',(0.417291972413659,0.0608799815177917,0.96));
#68648=CARTESIAN_POINT('',(0.417291972413659,0.0608799815177917,1.));
#68649=CARTESIAN_POINT('Ctrl Pts',(0.417291972413659,0.0608799815177917,
0.96));
#68650=CARTESIAN_POINT('Ctrl Pts',(0.399045083299279,0.0351296424865722,
0.96));
#68651=CARTESIAN_POINT('Ctrl Pts',(0.36186907030642,0.021146035194397,0.96));
#68652=CARTESIAN_POINT('Ctrl Pts',(0.435538980737329,0.121418869495392,
1.));
#68653=CARTESIAN_POINT('Ctrl Pts',(0.435538980737329,0.121418869495392,
0.96));
#68654=CARTESIAN_POINT('Ctrl Pts',(0.435538980737329,0.0866303205490112,
1.));
#68655=CARTESIAN_POINT('Ctrl Pts',(0.435538980737329,0.0866303205490112,
0.96));
#68656=CARTESIAN_POINT('Ctrl Pts',(0.417291972413659,0.0608799815177917,
1.));
#68657=CARTESIAN_POINT('Ctrl Pts',(0.417291972413659,0.0608799815177917,
0.96));
#68658=CARTESIAN_POINT('',(0.435538980737329,0.121418869495392,1.));
#68659=CARTESIAN_POINT('Ctrl Pts',(0.435538980737329,0.121418869495392,
1.));
#68660=CARTESIAN_POINT('Ctrl Pts',(0.435538980737329,0.0866303205490112,
1.));
#68661=CARTESIAN_POINT('Ctrl Pts',(0.417291972413659,0.0608799815177917,
1.));
#68662=CARTESIAN_POINT('',(0.435538980737329,0.121418869495392,0.96));
#68663=CARTESIAN_POINT('',(0.435538980737329,0.121418869495392,1.));
#68664=CARTESIAN_POINT('Ctrl Pts',(0.435538980737329,0.121418869495392,
0.96));
#68665=CARTESIAN_POINT('Ctrl Pts',(0.435538980737329,0.0866303205490112,
0.96));
#68666=CARTESIAN_POINT('Ctrl Pts',(0.417291972413659,0.0608799815177917,
0.96));
#68667=CARTESIAN_POINT('Ctrl Pts',(0.395634386315942,0.214017784595489,
1.));
#68668=CARTESIAN_POINT('Ctrl Pts',(0.395634386315942,0.214017784595489,
0.96));
#68669=CARTESIAN_POINT('Ctrl Pts',(0.435538980737329,0.175989127159119,
1.));
#68670=CARTESIAN_POINT('Ctrl Pts',(0.435538980737329,0.175989127159119,
0.96));
#68671=CARTESIAN_POINT('Ctrl Pts',(0.435538980737329,0.121418869495392,
1.));
#68672=CARTESIAN_POINT('Ctrl Pts',(0.435538980737329,0.121418869495392,
0.96));
#68673=CARTESIAN_POINT('',(0.395634386315942,0.214017784595489,1.));
#68674=CARTESIAN_POINT('Ctrl Pts',(0.395634386315942,0.214017784595489,
1.));
#68675=CARTESIAN_POINT('Ctrl Pts',(0.435538980737329,0.175989127159119,
1.));
#68676=CARTESIAN_POINT('Ctrl Pts',(0.435538980737329,0.121418869495392,
1.));
#68677=CARTESIAN_POINT('',(0.395634386315942,0.214017784595489,0.96));
#68678=CARTESIAN_POINT('',(0.395634386315942,0.214017784595489,1.));
#68679=CARTESIAN_POINT('Ctrl Pts',(0.395634386315942,0.214017784595489,
0.96));
#68680=CARTESIAN_POINT('Ctrl Pts',(0.435538980737329,0.175989127159119,
0.96));
#68681=CARTESIAN_POINT('Ctrl Pts',(0.435538980737329,0.121418869495392,
0.96));
#68682=CARTESIAN_POINT('Ctrl Pts',(0.29024562574923,0.252046382427216,1.));
#68683=CARTESIAN_POINT('Ctrl Pts',(0.29024562574923,0.252046382427216,0.96));
#68684=CARTESIAN_POINT('Ctrl Pts',(0.355729911103845,0.252046382427216,
1.));
#68685=CARTESIAN_POINT('Ctrl Pts',(0.355729911103845,0.252046382427216,
0.96));
#68686=CARTESIAN_POINT('Ctrl Pts',(0.395634386315942,0.214017784595489,
1.));
#68687=CARTESIAN_POINT('Ctrl Pts',(0.395634386315942,0.214017784595489,
0.96));
#68688=CARTESIAN_POINT('',(0.29024562574923,0.252046382427216,1.));
#68689=CARTESIAN_POINT('Ctrl Pts',(0.29024562574923,0.252046382427216,1.));
#68690=CARTESIAN_POINT('Ctrl Pts',(0.355729911103845,0.252046382427216,
1.));
#68691=CARTESIAN_POINT('Ctrl Pts',(0.395634386315942,0.214017784595489,
1.));
#68692=CARTESIAN_POINT('',(0.29024562574923,0.252046382427216,0.96));
#68693=CARTESIAN_POINT('',(0.29024562574923,0.252046382427216,1.));
#68694=CARTESIAN_POINT('Ctrl Pts',(0.29024562574923,0.252046382427216,0.96));
#68695=CARTESIAN_POINT('Ctrl Pts',(0.355729911103845,0.252046382427216,
0.96));
#68696=CARTESIAN_POINT('Ctrl Pts',(0.395634386315942,0.214017784595489,
0.96));
#68697=CARTESIAN_POINT('Ctrl Pts',(0.185880038514733,0.214870429039001,
1.));
#68698=CARTESIAN_POINT('Ctrl Pts',(0.185880038514733,0.214870429039001,
0.96));
#68699=CARTESIAN_POINT('Ctrl Pts',(0.225102398172021,0.252046382427216,
1.));
#68700=CARTESIAN_POINT('Ctrl Pts',(0.225102398172021,0.252046382427216,
0.96));
#68701=CARTESIAN_POINT('Ctrl Pts',(0.29024562574923,0.252046382427216,1.));
#68702=CARTESIAN_POINT('Ctrl Pts',(0.29024562574923,0.252046382427216,0.96));
#68703=CARTESIAN_POINT('',(0.185880038514733,0.214870429039001,1.));
#68704=CARTESIAN_POINT('Ctrl Pts',(0.185880038514733,0.214870429039001,
1.));
#68705=CARTESIAN_POINT('Ctrl Pts',(0.225102398172021,0.252046382427216,
1.));
#68706=CARTESIAN_POINT('Ctrl Pts',(0.29024562574923,0.252046382427216,1.));
#68707=CARTESIAN_POINT('',(0.185880038514733,0.214870429039001,0.96));
#68708=CARTESIAN_POINT('',(0.185880038514733,0.214870429039001,1.));
#68709=CARTESIAN_POINT('Ctrl Pts',(0.185880038514733,0.214870429039001,
0.96));
#68710=CARTESIAN_POINT('Ctrl Pts',(0.225102398172021,0.252046382427216,
0.96));
#68711=CARTESIAN_POINT('Ctrl Pts',(0.29024562574923,0.252046382427216,0.96));
#68712=CARTESIAN_POINT('Ctrl Pts',(0.146657559648156,0.123124188184738,
1.));
#68713=CARTESIAN_POINT('Ctrl Pts',(0.146657559648156,0.123124188184738,
0.96));
#68714=CARTESIAN_POINT('Ctrl Pts',(0.146657559648156,0.177694445848465,
1.));
#68715=CARTESIAN_POINT('Ctrl Pts',(0.146657559648156,0.177694445848465,
0.96));
#68716=CARTESIAN_POINT('Ctrl Pts',(0.185880038514733,0.214870429039001,
1.));
#68717=CARTESIAN_POINT('Ctrl Pts',(0.185880038514733,0.214870429039001,
0.96));
#68718=CARTESIAN_POINT('',(0.146657559648156,0.123124188184738,1.));
#68719=CARTESIAN_POINT('Ctrl Pts',(0.146657559648156,0.123124188184738,
1.));
#68720=CARTESIAN_POINT('Ctrl Pts',(0.146657559648156,0.177694445848465,
1.));
#68721=CARTESIAN_POINT('Ctrl Pts',(0.185880038514733,0.214870429039001,
1.));
#68722=CARTESIAN_POINT('',(0.146657559648156,0.123124188184738,0.96));
#68723=CARTESIAN_POINT('',(0.146657559648156,0.123124188184738,1.));
#68724=CARTESIAN_POINT('Ctrl Pts',(0.146657559648156,0.123124188184738,
0.96));
#68725=CARTESIAN_POINT('Ctrl Pts',(0.146657559648156,0.177694445848465,
0.96));
#68726=CARTESIAN_POINT('Ctrl Pts',(0.185880038514733,0.214870429039001,
0.96));
#68727=CARTESIAN_POINT('Ctrl Pts',(0.165075037255883,0.0610505104064941,
1.));
#68728=CARTESIAN_POINT('Ctrl Pts',(0.165075037255883,0.0610505104064941,
0.96));
#68729=CARTESIAN_POINT('Ctrl Pts',(0.146657559648156,0.0869714081287384,
1.));
#68730=CARTESIAN_POINT('Ctrl Pts',(0.146657559648156,0.0869714081287384,
0.96));
#68731=CARTESIAN_POINT('Ctrl Pts',(0.146657559648156,0.123124188184738,
1.));
#68732=CARTESIAN_POINT('Ctrl Pts',(0.146657559648156,0.123124188184738,
0.96));
#68733=CARTESIAN_POINT('',(0.165075037255883,0.0610505104064941,1.));
#68734=CARTESIAN_POINT('Ctrl Pts',(0.165075037255883,0.0610505104064941,
1.));
#68735=CARTESIAN_POINT('Ctrl Pts',(0.146657559648156,0.0869714081287384,
1.));
#68736=CARTESIAN_POINT('Ctrl Pts',(0.146657559648156,0.123124188184738,
1.));
#68737=CARTESIAN_POINT('',(0.165075037255883,0.0610505104064941,0.96));
#68738=CARTESIAN_POINT('',(0.165075037255883,0.0610505104064941,1.));
#68739=CARTESIAN_POINT('Ctrl Pts',(0.165075037255883,0.0610505104064941,
0.96));
#68740=CARTESIAN_POINT('Ctrl Pts',(0.146657559648156,0.0869714081287384,
0.96));
#68741=CARTESIAN_POINT('Ctrl Pts',(0.146657559648156,0.123124188184738,
0.96));
#68742=CARTESIAN_POINT('Ctrl Pts',(0.221691701188684,0.021146035194397,
1.));
#68743=CARTESIAN_POINT('Ctrl Pts',(0.221691701188684,0.021146035194397,
0.96));
#68744=CARTESIAN_POINT('Ctrl Pts',(0.18349251486361,0.0351296424865722,
1.));
#68745=CARTESIAN_POINT('Ctrl Pts',(0.18349251486361,0.0351296424865722,
0.96));
#68746=CARTESIAN_POINT('Ctrl Pts',(0.165075037255883,0.0610505104064941,
1.));
#68747=CARTESIAN_POINT('Ctrl Pts',(0.165075037255883,0.0610505104064941,
0.96));
#68748=CARTESIAN_POINT('',(0.221691701188684,0.021146035194397,1.));
#68749=CARTESIAN_POINT('Ctrl Pts',(0.221691701188684,0.021146035194397,
1.));
#68750=CARTESIAN_POINT('Ctrl Pts',(0.18349251486361,0.0351296424865722,
1.));
#68751=CARTESIAN_POINT('Ctrl Pts',(0.165075037255883,0.0610505104064941,
1.));
#68752=CARTESIAN_POINT('',(0.221691701188684,0.021146035194397,0.96));
#68753=CARTESIAN_POINT('',(0.221691701188684,0.021146035194397,1.));
#68754=CARTESIAN_POINT('Ctrl Pts',(0.221691701188684,0.021146035194397,
0.96));
#68755=CARTESIAN_POINT('Ctrl Pts',(0.18349251486361,0.0351296424865722,
0.96));
#68756=CARTESIAN_POINT('Ctrl Pts',(0.165075037255883,0.0610505104064941,
0.96));
#68757=CARTESIAN_POINT('Ctrl Pts',(0.151262018457055,-0.0237038969993592,
1.));
#68758=CARTESIAN_POINT('Ctrl Pts',(0.151262018457055,-0.0237038969993592,
0.96));
#68759=CARTESIAN_POINT('Ctrl Pts',(0.175989124551415,0.00920877456665037,
1.));
#68760=CARTESIAN_POINT('Ctrl Pts',(0.175989124551415,0.00920877456665037,
0.96));
#68761=CARTESIAN_POINT('Ctrl Pts',(0.221691701188684,0.021146035194397,
1.));
#68762=CARTESIAN_POINT('Ctrl Pts',(0.221691701188684,0.021146035194397,
0.96));
#68763=CARTESIAN_POINT('',(0.151262018457055,-0.0237038969993592,1.));
#68764=CARTESIAN_POINT('Ctrl Pts',(0.151262018457055,-0.0237038969993592,
1.));
#68765=CARTESIAN_POINT('Ctrl Pts',(0.175989124551415,0.00920877456665037,
1.));
#68766=CARTESIAN_POINT('Ctrl Pts',(0.221691701188684,0.021146035194397,
1.));
#68767=CARTESIAN_POINT('',(0.151262018457055,-0.0237038969993592,0.96));
#68768=CARTESIAN_POINT('',(0.151262018457055,-0.0237038969993592,1.));
#68769=CARTESIAN_POINT('Ctrl Pts',(0.151262018457055,-0.0237038969993592,
0.96));
#68770=CARTESIAN_POINT('Ctrl Pts',(0.175989124551415,0.00920877456665037,
0.96));
#68771=CARTESIAN_POINT('Ctrl Pts',(0.221691701188684,0.021146035194397,
0.96));
#68772=CARTESIAN_POINT('Ctrl Pts',(0.126534793153405,-0.105388784408569,
1.));
#68773=CARTESIAN_POINT('Ctrl Pts',(0.126534793153405,-0.105388784408569,
0.96));
#68774=CARTESIAN_POINT('Ctrl Pts',(0.126534793153405,-0.0566166281700134,
1.));
#68775=CARTESIAN_POINT('Ctrl Pts',(0.126534793153405,-0.0566166281700134,
0.96));
#68776=CARTESIAN_POINT('Ctrl Pts',(0.151262018457055,-0.0237038969993592,
1.));
#68777=CARTESIAN_POINT('Ctrl Pts',(0.151262018457055,-0.0237038969993592,
0.96));
#68778=CARTESIAN_POINT('Ctrl Pts',(0.126534793153405,-0.105388784408569,
1.));
#68779=CARTESIAN_POINT('Ctrl Pts',(0.126534793153405,-0.0566166281700134,
1.));
#68780=CARTESIAN_POINT('Ctrl Pts',(0.151262018457055,-0.0237038969993592,
1.));
#68781=CARTESIAN_POINT('Ctrl Pts',(0.126534793153405,-0.105388784408569,
0.96));
#68782=CARTESIAN_POINT('Ctrl Pts',(0.126534793153405,-0.0566166281700134,
0.96));
#68783=CARTESIAN_POINT('Ctrl Pts',(0.151262018457055,-0.0237038969993592,
0.96));
#68784=CARTESIAN_POINT('Origin',(0.291268799081445,-0.00324010252952578,
0.96));
#68785=CARTESIAN_POINT('Origin',(0.,0.,1.));
#68786=CARTESIAN_POINT('Origin',(0.,0.,1.));
#68787=CARTESIAN_POINT('Origin',(0.,0.,1.));
#68788=CARTESIAN_POINT('Origin',(0.,0.,1.));
#68789=CARTESIAN_POINT('Origin',(1.87869726832665E-16,-4.25270154953079E-17,
-0.0599999999999998));
#68790=CARTESIAN_POINT('Ctrl Pts',(0.564220937616133,0.373642629516334,
-0.0599999999999999));
#68791=CARTESIAN_POINT('Ctrl Pts',(0.554999902806836,0.390417265728263,
-0.06));
#68792=CARTESIAN_POINT('Ctrl Pts',(0.545076539942756,0.406773487088272,
-0.0599999999999998));
#68793=CARTESIAN_POINT('Ctrl Pts',(0.534474770141273,0.422664239409727,
-0.0599999999999997));
#68794=CARTESIAN_POINT('Ctrl Pts',(0.518439430377503,0.446699246521537,
-0.0599999999999996));
#68795=CARTESIAN_POINT('Ctrl Pts',(0.500853434182984,0.469670265905156,
-0.0600000000000004));
#68796=CARTESIAN_POINT('Ctrl Pts',(0.4818657358897,0.49147811068534,-0.0600000000000005));
#68797=CARTESIAN_POINT('Ctrl Pts',(0.475405651424852,0.498897678718297,
-0.0600000000000005));
#68798=CARTESIAN_POINT('Ctrl Pts',(0.46878307560605,0.506182489986116,-0.0600000000000007));
#68799=CARTESIAN_POINT('Ctrl Pts',(0.462003176886937,0.513328228135021,
-0.0600000000000008));
#68800=CARTESIAN_POINT('Ctrl Pts',(0.456208383549552,0.519435705183202,
-0.0600000000000009));
#68801=CARTESIAN_POINT('Ctrl Pts',(0.45029960428802,0.525440374114255,-0.06));
#68802=CARTESIAN_POINT('Ctrl Pts',(0.444288945418066,0.531331357726455,
-0.06));
#68803=CARTESIAN_POINT('Ctrl Pts',(0.419805435115621,0.555327388957209,
-0.0600000000000001));
#68804=CARTESIAN_POINT('Ctrl Pts',(0.393598452075611,0.577478902722108,
-0.0600000000000002));
#68805=CARTESIAN_POINT('Ctrl Pts',(0.365904584686211,0.597621427333679,
-0.0600000000000005));
#68806=CARTESIAN_POINT('Ctrl Pts',(0.355326984662029,0.605314811786729,
-0.0600000000000006));
#68807=CARTESIAN_POINT('Ctrl Pts',(0.344531984117663,0.612714798138308,
-0.0599999999999995));
#68808=CARTESIAN_POINT('Ctrl Pts',(0.33353112873019,0.619810852933279,-0.0599999999999995));
#68809=CARTESIAN_POINT('Ctrl Pts',(0.326461355727503,0.624371179821331,
-0.0599999999999995));
#68810=CARTESIAN_POINT('Ctrl Pts',(0.319305261975003,0.628806725629368,
-0.0600000000000005));
#68811=CARTESIAN_POINT('Ctrl Pts',(0.312069750178058,0.633112118087385,
-0.0600000000000004));
#68812=CARTESIAN_POINT('Ctrl Pts',(0.301086781020382,0.639647383857811,
-0.0600000000000004));
#68813=CARTESIAN_POINT('Ctrl Pts',(0.289938770881977,0.645872277100329,
-0.0599999999999999));
#68814=CARTESIAN_POINT('Ctrl Pts',(0.278638203951252,0.651779354610587,
-0.0599999999999998));
#68815=CARTESIAN_POINT('Ctrl Pts',(0.248488006514047,0.667539586314266,
-0.0599999999999998));
#68816=CARTESIAN_POINT('Ctrl Pts',(0.217254479547028,0.681040528771996,
-0.0600000000000008));
#68817=CARTESIAN_POINT('Ctrl Pts',(0.185214713477108,0.692275549523078,
-0.0600000000000008));
#68818=CARTESIAN_POINT('Ctrl Pts',(0.163435758734888,0.699912528143077,
-0.0600000000000008));
#68819=CARTESIAN_POINT('Ctrl Pts',(0.141283364114538,0.706501731226335,
-0.0600000000000006));
#68820=CARTESIAN_POINT('Ctrl Pts',(0.118836930295083,0.71202966809404,-0.0600000000000005));
#68821=CARTESIAN_POINT('Ctrl Pts',(0.101600177236571,0.716274604437963,
-0.0600000000000005));
#68822=CARTESIAN_POINT('Ctrl Pts',(0.0841898961222066,0.719893553076916,
-0.06));
#68823=CARTESIAN_POINT('Ctrl Pts',(0.066640643957318,0.722876340867067,
-0.0599999999999999));
#68824=CARTESIAN_POINT('Ctrl Pts',(0.0571917300477745,0.724482341212539,
-0.0599999999999999));
#68825=CARTESIAN_POINT('Ctrl Pts',(0.0476983252949259,0.725904193801259,
-0.0600000000000005));
#68826=CARTESIAN_POINT('Ctrl Pts',(0.0381937449141578,0.727136847640426,
-0.0600000000000004));
#68827=CARTESIAN_POINT('Ctrl Pts',(0.00262667264075837,0.731749559241503,
-0.0600000000000002));
#68828=CARTESIAN_POINT('Ctrl Pts',(-0.0331646305896378,0.733731011574693,
-0.06));
#68829=CARTESIAN_POINT('Ctrl Pts',(-0.0688851945093288,0.733054681865674,
-0.0599999999999999));
#68830=CARTESIAN_POINT('Ctrl Pts',(-0.100011196056527,0.732465345157086,
-0.0599999999999997));
#68831=CARTESIAN_POINT('Ctrl Pts',(-0.131084581015127,0.72985747823783,
-0.0600000000000001));
#68832=CARTESIAN_POINT('Ctrl Pts',(-0.161929396660483,0.725302428734695,
-0.0600000000000001));
#68833=CARTESIAN_POINT('Ctrl Pts',(-0.179884268169555,0.722650919013043,
-0.06));
#68834=CARTESIAN_POINT('Ctrl Pts',(-0.197761783439131,0.719338985371272,
-0.0600000000000004));
#68835=CARTESIAN_POINT('Ctrl Pts',(-0.215527051730703,0.715375574961876,
-0.0600000000000004));
#68836=CARTESIAN_POINT('Ctrl Pts',(-0.225777172638808,0.713088785072865,
-0.0600000000000004));
#68837=CARTESIAN_POINT('Ctrl Pts',(-0.235995395902091,0.710583358306907,
-0.0600000000000004));
#68838=CARTESIAN_POINT('Ctrl Pts',(-0.246143283251969,0.707869589519532,
-0.0600000000000003));
#68839=CARTESIAN_POINT('Ctrl Pts',(-0.280845547615335,0.698589439017892,
-0.0600000000000001));
#68840=CARTESIAN_POINT('Ctrl Pts',(-0.314784451676007,0.686866611325189,
-0.0600000000000013));
#68841=CARTESIAN_POINT('Ctrl Pts',(-0.347701200929954,0.672822676723929,
-0.0600000000000011));
#68842=CARTESIAN_POINT('Ctrl Pts',(-0.374455811938238,0.661407819066396,
-0.0600000000000009));
#68843=CARTESIAN_POINT('Ctrl Pts',(-0.400535660286788,0.648458458483484,
-0.0600000000000007));
#68844=CARTESIAN_POINT('Ctrl Pts',(-0.425798867633714,0.634014708143998,
-0.0600000000000007));
#68845=CARTESIAN_POINT('Ctrl Pts',(-0.440419184632767,0.625655824581885,
-0.0600000000000007));
#68846=CARTESIAN_POINT('Ctrl Pts',(-0.454765899488343,0.616796030051311,
-0.0600000000000007));
#68847=CARTESIAN_POINT('Ctrl Pts',(-0.468820720454222,0.607454901453629,
-0.0600000000000006));
#68848=CARTESIAN_POINT('Ctrl Pts',(-0.476475383557125,0.602367451916581,
-0.0600000000000006));
#68849=CARTESIAN_POINT('Ctrl Pts',(-0.484043443552845,0.597137188854445,
-0.0600000000000003));
#68850=CARTESIAN_POINT('Ctrl Pts',(-0.491521770420875,0.591767005742375,
-0.0600000000000004));
#68851=CARTESIAN_POINT('Ctrl Pts',(-0.497516875552335,0.58746192348264,
-0.0600000000000004));
#68852=CARTESIAN_POINT('Ctrl Pts',(-0.503453507366844,0.583067338002368,
-0.0600000000000002));
#68853=CARTESIAN_POINT('Ctrl Pts',(-0.509319859107208,0.578592953790838,
-0.0600000000000003));
#68854=CARTESIAN_POINT('Ctrl Pts',(-0.538206295805245,0.5565606887632,-0.0600000000000005));
#68855=CARTESIAN_POINT('Ctrl Pts',(-0.565457889840676,0.532549689384572,
-0.0600000000000006));
#68856=CARTESIAN_POINT('Ctrl Pts',(-0.590916862149367,0.506792766445156,
-0.0600000000000004));
#68857=CARTESIAN_POINT('Ctrl Pts',(-0.616583471997437,0.480825775949348,
-0.0600000000000003));
#68858=CARTESIAN_POINT('Ctrl Pts',(-0.640429074795126,0.45308353546991,
-0.0600000000000004));
#68859=CARTESIAN_POINT('Ctrl Pts',(-0.662265722032779,0.423759522339067,
-0.0600000000000004));
#68860=CARTESIAN_POINT('Ctrl Pts',(-0.676018847392074,0.405290715097877,
-0.0600000000000004));
#68861=CARTESIAN_POINT('Ctrl Pts',(-0.688974507348362,0.386193601376564,
-0.0600000000000005));
#68862=CARTESIAN_POINT('Ctrl Pts',(-0.701077753000059,0.366509473613423,
-0.0600000000000005));
#68863=CARTESIAN_POINT('',(0.7911,-9.68818082805471E-17,-0.0600000000000001));
#68864=CARTESIAN_POINT('Origin',(0.,0.,-0.0600000000000001));
#68865=CARTESIAN_POINT('',(-0.724732793080687,-0.317244732932517,-0.0599999999999999));
#68866=CARTESIAN_POINT('Origin',(0.,0.,-0.0600000000000001));
#68867=CARTESIAN_POINT('Ctrl Pts',(-0.724732793080687,-0.317244732932517,
-0.0599999999999997));
#68868=CARTESIAN_POINT('Ctrl Pts',(-0.714450380759048,-0.336937903853692,
-0.0599999999999997));
#68869=CARTESIAN_POINT('Ctrl Pts',(-0.703349785215869,-0.356164574870145,
-0.0599999999999997));
#68870=CARTESIAN_POINT('Ctrl Pts',(-0.69144548414381,-0.37486759263711,
-0.0599999999999997));
#68871=CARTESIAN_POINT('Ctrl Pts',(-0.674201669809379,-0.401959596099963,
-0.0599999999999997));
#68872=CARTESIAN_POINT('Ctrl Pts',(-0.655272167225403,-0.427953990204327,
-0.0600000000000001));
#68873=CARTESIAN_POINT('Ctrl Pts',(-0.634786796513414,-0.452716544678885,
-0.0599999999999998));
#68874=CARTESIAN_POINT('Ctrl Pts',(-0.625943879110367,-0.463405793459665,
-0.0599999999999997));
#68875=CARTESIAN_POINT('Ctrl Pts',(-0.616810792269047,-0.473865214589598,
-0.0599999999999995));
#68876=CARTESIAN_POINT('Ctrl Pts',(-0.607396992666966,-0.484082568711768,
-0.0599999999999995));
#68877=CARTESIAN_POINT('Ctrl Pts',(-0.600762905540228,-0.491282936290893,
-0.0599999999999995));
#68878=CARTESIAN_POINT('Ctrl Pts',(-0.59399520773963,-0.498356663864347,
-0.0599999999999999));
#68879=CARTESIAN_POINT('Ctrl Pts',(-0.587101581912719,-0.50529629740727,
-0.0599999999999999));
#68880=CARTESIAN_POINT('Ctrl Pts',(-0.561447885223103,-0.531121205593067,
-0.06));
#68881=CARTESIAN_POINT('Ctrl Pts',(-0.534036253371049,-0.555110192383224,
-0.0599999999999992));
#68882=CARTESIAN_POINT('Ctrl Pts',(-0.505053708225385,-0.577058137884389,
-0.0599999999999991));
#68883=CARTESIAN_POINT('Ctrl Pts',(-0.494424541121948,-0.585107409580043,
-0.0599999999999991));
#68884=CARTESIAN_POINT('Ctrl Pts',(-0.483583822744001,-0.592881716994318,
-0.0600000000000003));
#68885=CARTESIAN_POINT('Ctrl Pts',(-0.472540016063593,-0.60036928753405,
-0.0600000000000004));
#68886=CARTESIAN_POINT('Ctrl Pts',(-0.465321436044098,-0.605263399560527,
-0.0600000000000005));
#68887=CARTESIAN_POINT('Ctrl Pts',(-0.458016082683304,-0.610034988697207,
-0.0599999999999998));
#68888=CARTESIAN_POINT('Ctrl Pts',(-0.450626256800085,-0.614680536634416,
-0.0599999999999998));
#68889=CARTESIAN_POINT('Ctrl Pts',(-0.44377928707728,-0.618984822902397,
-0.0599999999999998));
#68890=CARTESIAN_POINT('Ctrl Pts',(-0.436867759283859,-0.623175873324015,
-0.06));
#68891=CARTESIAN_POINT('Ctrl Pts',(-0.429895671529333,-0.627250594422087,
-0.06));
#68892=CARTESIAN_POINT('Ctrl Pts',(-0.424514176663148,-0.630395719876964,
-0.06));
#68893=CARTESIAN_POINT('Ctrl Pts',(-0.419096249028614,-0.633471758380428,
-0.0600000000000006));
#68894=CARTESIAN_POINT('Ctrl Pts',(-0.41364286935094,-0.636477760421398,
-0.0600000000000006));
#68895=CARTESIAN_POINT('Ctrl Pts',(-0.382437517006967,-0.653678718062254,
-0.0600000000000007));
#68896=CARTESIAN_POINT('Ctrl Pts',(-0.35007282615117,-0.668590450667035,
-0.0600000000000001));
#68897=CARTESIAN_POINT('Ctrl Pts',(-0.316814221808171,-0.681152839764513,
-0.0600000000000002));
#68898=CARTESIAN_POINT('Ctrl Pts',(-0.283852732529365,-0.69360300301497,
-0.0600000000000004));
#68899=CARTESIAN_POINT('Ctrl Pts',(-0.250011984261866,-0.703745755096182,
-0.0600000000000001));
#68900=CARTESIAN_POINT('Ctrl Pts',(-0.215543393032759,-0.711472512578678,
-0.0599999999999999));
#68901=CARTESIAN_POINT('Ctrl Pts',(-0.204674264783505,-0.713909024052846,
-0.0599999999999999));
#68902=CARTESIAN_POINT('Ctrl Pts',(-0.193742728782231,-0.716104914100372,
-0.0600000000000004));
#68903=CARTESIAN_POINT('Ctrl Pts',(-0.182756823721076,-0.718055695088162,
-0.0600000000000004));
#68904=CARTESIAN_POINT('Ctrl Pts',(-0.175918855215345,-0.719269921761507,
-0.0600000000000004));
#68905=CARTESIAN_POINT('Ctrl Pts',(-0.169063474904282,-0.720388450438065,
-0.0600000000000006));
#68906=CARTESIAN_POINT('Ctrl Pts',(-0.162200941898156,-0.72140941413215,
-0.0600000000000006));
#68907=CARTESIAN_POINT('Ctrl Pts',(-0.127449530315254,-0.726579506503682,
-0.0600000000000006));
#68908=CARTESIAN_POINT('Ctrl Pts',(-0.0924516067775416,-0.729263481555391,
-0.0600000000000014));
#68909=CARTESIAN_POINT('Ctrl Pts',(-0.0574594945934324,-0.72938133341839,
-0.0600000000000012));
#68910=CARTESIAN_POINT('Ctrl Pts',(-0.027630035940758,-0.729481797696052,
-0.060000000000001));
#68911=CARTESIAN_POINT('Ctrl Pts',(0.00219580972971492,-0.727716416426016,
-0.0600000000000007));
#68912=CARTESIAN_POINT('Ctrl Pts',(0.0318469521835107,-0.724114769434076,
-0.0600000000000006));
#68913=CARTESIAN_POINT('Ctrl Pts',(0.0479356243986104,-0.72216052035318,
-0.0600000000000005));
#68914=CARTESIAN_POINT('Ctrl Pts',(0.0639727227373624,-0.719665181752117,
-0.0599999999999997));
#68915=CARTESIAN_POINT('Ctrl Pts',(0.0799293665208594,-0.716630325957448,
-0.0599999999999997));
#68916=CARTESIAN_POINT('Ctrl Pts',(0.0871442683202932,-0.715258095880054,
-0.0599999999999997));
#68917=CARTESIAN_POINT('Ctrl Pts',(0.0943427028482492,-0.713775535082417,
-0.0600000000000005));
#68918=CARTESIAN_POINT('Ctrl Pts',(0.101521897140979,-0.712182649561427,
-0.0600000000000005));
#68919=CARTESIAN_POINT('Ctrl Pts',(0.108504253187729,-0.710633437575268,
-0.0600000000000005));
#68920=CARTESIAN_POINT('Ctrl Pts',(0.115459879835767,-0.708981734404333,
-0.0600000000000009));
#68921=CARTESIAN_POINT('Ctrl Pts',(0.122383960481882,-0.707228903035257,
-0.0600000000000009));
#68922=CARTESIAN_POINT('Ctrl Pts',(0.155299370056219,-0.698896365420998,
-0.0600000000000008));
#68923=CARTESIAN_POINT('Ctrl Pts',(0.187522320328344,-0.688278118088817,
-0.0599999999999995));
#68924=CARTESIAN_POINT('Ctrl Pts',(0.218802043739288,-0.675429950655413,
-0.0599999999999997));
#68925=CARTESIAN_POINT('Ctrl Pts',(0.241942213387686,-0.66592511040558,
-0.0599999999999999));
#68926=CARTESIAN_POINT('Ctrl Pts',(0.264566024515351,-0.65519881750284,
-0.06));
#68927=CARTESIAN_POINT('Ctrl Pts',(0.286562207485726,-0.643258021344417,
-0.0600000000000002));
#68928=CARTESIAN_POINT('Ctrl Pts',(0.300602246187078,-0.635636278953248,
-0.0600000000000002));
#68929=CARTESIAN_POINT('Ctrl Pts',(0.314386374989223,-0.62751943179706,
-0.0600000000000001));
#68930=CARTESIAN_POINT('Ctrl Pts',(0.327891021984824,-0.618923601513977,
-0.06));
#68931=CARTESIAN_POINT('Ctrl Pts',(0.335107601460311,-0.614330183232413,
-0.06));
#68932=CARTESIAN_POINT('Ctrl Pts',(0.342244337517139,-0.609599960851706,
-0.0600000000000004));
#68933=CARTESIAN_POINT('Ctrl Pts',(0.349297374951807,-0.604735234968208,
-0.0600000000000003));
#68934=CARTESIAN_POINT('Ctrl Pts',(0.354530483740722,-0.60112577733915,
-0.0600000000000003));
#68935=CARTESIAN_POINT('Ctrl Pts',(0.359715650922231,-0.597443457431399,
-0.0600000000000008));
#68936=CARTESIAN_POINT('Ctrl Pts',(0.364844366648222,-0.593694722470919,
-0.0600000000000007));
#68937=CARTESIAN_POINT('Ctrl Pts',(0.391762620975772,-0.574019348271211,
-0.0600000000000006));
#68938=CARTESIAN_POINT('Ctrl Pts',(0.417186617116553,-0.552477930138312,
-0.0600000000000008));
#68939=CARTESIAN_POINT('Ctrl Pts',(0.44093118569783,-0.529249758345641,
-0.0600000000000006));
#68940=CARTESIAN_POINT('Ctrl Pts',(0.464233432423963,-0.506454288794062,
-0.0600000000000004));
#68941=CARTESIAN_POINT('Ctrl Pts',(0.485918907142877,-0.482033324451575,
-0.0600000000000005));
#68942=CARTESIAN_POINT('Ctrl Pts',(0.50577214775514,-0.456128464695498,
-0.0600000000000006));
#68943=CARTESIAN_POINT('Ctrl Pts',(0.516780263536972,-0.441764880378141,
-0.0600000000000006));
#68944=CARTESIAN_POINT('Ctrl Pts',(0.527224294979779,-0.426944672942178,
-0.06));
#68945=CARTESIAN_POINT('Ctrl Pts',(0.5370608629359,-0.411689834101531,-0.0600000000000001));
#68946=CARTESIAN_POINT('Ctrl Pts',(-0.292601934307104,0.610169646934147,
-2.97494887079529));
#68947=CARTESIAN_POINT('Ctrl Pts',(-0.393827994997909,0.561627505729252,
-2.96966816631922));
#68948=CARTESIAN_POINT('Ctrl Pts',(-0.571555357247122,0.41324396405726,
-2.95910675736706));
#68949=CARTESIAN_POINT('Ctrl Pts',(-0.6994873117981,0.0901905791434185,
-2.94326464393882));
#68950=CARTESIAN_POINT('Ctrl Pts',(-0.657692280887251,-0.254657867677908,
-2.92742253051059));
#68951=CARTESIAN_POINT('Ctrl Pts',(-0.456327777700922,-0.537761889174431,
-2.91158041708236));
#68952=CARTESIAN_POINT('Ctrl Pts',(-0.14424191559841,-0.690367492084008,
-2.89573830365411));
#68953=CARTESIAN_POINT('Ctrl Pts',(0.202839712455166,-0.675480941669175,
-2.87989619022589));
#68954=CARTESIAN_POINT('Ctrl Pts',(0.500707301958,-0.496697430942489,-2.86405407679764));
#68955=CARTESIAN_POINT('Ctrl Pts',(0.677088347387025,-0.197403558953597,
-2.84821196336941));
#68956=CARTESIAN_POINT('Ctrl Pts',(0.689188274048217,0.149787622898873,
-2.83236984994118));
#68957=CARTESIAN_POINT('Ctrl Pts',(0.534070984426596,0.460635224458885,
-2.81652773651294));
#68958=CARTESIAN_POINT('Ctrl Pts',(0.249372597829536,0.659719708601146,
-2.80068562308471));
#68959=CARTESIAN_POINT('Ctrl Pts',(-0.095830858278809,0.69873681536456,
-2.78484350965647));
#68960=CARTESIAN_POINT('Ctrl Pts',(-0.417782948255712,0.568220153665686,
-2.76900139622824));
#68961=CARTESIAN_POINT('Ctrl Pts',(-0.638368754645892,0.299836710863442,
-2.7531592828));
#68962=CARTESIAN_POINT('Ctrl Pts',(-0.704067736716126,-0.0412958101518603,
-2.73731716937176));
#68963=CARTESIAN_POINT('Ctrl Pts',(-0.598939416511963,-0.372408780057021,
-2.72147505594353));
#68964=CARTESIAN_POINT('Ctrl Pts',(-0.348490978460388,-0.613164545241514,
-2.7056329425153));
#68965=CARTESIAN_POINT('Ctrl Pts',(-0.0134884969402019,-0.705148767075711,
-2.68979082908706));
#68966=CARTESIAN_POINT('Ctrl Pts',(0.324786686361382,-0.626043393699459,
-2.67394871565883));
#68967=CARTESIAN_POINT('Ctrl Pts',(0.584259176083316,-0.395041691351842,
-2.65810660223059));
#68968=CARTESIAN_POINT('Ctrl Pts',(0.701973402101012,-0.068191388181339,
-2.64226448880235));
#68969=CARTESIAN_POINT('Ctrl Pts',(0.649368470484853,0.275204128232534,
-2.62642237537412));
#68970=CARTESIAN_POINT('Ctrl Pts',(0.439207867209178,0.551827121547341,
-2.61058026194588));
#68971=CARTESIAN_POINT('Ctrl Pts',(0.122482665136422,0.69456081044579,-2.59473814851765));
#68972=CARTESIAN_POINT('Ctrl Pts',(-0.223960392743318,0.668773852033162,
-2.57889603508941));
#68973=CARTESIAN_POINT('Ctrl Pts',(-0.516064147577321,0.480722912143853,
-2.56305392166118));
#68974=CARTESIAN_POINT('Ctrl Pts',(-0.682955735366548,0.176034616500302,
-2.54721180823294));
#68975=CARTESIAN_POINT('Ctrl Pts',(-0.684142404452695,-0.171364795411006,
-2.53136969480471));
#68976=CARTESIAN_POINT('Ctrl Pts',(-0.519336234411588,-0.477186125430353,
-2.51552758137647));
#68977=CARTESIAN_POINT('Ctrl Pts',(-0.228523993923267,-0.667228226979231,
-2.49968546794824));
#68978=CARTESIAN_POINT('Ctrl Pts',(0.117734811948404,-0.69538136064443,
-2.48384335452));
#68979=CARTESIAN_POINT('Ctrl Pts',(0.435427729238652,-0.554814757632145,
-2.46800124109176));
#68980=CARTESIAN_POINT('Ctrl Pts',(0.647473219121237,-0.279633962881997,
-2.45215912766353));
#68981=CARTESIAN_POINT('Ctrl Pts',(0.702422880414448,0.0633941617704607,
-2.43631701423529));
#68982=CARTESIAN_POINT('Ctrl Pts',(0.586944327597745,0.391041019558242,
-2.42047490080706));
#68983=CARTESIAN_POINT('Ctrl Pts',(0.329056015185207,0.623809956274138,
-2.40463278737882));
#68984=CARTESIAN_POINT('Ctrl Pts',(-0.0086708539911011,0.705224459989427,
-2.38879067395059));
#68985=CARTESIAN_POINT('Ctrl Pts',(-0.344293921879448,0.615531004932474,
-2.37294856052235));
#68986=CARTESIAN_POINT('Ctrl Pts',(-0.5963812737897,0.376491831185336,-2.35710644709412));
#68987=CARTESIAN_POINT('Ctrl Pts',(-0.70376918857369,0.0461047924910424,
-2.34126433366588));
#68988=CARTESIAN_POINT('Ctrl Pts',(-0.640402235743698,-0.295468609383107,
-2.32542222023765));
#68989=CARTESIAN_POINT('Ctrl Pts',(-0.42165508048436,-0.565352735712883,
-2.30958010680941));
#68990=CARTESIAN_POINT('Ctrl Pts',(-0.100602142852268,-0.698065850425191,
-2.29373799338118));
#68991=CARTESIAN_POINT('Ctrl Pts',(0.244859799696957,-0.661407893185951,
-2.27789587995294));
#68992=CARTESIAN_POINT('Ctrl Pts',(0.530911635409909,-0.46427315027114,
-2.26205376652471));
#68993=CARTESIAN_POINT('Ctrl Pts',(0.688148871832329,-0.154492242110101,
-2.24621165309647));
#68994=CARTESIAN_POINT('Ctrl Pts',(0.678421183651292,0.192772975931516,
-2.23036953966824));
#68995=CARTESIAN_POINT('Ctrl Pts',(0.50408879085726,0.493265865034647,-2.21452742624));
#68996=CARTESIAN_POINT('Ctrl Pts',(0.207449800749737,0.674078113311214,
-2.19868531281176));
#68997=CARTESIAN_POINT('Ctrl Pts',(-0.13952254273371,0.691339412116387,
-2.18284319938353));
#68998=CARTESIAN_POINT('Ctrl Pts',(-0.45264266065732,0.540861668478527,
-2.1670010859553));
#68999=CARTESIAN_POINT('Ctrl Pts',(-0.655938508277729,0.259155158225147,
-2.15115897252706));
#69000=CARTESIAN_POINT('Ctrl Pts',(-0.700084602026596,-0.0854299284886501,
-2.13531685909882));
#69001=CARTESIAN_POINT('Ctrl Pts',(-0.574369815989129,-0.409287230630185,
-2.11947474567059));
#69002=CARTESIAN_POINT('Ctrl Pts',(-0.309296212482741,-0.633839550375444,
-2.10363263224235));
#69003=CARTESIAN_POINT('Ctrl Pts',(0.0308216451249593,-0.704603965975287,
-2.08779051881412));
#69004=CARTESIAN_POINT('Ctrl Pts',(0.363461275469507,-0.60441097269192,
-2.07194840538588));
#69005=CARTESIAN_POINT('Ctrl Pts',(0.607914632553942,-0.357570303860817,
-2.05610629195764));
#69006=CARTESIAN_POINT('Ctrl Pts',(0.704870224337332,-0.0239726827650286,
-2.04026417852942));
#69007=CARTESIAN_POINT('Ctrl Pts',(0.630803805217274,0.315441408188147,
-2.02442206510117));
#69008=CARTESIAN_POINT('Ctrl Pts',(0.403686041993089,0.578320241887024,
-2.00857995167294));
#69009=CARTESIAN_POINT('Ctrl Pts',(0.0786223075935471,0.700881769933403,
-1.9927378382447));
#69010=CARTESIAN_POINT('Ctrl Pts',(-0.265517484613883,0.653389002081171,
-1.97689572481647));
#69011=CARTESIAN_POINT('Ctrl Pts',(-0.545235014990942,0.44736506468894,
-1.96105361138823));
#69012=CARTESIAN_POINT('Ctrl Pts',(-0.692662677731179,0.132797355224364,
-1.94521149796));
#69013=CARTESIAN_POINT('Ctrl Pts',(-0.672030235315574,-0.213990853771854,
-1.92936938453176));
#69014=CARTESIAN_POINT('Ctrl Pts',(-0.488343718173467,-0.50885865974436,
-1.91352727110353));
#69015=CARTESIAN_POINT('Ctrl Pts',(-0.186170816147377,-0.680262559524874,
-1.8976851576753));
#69016=CARTESIAN_POINT('Ctrl Pts',(0.161172538892235,-0.686614983366474,
-1.88184304424706));
#69017=CARTESIAN_POINT('Ctrl Pts',(0.469410749818722,-0.526374648545063,
-1.86600093081882));
#69018=CARTESIAN_POINT('Ctrl Pts',(0.663756264470278,-0.238420519361853,
-1.85015881739059));
#69019=CARTESIAN_POINT('Ctrl Pts',(0.697055210292531,0.107381360022812,
-1.83431670396235));
#69020=CARTESIAN_POINT('Ctrl Pts',(0.561228294844321,0.427129399295399,
-1.81847459053412));
#69021=CARTESIAN_POINT('Ctrl Pts',(0.289231077053685,0.643243427282921,
-1.80263247710588));
#69022=CARTESIAN_POINT('Ctrl Pts',(-0.0529420095786137,0.703287897164517,
-1.78679036367765));
#69023=CARTESIAN_POINT('Ctrl Pts',(-0.382269825369864,0.592694274721806,
-1.77094825024941));
#69024=CARTESIAN_POINT('Ctrl Pts',(-0.618847866826519,0.338295788328172,
-1.75510613682118));
#69025=CARTESIAN_POINT('Ctrl Pts',(-0.705275422457957,0.00181690755493101,
-1.73926402339294));
#69026=CARTESIAN_POINT('Ctrl Pts',(-0.62058265434053,-0.335102807818698,
-1.72342190996471));
#69027=CARTESIAN_POINT('Ctrl Pts',(-0.385318490507109,-0.590716838721934,
-1.70757979653647));
#69028=CARTESIAN_POINT('Ctrl Pts',(-0.0565648575352245,-0.70300578914283,
-1.69173768310824));
#69029=CARTESIAN_POINT('Ctrl Pts',(0.285913054528226,-0.644725094847914,
-1.67589556968));
#69030=CARTESIAN_POINT('Ctrl Pts',(0.559020146487969,-0.430015346815531,
-1.66005345625177));
#69031=CARTESIAN_POINT('Ctrl Pts',(0.696492697099633,-0.110971372719233,
-1.64421134282353));
#69032=CARTESIAN_POINT('Ctrl Pts',(0.664975868496808,0.234997482950838,
-1.6283692293953));
#69033=CARTESIAN_POINT('Ctrl Pts',(0.472116559667202,0.523949116579385,
-1.61252711596706));
#69034=CARTESIAN_POINT('Ctrl Pts',(0.164708046420555,0.685775460424648,
-1.59668500253882));
#69035=CARTESIAN_POINT('Ctrl Pts',(-0.182663427862365,0.681212738282163,
-1.58084288911059));
#69036=CARTESIAN_POINT('Ctrl Pts',(-0.4857154435089,0.51136799920729,-1.56500077568235));
#69037=CARTESIAN_POINT('Ctrl Pts',(-0.670918770123565,0.217450515226326,
-1.54915866225412));
#69038=CARTESIAN_POINT('Ctrl Pts',(-0.693337695783756,-0.129226786238709,
-1.53331654882588));
#69039=CARTESIAN_POINT('Ctrl Pts',(-0.54753273728204,-0.444549912024228,
-1.51747443539765));
#69040=CARTESIAN_POINT('Ctrl Pts',(-0.268880416908177,-0.652012303625934,
-1.50163232196941));
#69041=CARTESIAN_POINT('Ctrl Pts',(0.0750101104497115,-0.701277552761128,
-1.48579020854118));
#69042=CARTESIAN_POINT('Ctrl Pts',(0.400701004053372,-0.580392477576107,
-1.46994809511294));
#69043=CARTESIAN_POINT('Ctrl Pts',(0.629170183477428,-0.318687312109054,
-1.45410598168471));
#69044=CARTESIAN_POINT('Ctrl Pts',(0.70498438292987,0.0203406612799057,
-1.43826386825647));
#69045=CARTESIAN_POINT('Ctrl Pts',(0.609748873285091,0.354433398826739,
-1.42242175482824));
#69046=CARTESIAN_POINT('Ctrl Pts',(0.366570558206358,0.602530288477345,
-1.4065796414));
#69047=CARTESIAN_POINT('Ctrl Pts',(0.034451567471494,0.704435811252572,
-1.39073752797176));
#69048=CARTESIAN_POINT('Ctrl Pts',(-0.306026375229727,0.63542472436951,
-1.37489541454353));
#69049=CARTESIAN_POINT('Ctrl Pts',(-0.57225342141949,0.412241124040289,
-1.35905330111529));
#69050=CARTESIAN_POINT('Ctrl Pts',(-0.699635148998229,0.089035840887468,
-1.34321118768706));
#69051=CARTESIAN_POINT('Ctrl Pts',(-0.657265047163405,-0.255772126029403,
-1.32736907425882));
#69052=CARTESIAN_POINT('Ctrl Pts',(-0.455423334553543,-0.538522338460017,
-1.31152696083059));
#69053=CARTESIAN_POINT('Ctrl Pts',(-0.143082679303674,-0.690611373754874,
-1.29568484740235));
#69054=CARTESIAN_POINT('Ctrl Pts',(0.203973994150782,-0.675138009881304,
-1.27984273397412));
#69055=CARTESIAN_POINT('Ctrl Pts',(0.501540645971156,-0.495856534811379,
-1.26400062054588));
#69056=CARTESIAN_POINT('Ctrl Pts',(0.677418954516088,-0.196265847101944,
-1.24815850711765));
#69057=CARTESIAN_POINT('Ctrl Pts',(0.688935728376574,0.150944641649023,
-1.23231639368941));
#69058=CARTESIAN_POINT('Ctrl Pts',(0.533296663357694,0.461531571539655,
-1.21647428026118));
#69059=CARTESIAN_POINT('Ctrl Pts',(0.248264321922183,0.660137522897185,
-1.20063216683294));
#69060=CARTESIAN_POINT('Ctrl Pts',(-0.0970041624297474,0.698574917347893,
-1.1847900534047));
#69061=CARTESIAN_POINT('Ctrl Pts',(-0.418736616528254,0.567517725410213,
-1.16894793997647));
#69062=CARTESIAN_POINT('Ctrl Pts',(-0.638871392465658,0.298764232406262,
-1.15310582654823));
#69063=CARTESIAN_POINT('Ctrl Pts',(-0.703997393063064,-0.0424781501094858,
-1.13726371312));
#69064=CARTESIAN_POINT('Ctrl Pts',(-0.598313157002194,-0.373414098333714,
-1.12142159969176));
#69065=CARTESIAN_POINT('Ctrl Pts',(-0.347460752777172,-0.613748929087322,
-1.10557948626353));
#69066=CARTESIAN_POINT('Ctrl Pts',(-0.0123042673209635,-0.705170424565585,
-1.08973737283529));
#69067=CARTESIAN_POINT('Ctrl Pts',(0.32583759114047,-0.625497071836542,
-1.07389525940706));
#69068=CARTESIAN_POINT('Ctrl Pts',(0.584921776088787,-0.394059942817653,
-1.05805314597882));
#69069=CARTESIAN_POINT('Ctrl Pts',(0.702086931244113,-0.0670124141673551,
-1.04221103255059));
#69070=CARTESIAN_POINT('Ctrl Pts',(0.648905383326142,0.276294274581765,
-1.02636891912235));
#69071=CARTESIAN_POINT('Ctrl Pts',(0.438280522141762,0.552563938913369,
-1.01052680569412));
#69072=CARTESIAN_POINT('Ctrl Pts',(0.121316063044922,0.694765525572184,
-0.994684692265882));
#69073=CARTESIAN_POINT('Ctrl Pts',(-0.225083200276113,0.668396795047505,
-0.978842578837647));
#69074=CARTESIAN_POINT('Ctrl Pts',(-0.51687073479559,0.479855568049576,
-0.963000465409411));
#69075=CARTESIAN_POINT('Ctrl Pts',(-0.68325040076027,0.174887428185227,
-0.947158351981176));
#69076=CARTESIAN_POINT('Ctrl Pts',(-0.683853653629245,-0.172513486702478,
-0.931316238552941));
#69077=CARTESIAN_POINT('Ctrl Pts',(-0.518534126716599,-0.478057613794162,
-0.915474125124705));
#69078=CARTESIAN_POINT('Ctrl Pts',(-0.22740314400511,-0.66761106399827,
-0.89963201169647));
#69079=CARTESIAN_POINT('Ctrl Pts',(0.118902453310195,-0.695182658927227,
-0.883789898268235));
#69080=CARTESIAN_POINT('Ctrl Pts',(0.436358858299948,-0.55408272799238,
-0.86794778484));
#69081=CARTESIAN_POINT('Ctrl Pts',(0.647941916898673,-0.278546216994571,
-0.852105671411764));
#69082=CARTESIAN_POINT('Ctrl Pts',(0.702315427199591,0.0645737051265365,
-0.836263557983531));
#69083=CARTESIAN_POINT('Ctrl Pts',(0.586286794664772,0.392026168868892,
-0.820421444555292));
#69084=CARTESIAN_POINT('Ctrl Pts',(0.328007939141782,0.624361685672875,
-0.804579331127061));
#69085=CARTESIAN_POINT('Ctrl Pts',(-0.00985517942347469,0.705208903882278,
-0.788737217698822));
#69086=CARTESIAN_POINT('Ctrl Pts',(-0.345327144915973,0.614951937683339,
-0.772895104270589));
#69087=CARTESIAN_POINT('Ctrl Pts',(-0.597012704480207,0.375489751345548,
-0.757052990842353));
#69088=CARTESIAN_POINT('Ctrl Pts',(-0.703845623473477,0.044922833765742,
-0.741210877414119));
#69089=CARTESIAN_POINT('Ctrl Pts',(-0.639905129523691,-0.296543669441083,
-0.725368763985881));
#69090=CARTESIAN_POINT('Ctrl Pts',(-0.420705045567162,-0.56606005627552,
-0.709526650557648));
#69091=CARTESIAN_POINT('Ctrl Pts',(-0.0994296853315642,-0.69823381495827,
-0.693684537129411));
#69092=CARTESIAN_POINT('Ctrl Pts',(0.245970207536815,-0.660995748610087,
-0.677842423701176));
#69093=CARTESIAN_POINT('Ctrl Pts',(0.531690576341267,-0.46338089484376,
-0.662000310272941));
#69094=CARTESIAN_POINT('Ctrl Pts',(0.688407352137116,-0.153336362940691,
-0.646158196844705));
#69095=CARTESIAN_POINT('Ctrl Pts',(0.678096488492109,0.193912028948647,
-0.630316083416472));
#69096=CARTESIAN_POINT('Ctrl Pts',(0.503259700720423,0.494111724518966,
-0.614473969988234));
#69097=CARTESIAN_POINT('Ctrl Pts',(0.206317477008665,0.674425549158015,
-0.598631856560001));
#69098=CARTESIAN_POINT('Ctrl Pts',(-0.140683365416483,0.691104126287348,
-0.582789743131764));
#69099=CARTESIAN_POINT('Ctrl Pts',(-0.453550332947481,0.540100748156837,
-0.56694762970353));
#69100=CARTESIAN_POINT('Ctrl Pts',(-0.656372802486486,0.258053224805003,
-0.551105516275294));
#69101=CARTESIAN_POINT('Ctrl Pts',(-0.699940145751841,-0.086605513920196,
-0.535263402847059));
#69102=CARTESIAN_POINT('Ctrl Pts',(-0.573681658522724,-0.410251236866699,
-0.519421289418823));
#69103=CARTESIAN_POINT('Ctrl Pts',(-0.308231320835643,-0.634358081474877,
-0.503579175990589));
#69104=CARTESIAN_POINT('Ctrl Pts',(0.032004897278945,-0.704551211216498,
-0.487737062562353));
#69105=CARTESIAN_POINT('Ctrl Pts',(0.364475796750062,-0.603799731912975,
-0.471894949134118));
#69106=CARTESIAN_POINT('Ctrl Pts',(0.60851427060865,-0.356548881847406,
-0.456052835705882));
#69107=CARTESIAN_POINT('Ctrl Pts',(0.704909489523639,-0.0227889061948828,
-0.440210722277648));
#69108=CARTESIAN_POINT('Ctrl Pts',(0.630273170690079,0.316500320697992,
-0.424368608849411));
#69109=CARTESIAN_POINT('Ctrl Pts',(0.402714255056845,0.578997367377502,
-0.408526495421177));
#69110=CARTESIAN_POINT('Ctrl Pts',(0.0774451521325488,0.701012818064358,
-0.39268438199294));
#69111=CARTESIAN_POINT('Ctrl Pts',(-0.26661439669049,0.652942176782176,
-0.376842268564707));
#69112=CARTESIAN_POINT('Ctrl Pts',(-0.545985540464761,0.446448778736983,
-0.36100015513647));
#69113=CARTESIAN_POINT('Ctrl Pts',(-0.692884718193416,0.131633926296123,
-0.345158041708236));
#69114=CARTESIAN_POINT('Ctrl Pts',(-0.671669915542376,-0.21511914411509,
-0.32931592828));
#69115=CARTESIAN_POINT('Ctrl Pts',(-0.487488465654378,-0.509678055216417,
-0.313473814851765));
#69116=CARTESIAN_POINT('Ctrl Pts',(-0.185028133270616,-0.680574251437019,
-0.297631701423529));
#69117=CARTESIAN_POINT('Ctrl Pts',(0.162325390816526,-0.68634334526228,
-0.281789587995294));
#69118=CARTESIAN_POINT('Ctrl Pts',(0.470294081325063,-0.525585589562447,
-0.265947474567059));
#69119=CARTESIAN_POINT('Ctrl Pts',(0.664155702788206,-0.237305484551378,
-0.250105361138824));
#69120=CARTESIAN_POINT('Ctrl Pts',(0.696873939840873,0.108551823732687,
-0.234263247710588));
#69121=CARTESIAN_POINT('Ctrl Pts',(0.560510101409974,0.428071317231208,
-0.218421134282353));
#69122=CARTESIAN_POINT('Ctrl Pts',(0.288150599099951,0.643728235591383,
-0.202579020854118));
#69123=CARTESIAN_POINT('Ctrl Pts',(-0.0541233696112858,0.703198020558049,
-0.186736907425882));
#69124=CARTESIAN_POINT('Ctrl Pts',(-0.383263958328779,0.592051415322255,
-0.170894793997647));
#69125=CARTESIAN_POINT('Ctrl Pts',(-0.61941646401829,0.337256127609639,
-0.155052680569412));
#69126=CARTESIAN_POINT('Ctrl Pts',(-0.70527484326665,0.000632295077805697,
-0.139210567141176));
#69127=CARTESIAN_POINT('Ctrl Pts',(-0.620024187785913,-0.33614416060722,
-0.123368453712941));
#69128=CARTESIAN_POINT('Ctrl Pts',(-0.384315741505486,-0.591363827723695,
-0.107526340284706));
#69129=CARTESIAN_POINT('Ctrl Pts',(-0.055404374357266,-0.703098282770509,
-0.091684226856471));
#69130=CARTESIAN_POINT('Ctrl Pts',(0.287037892597339,-0.644247893625522,
-0.0758421134282355));
#69131=CARTESIAN_POINT('Ctrl Pts',(0.468762250669717,-0.500787277377127,
-0.0652807044760785));
#69132=CARTESIAN_POINT('Ctrl Pts',(0.5370608629359,-0.411689834101531,-0.0600000000000001));
#69133=CARTESIAN_POINT('Ctrl Pts',(-0.309090610374651,0.644553868208601,
-2.9529325805302));
#69134=CARTESIAN_POINT('Ctrl Pts',(-0.416020952304324,0.593276284929997,
-2.94765187605412));
#69135=CARTESIAN_POINT('Ctrl Pts',(-0.603763589782005,0.436531048185212,
-2.93709046710196));
#69136=CARTESIAN_POINT('Ctrl Pts',(-0.738904753534814,0.0952729899872264,
-2.92124835367373));
#69137=CARTESIAN_POINT('Ctrl Pts',(-0.694754493060791,-0.269008323351198,
-2.90540624024549));
#69138=CARTESIAN_POINT('Ctrl Pts',(-0.482042716752689,-0.568065795445821,
-2.88956412681726));
#69139=CARTESIAN_POINT('Ctrl Pts',(-0.152370222156937,-0.729271014617091,
-2.87372201338902));
#69140=CARTESIAN_POINT('Ctrl Pts',(0.21427011642781,-0.713545578744666,
-2.85787989996079));
#69141=CARTESIAN_POINT('Ctrl Pts',(0.528923111693477,-0.524687276812066,
-2.84203778653255));
#69142=CARTESIAN_POINT('Ctrl Pts',(0.715243564834969,-0.208527625326828,
-2.82619567310431));
#69143=CARTESIAN_POINT('Ctrl Pts',(0.728025345399933,0.158228440621952,
-2.81035355967608));
#69144=CARTESIAN_POINT('Ctrl Pts',(0.564166901188532,0.486592896336179,
-2.79451144624784));
#69145=CARTESIAN_POINT('Ctrl Pts',(0.263425218484532,0.696896170186273,
-2.77866933281961));
#69146=CARTESIAN_POINT('Ctrl Pts',(-0.101231109590118,0.738111965198415,
-2.76282721939137));
#69147=CARTESIAN_POINT('Ctrl Pts',(-0.441325812784774,0.600240441129041,
-2.74698510596314));
#69148=CARTESIAN_POINT('Ctrl Pts',(-0.674342049326689,0.316733080363853,
-2.7311429925349));
#69149=CARTESIAN_POINT('Ctrl Pts',(-0.7437432941174,-0.0436229076748224,
-2.71530087910667));
#69150=CARTESIAN_POINT('Ctrl Pts',(-0.632690792921485,-0.393394723822608,
-2.69945876567843));
#69151=CARTESIAN_POINT('Ctrl Pts',(-0.368129108570174,-0.647717534737413,
-2.6836166522502));
#69152=CARTESIAN_POINT('Ctrl Pts',(-0.0142485994228211,-0.744885242595864,
-2.66777453882196));
#69153=CARTESIAN_POINT('Ctrl Pts',(0.343089034482034,-0.661322130825325,
-2.65193242539373));
#69154=CARTESIAN_POINT('Ctrl Pts',(0.617183292995749,-0.4173030427585,-2.63609031196549));
#69155=CARTESIAN_POINT('Ctrl Pts',(0.74153093975943,-0.0720341027313379,
-2.62024819853726));
#69156=CARTESIAN_POINT('Ctrl Pts',(0.685961620094956,0.290712404805016,
-2.60440608510902));
#69157=CARTESIAN_POINT('Ctrl Pts',(0.463958066711043,0.582923630440996,
-2.58856397168078));
#69158=CARTESIAN_POINT('Ctrl Pts',(0.12938479650513,0.733700634451997,-2.57272185825255));
#69159=CARTESIAN_POINT('Ctrl Pts',(-0.236580987260744,0.70646053183839,
-2.55687974482432));
#69160=CARTESIAN_POINT('Ctrl Pts',(-0.545145344800533,0.507812563466085,
-2.54103763139608));
#69161=CARTESIAN_POINT('Ctrl Pts',(-0.721441591297748,0.185954502283091,
-2.52519551796784));
#69162=CARTESIAN_POINT('Ctrl Pts',(-0.72269513144614,-0.181021527884781,
-2.50935340453961));
#69163=CARTESIAN_POINT('Ctrl Pts',(-0.548601819957467,-0.504076472087772,
-2.49351129111137));
#69164=CARTESIAN_POINT('Ctrl Pts',(-0.24140175605559,-0.704827807870036,
-2.47766917768314));
#69165=CARTESIAN_POINT('Ctrl Pts',(0.124369392750774,-0.734567424216532,
-2.4618270642549));
#69166=CARTESIAN_POINT('Ctrl Pts',(0.459964910769068,-0.586079625507186,
-2.44598495082667));
#69167=CARTESIAN_POINT('Ctrl Pts',(0.683959567708728,-0.295391869070711,
-2.43014283739843));
#69168=CARTESIAN_POINT('Ctrl Pts',(0.742005747031568,0.0669665434790141,
-2.41430072397019));
#69169=CARTESIAN_POINT('Ctrl Pts',(0.620019757910135,0.413076925492657,
-2.39845861054196));
#69170=CARTESIAN_POINT('Ctrl Pts',(0.347598948113237,0.658962834948961,
-2.38261649711372));
#69171=CARTESIAN_POINT('Ctrl Pts',(-0.00915947312147629,0.744965200949376,
-2.36677438368549));
#69172=CARTESIAN_POINT('Ctrl Pts',(-0.363695539860336,0.65021734893734,
-2.35093227025725));
#69173=CARTESIAN_POINT('Ctrl Pts',(-0.629988493986507,0.397707862655514,
-2.33509015682902));
#69174=CARTESIAN_POINT('Ctrl Pts',(-0.743427922218747,0.0487028853243916,
-2.31924804340078));
#69175=CARTESIAN_POINT('Ctrl Pts',(-0.676490120955796,-0.312118828048898,
-2.30340592997255));
#69176=CARTESIAN_POINT('Ctrl Pts',(-0.445416147036459,-0.597211438715468,
-2.28756381654432));
#69177=CARTESIAN_POINT('Ctrl Pts',(-0.106271265133095,-0.737403190107296,
-2.27172170311607));
#69178=CARTESIAN_POINT('Ctrl Pts',(0.258658115585497,-0.69867948718648,
-2.25587958968785));
#69179=CARTESIAN_POINT('Ctrl Pts',(0.560829516839833,-0.490435826194014,
-2.2400374762596));
#69180=CARTESIAN_POINT('Ctrl Pts',(0.726927370890315,-0.163198174082615,
-2.22419536283138));
#69181=CARTESIAN_POINT('Ctrl Pts',(0.716651508960247,0.203636100135525,
-2.20835324940314));
#69182=CARTESIAN_POINT('Ctrl Pts',(0.532495153930052,0.521062335632134,
-2.1925111359749));
#69183=CARTESIAN_POINT('Ctrl Pts',(0.21913999197469,0.712063698337962,-2.17666902254667));
#69184=CARTESIAN_POINT('Ctrl Pts',(-0.147384903646339,0.730297704193682,
-2.16082690911843));
#69185=CARTESIAN_POINT('Ctrl Pts',(-0.478149936347774,0.571340253215214,
-2.1449847956902));
#69186=CARTESIAN_POINT('Ctrl Pts',(-0.692901892025805,0.273759044782935,
-2.12914268226196));
#69187=CARTESIAN_POINT('Ctrl Pts',(-0.739535702204835,-0.0902440676045038,
-2.11330056883373));
#69188=CARTESIAN_POINT('Ctrl Pts',(-0.606736648632429,-0.4323513452965,
-2.09745845540549));
#69189=CARTESIAN_POINT('Ctrl Pts',(-0.326725642908844,-0.669557615772689,
-2.08161634197725));
#69190=CARTESIAN_POINT('Ctrl Pts',(0.0325585035074464,-0.744309740916213,
-2.06577422854902));
#69191=CARTESIAN_POINT('Ctrl Pts',(0.383943010316906,-0.63847068170919,
-2.04993211512078));
#69192=CARTESIAN_POINT('Ctrl Pts',(0.642171779474866,-0.377720071242564,
-2.03409000169255));
#69193=CARTESIAN_POINT('Ctrl Pts',(0.744591003443873,-0.0253235890791637,
-2.01824788826431));
#69194=CARTESIAN_POINT('Ctrl Pts',(0.666350800595265,0.333217132091755,
-2.00240577483608));
#69195=CARTESIAN_POINT('Ctrl Pts',(0.426434519015904,0.610909688550673,
-1.98656366140784));
#69196=CARTESIAN_POINT('Ctrl Pts',(0.0830528243112992,0.740377792040875,
-1.97072154797961));
#69197=CARTESIAN_POINT('Ctrl Pts',(-0.280479900376565,0.690208716301205,
-1.95487943455138));
#69198=CARTESIAN_POINT('Ctrl Pts',(-0.575960046129783,0.472574937798846,
-1.93903732112313));
#69199=CARTESIAN_POINT('Ctrl Pts',(-0.731695538345162,0.14028073901712,
-1.9231952076949));
#69200=CARTESIAN_POINT('Ctrl Pts',(-0.709900418518422,-0.226049645787761,
-1.90735309426667));
#69201=CARTESIAN_POINT('Ctrl Pts',(-0.515862816424316,-0.537533814010037,
-1.89151098083843));
#69202=CARTESIAN_POINT('Ctrl Pts',(-0.196661896078054,-0.71859664987,-1.8756688674102));
#69203=CARTESIAN_POINT('Ctrl Pts',(0.17025491830668,-0.725307044889122,
-1.85982675398196));
#69204=CARTESIAN_POINT('Ctrl Pts',(0.4958629392573,-0.556036862127428,-1.84398464055372));
#69205=CARTESIAN_POINT('Ctrl Pts',(0.701160193663617,-0.251855969544111,
-1.82814252712549));
#69206=CARTESIAN_POINT('Ctrl Pts',(0.736335598479057,0.113432504097785,
-1.81230041369725));
#69207=CARTESIAN_POINT('Ctrl Pts',(0.592854577751664,0.451198954134761,
-1.79645830026902));
#69208=CARTESIAN_POINT('Ctrl Pts',(0.305529798897411,0.679491419047446,
-1.78061618684078));
#69209=CARTESIAN_POINT('Ctrl Pts',(-0.055925392611856,0.742919509122363,
-1.76477407341255));
#69210=CARTESIAN_POINT('Ctrl Pts',(-0.403811457812752,0.626093725501658,
-1.74893195998431));
#69211=CARTESIAN_POINT('Ctrl Pts',(-0.653721122313909,0.357359400063925,
-1.73308984655608));
#69212=CARTESIAN_POINT('Ctrl Pts',(-0.745019035250031,0.00191929375476884,
-1.71724773312784));
#69213=CARTESIAN_POINT('Ctrl Pts',(-0.655553668407108,-0.353986489023787,
-1.70140561969961));
#69214=CARTESIAN_POINT('Ctrl Pts',(-0.407031921034679,-0.624004857218455,
-1.68556350627137));
#69215=CARTESIAN_POINT('Ctrl Pts',(-0.059752394948178,-0.742621503776561,
-1.66972139284314));
#69216=CARTESIAN_POINT('Ctrl Pts',(0.302024799485628,-0.681056581400599,
-1.6538792794149));
#69217=CARTESIAN_POINT('Ctrl Pts',(0.590521996031449,-0.45424753029206,
-1.63803716598667));
#69218=CARTESIAN_POINT('Ctrl Pts',(0.7357413865968,-0.117224820844492,-1.62219505255843));
#69219=CARTESIAN_POINT('Ctrl Pts',(0.702448524698983,0.248240038514392,
-1.6063529391302));
#69220=CARTESIAN_POINT('Ctrl Pts',(0.498721226642195,0.553474646817637,
-1.59051082570196));
#69221=CARTESIAN_POINT('Ctrl Pts',(0.173989658415294,0.724420213231198,
-1.57466871227373));
#69222=CARTESIAN_POINT('Ctrl Pts',(-0.192956859785644,0.719600373009261,
-1.55882659884549));
#69223=CARTESIAN_POINT('Ctrl Pts',(-0.513086433478563,0.540184559529105,
-1.54298448541725));
#69224=CARTESIAN_POINT('Ctrl Pts',(-0.708726320146782,0.229704265751867,
-1.52714237198902));
#69225=CARTESIAN_POINT('Ctrl Pts',(-0.732408594950133,-0.1365089616713,
-1.51130025856078));
#69226=CARTESIAN_POINT('Ctrl Pts',(-0.5783872494465,-0.469601145921851,
-1.49545814513255));
#69227=CARTESIAN_POINT('Ctrl Pts',(-0.284032340308158,-0.68875443826699,
-1.47961603170431));
#69228=CARTESIAN_POINT('Ctrl Pts',(0.0792370729813301,-0.740795877984452,
-1.46377391827608));
#69229=CARTESIAN_POINT('Ctrl Pts',(0.423281268505223,-0.613098698666059,
-1.44793180484784));
#69230=CARTESIAN_POINT('Ctrl Pts',(0.664625121160208,-0.336645948878317,
-1.43208969141961));
#69231=CARTESIAN_POINT('Ctrl Pts',(0.744711595090442,0.0214868962685335,
-1.41624757799137));
#69232=CARTESIAN_POINT('Ctrl Pts',(0.644109383163333,0.374406395637621,
-1.40040546456314));
#69233=CARTESIAN_POINT('Ctrl Pts',(0.387227507055584,0.636484017358584,
-1.3845633511349));
#69234=CARTESIAN_POINT('Ctrl Pts',(0.0363929788890332,0.744132110354732,
-1.36872123770667));
#69235=CARTESIAN_POINT('Ctrl Pts',(-0.323271544101347,0.671232117339253,
-1.35287912427843));
#69236=CARTESIAN_POINT('Ctrl Pts',(-0.604500991199494,0.435471696224031,
-1.3370370108502));
#69237=CARTESIAN_POINT('Ctrl Pts',(-0.739060921642629,0.0940531800321082,
-1.32119489742196));
#69238=CARTESIAN_POINT('Ctrl Pts',(-0.694303183903219,-0.270185372282176,
-1.30535278399373));
#69239=CARTESIAN_POINT('Ctrl Pts',(-0.481087306512033,-0.56886909749643,
-1.28951067056549));
#69240=CARTESIAN_POINT('Ctrl Pts',(-0.151145660689984,-0.729528639484422,
-1.27366855713725));
#69241=CARTESIAN_POINT('Ctrl Pts',(0.215468317056472,-0.713183322097661,
-1.25782644370902));
#69242=CARTESIAN_POINT('Ctrl Pts',(0.529803416228333,-0.523798994583028,
-1.24198433028078));
#69243=CARTESIAN_POINT('Ctrl Pts',(0.715592802305182,-0.207325801246306,
-1.22614221685255));
#69244=CARTESIAN_POINT('Ctrl Pts',(0.727758568298884,0.159450659581461,
-1.21030010342431));
#69245=CARTESIAN_POINT('Ctrl Pts',(0.563348945653209,0.487539754281456,
-1.19445798999608));
#69246=CARTESIAN_POINT('Ctrl Pts',(0.262254489119811,0.69733752911335,-1.17861587656784));
#69247=CARTESIAN_POINT('Ctrl Pts',(-0.102470531663754,0.737940943920278,
-1.16277376313961));
#69248=CARTESIAN_POINT('Ctrl Pts',(-0.442333222080111,0.599498429704058,
-1.14693164971137));
#69249=CARTESIAN_POINT('Ctrl Pts',(-0.674873011744545,0.315600165703775,
-1.13108953628314));
#69250=CARTESIAN_POINT('Ctrl Pts',(-0.743668986465564,-0.0448718747400542,
-1.1152474228549));
#69251=CARTESIAN_POINT('Ctrl Pts',(-0.632029242496039,-0.394456693698165,
-1.09940530942667));
#69252=CARTESIAN_POINT('Ctrl Pts',(-0.367040827708315,-0.64833484972551,
-1.08356319599843));
#69253=CARTESIAN_POINT('Ctrl Pts',(-0.0129976362099471,-0.744908120526524,
-1.0677210825702));
#69254=CARTESIAN_POINT('Ctrl Pts',(0.344199159746186,-0.66074502268532,
-1.05187896914196));
#69255=CARTESIAN_POINT('Ctrl Pts',(0.617883231773016,-0.416265970825311,
-1.03603685571372));
#69256=CARTESIAN_POINT('Ctrl Pts',(0.741650866485886,-0.07078869128708,
-1.02019474228549));
#69257=CARTESIAN_POINT('Ctrl Pts',(0.685472437093205,0.291863982976498,
-1.00435262885725));
#69258=CARTESIAN_POINT('Ctrl Pts',(0.462978463983554,0.583701968868388,
-0.988510515429021));
#69259=CARTESIAN_POINT('Ctrl Pts',(0.128152454164742,0.733916885665508,
-0.972668402000784));
#69260=CARTESIAN_POINT('Ctrl Pts',(-0.237767067135667,0.706062226973733,
-0.956826288572548));
#69261=CARTESIAN_POINT('Ctrl Pts',(-0.545997384744169,0.506896342880804,
-0.940984175144315));
#69262=CARTESIAN_POINT('Ctrl Pts',(-0.721752861647405,0.184742667722392,
-0.925142061716078));
#69263=CARTESIAN_POINT('Ctrl Pts',(-0.72239010896405,-0.182234950117461,
-0.909299948287843));
#69264=CARTESIAN_POINT('Ctrl Pts',(-0.547754511966775,-0.504997070480062,
-0.893457834859609));
#69265=CARTESIAN_POINT('Ctrl Pts',(-0.240217744110618,-0.705232218483962,
-0.877615721431371));
#69266=CARTESIAN_POINT('Ctrl Pts',(0.125602832926312,-0.734357525279266,
-0.861773608003138));
#69267=CARTESIAN_POINT('Ctrl Pts',(0.460948510725695,-0.585306344603549,
-0.845931494574901));
#69268=CARTESIAN_POINT('Ctrl Pts',(0.684454677498251,-0.294242826631626,
-0.830089381146668));
#69269=CARTESIAN_POINT('Ctrl Pts',(0.741892238623479,0.068212556348874,
-0.814247267718431));
#69270=CARTESIAN_POINT('Ctrl Pts',(0.619325171744547,0.414117589842537,
-0.798405154290196));
#69271=CARTESIAN_POINT('Ctrl Pts',(0.346491810989388,0.659545655349725,
-0.782563040861961));
#69272=CARTESIAN_POINT('Ctrl Pts',(-0.0104105375467384,0.744948768225972,
-0.766720927433726));
#69273=CARTESIAN_POINT('Ctrl Pts',(-0.364786986982069,0.649605650146261,
-0.75087881400549));
#69274=CARTESIAN_POINT('Ctrl Pts',(-0.630655506998571,0.396649313708947,
-0.735036700577256));
#69275=CARTESIAN_POINT('Ctrl Pts',(-0.743508664370658,0.047454320974652,
-0.719194587149019));
#69276=CARTESIAN_POINT('Ctrl Pts',(-0.675965001853878,-0.31325446978789,
-0.703352473720785));
#69277=CARTESIAN_POINT('Ctrl Pts',(-0.444412575842957,-0.597958618138441,
-0.687510360292549));
#69278=CARTESIAN_POINT('Ctrl Pts',(-0.105032737398919,-0.737580619761592,
-0.671668246864314));
#69279=CARTESIAN_POINT('Ctrl Pts',(0.259831097021177,-0.698244117479107,
-0.655826133436078));
#69280=CARTESIAN_POINT('Ctrl Pts',(0.561652352575658,-0.489493290474582,
-0.639984020007844));
#69281=CARTESIAN_POINT('Ctrl Pts',(0.727200417052382,-0.161977158921392,
-0.624141906579607));
#69282=CARTESIAN_POINT('Ctrl Pts',(0.716308516610675,0.204839340958754,
-0.608299793151373));
#69283=CARTESIAN_POINT('Ctrl Pts',(0.531619342985543,0.521955860908782,
-0.592457679723137));
#69284=CARTESIAN_POINT('Ctrl Pts',(0.217943859635038,0.712430712856194,
-0.576615566294903));
#69285=CARTESIAN_POINT('Ctrl Pts',(-0.148611140897316,0.730049159560228,
-0.560773452866666));
#69286=CARTESIAN_POINT('Ctrl Pts',(-0.479108757699555,0.57053645358472,
-0.544931339438432));
#69287=CARTESIAN_POINT('Ctrl Pts',(-0.693360659540056,0.272595015316652,
-0.529089226010196));
#69288=CARTESIAN_POINT('Ctrl Pts',(-0.739383105543975,-0.0914858995132521,
-0.513247112581961));
#69289=CARTESIAN_POINT('Ctrl Pts',(-0.606009712182644,-0.433369675119762,
-0.497404999153725));
#69290=CARTESIAN_POINT('Ctrl Pts',(-0.325600742590041,-0.670105367086779,
-0.481562885725491));
#69291=CARTESIAN_POINT('Ctrl Pts',(0.0338084341730408,-0.744254013326329,
-0.465720772297255));
#69292=CARTESIAN_POINT('Ctrl Pts',(0.385014701803114,-0.637824996348643,
-0.44987865886902));
#69293=CARTESIAN_POINT('Ctrl Pts',(0.642805208275577,-0.376641090154065,
-0.434036545440785));
#69294=CARTESIAN_POINT('Ctrl Pts',(0.744632481298183,-0.024073104445561,
-0.418194432012549));
#69295=CARTESIAN_POINT('Ctrl Pts',(0.665790263802216,0.334335716337538,
-0.402352318584314));
#69296=CARTESIAN_POINT('Ctrl Pts',(0.425407970035668,0.611624971351682,
-0.386510205156079));
#69297=CARTESIAN_POINT('Ctrl Pts',(0.0818093338989499,0.740516224983506,
-0.370668091727843));
#69298=CARTESIAN_POINT('Ctrl Pts',(-0.281638625537042,0.689736711545923,
-0.354825978299609));
#69299=CARTESIAN_POINT('Ctrl Pts',(-0.576752865142938,0.471607017389029,
-0.338983864871373));
#69300=CARTESIAN_POINT('Ctrl Pts',(-0.731930091210175,0.139051748653782,
-0.323141751443138));
#69301=CARTESIAN_POINT('Ctrl Pts',(-0.709519794040012,-0.227241517439931,
-0.307299638014902));
#69302=CARTESIAN_POINT('Ctrl Pts',(-0.514959368797507,-0.538399383976947,
-0.291457524586667));
#69303=CARTESIAN_POINT('Ctrl Pts',(-0.195454820845694,-0.71892590621481,
-0.275615411158432));
#69304=CARTESIAN_POINT('Ctrl Pts',(0.171472735631759,-0.725020099460598,
-0.259773297730196));
#69305=CARTESIAN_POINT('Ctrl Pts',(0.49679604817575,-0.555203338168894,
-0.243931184301961));
#69306=CARTESIAN_POINT('Ctrl Pts',(0.70158214109123,-0.25067810039921,-0.228089070873726));
#69307=CARTESIAN_POINT('Ctrl Pts',(0.736144113092337,0.114668925666095,
-0.21224695744549));
#69308=CARTESIAN_POINT('Ctrl Pts',(0.59209591274996,0.45219395093952,-0.196404844017255));
#69309=CARTESIAN_POINT('Ctrl Pts',(0.30438843395392,0.680003547227091,-0.18056273058902));
#69310=CARTESIAN_POINT('Ctrl Pts',(-0.0571733245314984,0.742824567798009,
-0.164720617160785));
#69311=CARTESIAN_POINT('Ctrl Pts',(-0.404861612056579,0.625414639751036,
-0.148878503732549));
#69312=CARTESIAN_POINT('Ctrl Pts',(-0.654321761039958,0.356261152484546,
-0.133036390304314));
#69313=CARTESIAN_POINT('Ctrl Pts',(-0.745018423420191,0.000667926109236243,
-0.117194276876079));
#69314=CARTESIAN_POINT('Ctrl Pts',(-0.654963731198904,-0.355086524024519,
-0.101352163447843));
#69315=CARTESIAN_POINT('Ctrl Pts',(-0.405972665217733,-0.624688305282234,
-0.0855100500196082));
#69316=CARTESIAN_POINT('Ctrl Pts',(-0.0585265163337596,-0.742719209596254,
-0.0696679365913732));
#69317=CARTESIAN_POINT('Ctrl Pts',(0.303213024321455,-0.680552488980807,
-0.0538258231631377));
#69318=CARTESIAN_POINT('Ctrl Pts',(0.495177895946605,-0.529007593879737,
-0.0432644142109807));
#69319=CARTESIAN_POINT('Ctrl Pts',(0.567325265044103,-0.434889340047653,
-0.0379837097349022));
#69320=CARTESIAN_POINT('Ctrl Pts',(-0.325579286442198,0.678938089483055,
-2.9309162902651));
#69321=CARTESIAN_POINT('Ctrl Pts',(-0.438213909610741,0.624925064130741,
-2.92563558578902));
#69322=CARTESIAN_POINT('Ctrl Pts',(-0.635971822316887,0.459818132313165,
-2.91507417683686));
#69323=CARTESIAN_POINT('Ctrl Pts',(-0.778322195271528,0.100355400831034,
-2.89923206340863));
#69324=CARTESIAN_POINT('Ctrl Pts',(-0.731816705234331,-0.283358779024489,
-2.88338994998039));
#69325=CARTESIAN_POINT('Ctrl Pts',(-0.507757655804455,-0.598369701717211,
-2.86754783655216));
#69326=CARTESIAN_POINT('Ctrl Pts',(-0.160498528715463,-0.768174537150173,
-2.85170572312392));
#69327=CARTESIAN_POINT('Ctrl Pts',(0.225700520400454,-0.751610215820158,
-2.83586360969569));
#69328=CARTESIAN_POINT('Ctrl Pts',(0.557138921428952,-0.552677122681642,
-2.82002149626745));
#69329=CARTESIAN_POINT('Ctrl Pts',(0.753398782282915,-0.21965169170006,
-2.80417938283922));
#69330=CARTESIAN_POINT('Ctrl Pts',(0.766862416751649,0.166669258345032,
-2.78833726941098));
#69331=CARTESIAN_POINT('Ctrl Pts',(0.594262817950469,0.512550568213471,
-2.77249515598275));
#69332=CARTESIAN_POINT('Ctrl Pts',(0.277477839139527,0.734072631771401,
-2.7566530425545));
#69333=CARTESIAN_POINT('Ctrl Pts',(-0.106631360901428,0.777487115032269,
-2.74081092912628));
#69334=CARTESIAN_POINT('Ctrl Pts',(-0.464868677313834,0.632260728592397,
-2.72496881569804));
#69335=CARTESIAN_POINT('Ctrl Pts',(-0.710315344007488,0.333629449864264,
-2.70912670226981));
#69336=CARTESIAN_POINT('Ctrl Pts',(-0.783418851518672,-0.0459500051977844,
-2.69328458884157));
#69337=CARTESIAN_POINT('Ctrl Pts',(-0.666442169331009,-0.414380667588194,
-2.67744247541334));
#69338=CARTESIAN_POINT('Ctrl Pts',(-0.387767238679958,-0.682270524233312,
-2.6616003619851));
#69339=CARTESIAN_POINT('Ctrl Pts',(-0.0150087019054416,-0.784621718116017,
-2.64575824855686));
#69340=CARTESIAN_POINT('Ctrl Pts',(0.361391382602686,-0.696600867951191,
-2.62991613512863));
#69341=CARTESIAN_POINT('Ctrl Pts',(0.65010740990818,-0.439564394165159,
-2.61407402170039));
#69342=CARTESIAN_POINT('Ctrl Pts',(0.781088477417849,-0.0758768172813364,
-2.59823190827216));
#69343=CARTESIAN_POINT('Ctrl Pts',(0.722554769705059,0.306220681377498,
-2.58238979484392));
#69344=CARTESIAN_POINT('Ctrl Pts',(0.488708266212908,0.614020139334652,
-2.56654768141569));
#69345=CARTESIAN_POINT('Ctrl Pts',(0.136286927873838,0.772840458458201,
-2.55070556798745));
#69346=CARTESIAN_POINT('Ctrl Pts',(-0.249201581778172,0.74414721164362,
-2.53486345455922));
#69347=CARTESIAN_POINT('Ctrl Pts',(-0.574226542023743,0.534902214788316,
-2.51902134113098));
#69348=CARTESIAN_POINT('Ctrl Pts',(-0.75992744722895,0.195874388065881,
-2.50317922770274));
#69349=CARTESIAN_POINT('Ctrl Pts',(-0.761247858439583,-0.190678260358557,
-2.48733711427451));
#69350=CARTESIAN_POINT('Ctrl Pts',(-0.577867405503348,-0.530966818745191,
-2.47149500084628));
#69351=CARTESIAN_POINT('Ctrl Pts',(-0.254279518187912,-0.74242738876084,
-2.45565288741804));
#69352=CARTESIAN_POINT('Ctrl Pts',(0.131003973553142,-0.773753487788634,
-2.43981077398981));
#69353=CARTESIAN_POINT('Ctrl Pts',(0.484502092299483,-0.617344493382228,
-2.42396866056157));
#69354=CARTESIAN_POINT('Ctrl Pts',(0.720445916296219,-0.311149775259424,
-2.40812654713334));
#69355=CARTESIAN_POINT('Ctrl Pts',(0.781588613648687,0.0705389251875665,
-2.3922844337051));
#69356=CARTESIAN_POINT('Ctrl Pts',(0.653095188222527,0.435112831427073,
-2.37644232027686));
#69357=CARTESIAN_POINT('Ctrl Pts',(0.366141881041268,0.694115713623784,
-2.36060020684863));
#69358=CARTESIAN_POINT('Ctrl Pts',(-0.00964809225185164,0.784705941909324,
-2.34475809342039));
#69359=CARTESIAN_POINT('Ctrl Pts',(-0.383097157841225,0.684903692942206,
-2.32891597999216));
#69360=CARTESIAN_POINT('Ctrl Pts',(-0.663595714183315,0.418923894125693,
-2.31307386656392));
#69361=CARTESIAN_POINT('Ctrl Pts',(-0.783086655863804,0.0513009781577409,
-2.29723175313568));
#69362=CARTESIAN_POINT('Ctrl Pts',(-0.712578006167895,-0.328769046714688,
-2.28138963970745));
#69363=CARTESIAN_POINT('Ctrl Pts',(-0.469177213588559,-0.629070141718054,
-2.26554752627922));
#69364=CARTESIAN_POINT('Ctrl Pts',(-0.111940387413922,-0.776740529789401,
-2.24970541285098));
#69365=CARTESIAN_POINT('Ctrl Pts',(0.272456431474037,-0.73595108118701,
-2.23386329942275));
#69366=CARTESIAN_POINT('Ctrl Pts',(0.590747398269758,-0.516598502116886,
-2.21802118599451));
#69367=CARTESIAN_POINT('Ctrl Pts',(0.7657058699483,-0.17190410605513,-2.20217907256628));
#69368=CARTESIAN_POINT('Ctrl Pts',(0.754881834269203,0.214499224339534,
-2.18633695913804));
#69369=CARTESIAN_POINT('Ctrl Pts',(0.560901517002844,0.548858806229622,
-2.17049484570981));
#69370=CARTESIAN_POINT('Ctrl Pts',(0.230830183199643,0.75004928336471,-2.15465273228157));
#69371=CARTESIAN_POINT('Ctrl Pts',(-0.155247264558969,0.769255996270977,
-2.13881061885334));
#69372=CARTESIAN_POINT('Ctrl Pts',(-0.503657212038229,0.601818837951901,
-2.1229685054251));
#69373=CARTESIAN_POINT('Ctrl Pts',(-0.729865275773881,0.288362931340722,
-2.10712639199686));
#69374=CARTESIAN_POINT('Ctrl Pts',(-0.778986802383074,-0.0950582067203571,
-2.09128427856863));
#69375=CARTESIAN_POINT('Ctrl Pts',(-0.639103481275727,-0.455415459962816,
-2.07544216514039));
#69376=CARTESIAN_POINT('Ctrl Pts',(-0.344155073334948,-0.705275681169934,
-2.05960005171216));
#69377=CARTESIAN_POINT('Ctrl Pts',(0.0342953618899345,-0.784015515857139,
-2.04375793828392));
#69378=CARTESIAN_POINT('Ctrl Pts',(0.404424745164305,-0.672530390726459,
-2.02791582485569));
#69379=CARTESIAN_POINT('Ctrl Pts',(0.67642892639579,-0.39786983862431,-2.01207371142745));
#69380=CARTESIAN_POINT('Ctrl Pts',(0.784311782550415,-0.0266744953932996,
-1.99623159799922));
#69381=CARTESIAN_POINT('Ctrl Pts',(0.701897795973256,0.350992855995365,
-1.98038948457098));
#69382=CARTESIAN_POINT('Ctrl Pts',(0.449182996038718,0.64349913521432,-1.96454737114274));
#69383=CARTESIAN_POINT('Ctrl Pts',(0.087483341029052,0.779873814148348,
-1.94870525771451));
#69384=CARTESIAN_POINT('Ctrl Pts',(-0.295442316139248,0.727028430521238,
-1.93286314428627));
#69385=CARTESIAN_POINT('Ctrl Pts',(-0.606685077268622,0.497784810908752,
-1.91702103085804));
#69386=CARTESIAN_POINT('Ctrl Pts',(-0.770728398959144,0.147764122809877,
-1.90117891742981));
#69387=CARTESIAN_POINT('Ctrl Pts',(-0.747770601721272,-0.238108437803669,
-1.88533680400157));
#69388=CARTESIAN_POINT('Ctrl Pts',(-0.543381914675166,-0.566208968275712,
-1.86949469057333));
#69389=CARTESIAN_POINT('Ctrl Pts',(-0.207152976008731,-0.75693074021513,
-1.8536525771451));
#69390=CARTESIAN_POINT('Ctrl Pts',(0.179337297721125,-0.763999106411768,
-1.83781046371686));
#69391=CARTESIAN_POINT('Ctrl Pts',(0.522315128695877,-0.585699075709795,
-1.82196835028863));
#69392=CARTESIAN_POINT('Ctrl Pts',(0.738564122856956,-0.265291419726369,
-1.80612623686039));
#69393=CARTESIAN_POINT('Ctrl Pts',(0.775615986665582,0.119483648172757,
-1.79028412343216));
#69394=CARTESIAN_POINT('Ctrl Pts',(0.624480860659006,0.475268508974123,
-1.77444201000392));
#69395=CARTESIAN_POINT('Ctrl Pts',(0.321828520741137,0.715739410811971,
-1.75859989657569));
#69396=CARTESIAN_POINT('Ctrl Pts',(-0.0589087756450992,0.782551121080208,
-1.74275778314745));
#69397=CARTESIAN_POINT('Ctrl Pts',(-0.425353090255639,0.659493176281511,
-1.72691566971922));
#69398=CARTESIAN_POINT('Ctrl Pts',(-0.6885943778013,0.376423011799676,-1.71107355629098));
#69399=CARTESIAN_POINT('Ctrl Pts',(-0.784762648042105,0.00202167995460736,
-1.69523144286274));
#69400=CARTESIAN_POINT('Ctrl Pts',(-0.690524682473687,-0.372870170228878,
-1.67938932943451));
#69401=CARTESIAN_POINT('Ctrl Pts',(-0.428745351562249,-0.657292875714973,
-1.66354721600628));
#69402=CARTESIAN_POINT('Ctrl Pts',(-0.0629399323611319,-0.782237218410294,
-1.64770510257804));
#69403=CARTESIAN_POINT('Ctrl Pts',(0.318136544443031,-0.717388067953282,
-1.6318629891498));
#69404=CARTESIAN_POINT('Ctrl Pts',(0.622023845574929,-0.478479713768591,
-1.61602087572157));
#69405=CARTESIAN_POINT('Ctrl Pts',(0.774990076093966,-0.123478268969749,
-1.60017876229333));
#69406=CARTESIAN_POINT('Ctrl Pts',(0.739921180901159,0.261482594077944,
-1.5843366488651));
#69407=CARTESIAN_POINT('Ctrl Pts',(0.525325893617189,0.583000177055891,
-1.56849453543686));
#69408=CARTESIAN_POINT('Ctrl Pts',(0.183271270410032,0.763064966037748,
-1.55265242200863));
#69409=CARTESIAN_POINT('Ctrl Pts',(-0.203250291708922,0.757988007736359,
-1.53681030858039));
#69410=CARTESIAN_POINT('Ctrl Pts',(-0.540457423448226,0.569001119850921,
-1.52096819515216));
#69411=CARTESIAN_POINT('Ctrl Pts',(-0.74653387017,0.241958016277407,-1.50512608172392));
#69412=CARTESIAN_POINT('Ctrl Pts',(-0.771479494116511,-0.14379113710389,
-1.48928396829569));
#69413=CARTESIAN_POINT('Ctrl Pts',(-0.609241761610959,-0.494652379819475,
-1.47344185486745));
#69414=CARTESIAN_POINT('Ctrl Pts',(-0.29918426370814,-0.725496572908043,
-1.45759974143922));
#69415=CARTESIAN_POINT('Ctrl Pts',(0.0834640355129492,-0.780314203207778,
-1.44175762801098));
#69416=CARTESIAN_POINT('Ctrl Pts',(0.445861532957072,-0.645804919756011,
-1.42591551458274));
#69417=CARTESIAN_POINT('Ctrl Pts',(0.70008005884299,-0.354604585647581,
-1.41007340115451));
#69418=CARTESIAN_POINT('Ctrl Pts',(0.784438807251015,0.0226331312571616,
-1.39423128772627));
#69419=CARTESIAN_POINT('Ctrl Pts',(0.678469893041574,0.394379392448504,
-1.37838917429804));
#69420=CARTESIAN_POINT('Ctrl Pts',(0.407884455904809,0.670437746239824,
-1.3625470608698));
#69421=CARTESIAN_POINT('Ctrl Pts',(0.0383343903065725,0.78382840945689,
-1.34670494744157));
#69422=CARTESIAN_POINT('Ctrl Pts',(-0.340516712972966,0.707039510308996,
-1.33086283401333));
#69423=CARTESIAN_POINT('Ctrl Pts',(-0.636748560979497,0.458702268407773,
-1.3150207205851));
#69424=CARTESIAN_POINT('Ctrl Pts',(-0.778486694287029,0.0990705191767479,
-1.29917860715686));
#69425=CARTESIAN_POINT('Ctrl Pts',(-0.731341320643033,-0.28459861853495,
-1.28333649372863));
#69426=CARTESIAN_POINT('Ctrl Pts',(-0.506751278470523,-0.599215856532842,
-1.26749438030039));
#69427=CARTESIAN_POINT('Ctrl Pts',(-0.159208642076294,-0.768445905213971,
-1.25165226687216));
#69428=CARTESIAN_POINT('Ctrl Pts',(0.226962639962163,-0.751228634314016,
-1.23581015344392));
#69429=CARTESIAN_POINT('Ctrl Pts',(0.558066186485511,-0.551741454354678,
-1.21996804001569));
#69430=CARTESIAN_POINT('Ctrl Pts',(0.753766650094275,-0.218385755390668,
-1.20412592658745));
#69431=CARTESIAN_POINT('Ctrl Pts',(0.766581408221195,0.167956677513898,
-1.18828381315922));
#69432=CARTESIAN_POINT('Ctrl Pts',(0.593401227948724,0.513547937023258,
-1.17244169973098));
#69433=CARTESIAN_POINT('Ctrl Pts',(0.27624465631744,0.734537535329514,-1.15659958630275));
#69434=CARTESIAN_POINT('Ctrl Pts',(-0.10793690089776,0.777306970492665,
-1.14075747287451));
#69435=CARTESIAN_POINT('Ctrl Pts',(-0.465929827631969,0.631479133997901,
-1.12491535944628));
#69436=CARTESIAN_POINT('Ctrl Pts',(-0.710874631023432,0.33243609900129,
-1.10907324601804));
#69437=CARTESIAN_POINT('Ctrl Pts',(-0.783340579868063,-0.0472655993706233,
-1.09323113258981));
#69438=CARTESIAN_POINT('Ctrl Pts',(-0.665745327989884,-0.415499289062616,
-1.07738901916157));
#69439=CARTESIAN_POINT('Ctrl Pts',(-0.386620902639458,-0.682920770363698,
-1.06154690573333));
#69440=CARTESIAN_POINT('Ctrl Pts',(-0.0136910050989311,-0.784645816487464,
-1.0457047923051));
#69441=CARTESIAN_POINT('Ctrl Pts',(0.362560728351902,-0.695992973534098,
-1.02986267887686));
#69442=CARTESIAN_POINT('Ctrl Pts',(0.650844687457245,-0.438471998832969,
-1.01402056544863));
#69443=CARTESIAN_POINT('Ctrl Pts',(0.781214801727662,-0.0745649684068042,
-0.998178452020392));
#69444=CARTESIAN_POINT('Ctrl Pts',(0.722039490860267,0.307433691371231,
-0.982336338592158));
#69445=CARTESIAN_POINT('Ctrl Pts',(0.487676405825348,0.614839998823407,
-0.966494225163922));
#69446=CARTESIAN_POINT('Ctrl Pts',(0.134988845284561,0.773068245758832,
-0.950652111735687));
#69447=CARTESIAN_POINT('Ctrl Pts',(-0.250450933995221,0.743727658899963,
-0.934809998307451));
#69448=CARTESIAN_POINT('Ctrl Pts',(-0.575124034692748,0.533937117712032,
-0.918967884879216));
#69449=CARTESIAN_POINT('Ctrl Pts',(-0.760255322534541,0.194597907259556,
-0.90312577145098));
#69450=CARTESIAN_POINT('Ctrl Pts',(-0.760926564298854,-0.191956413532444,
-0.887283658022745));
#69451=CARTESIAN_POINT('Ctrl Pts',(-0.576974897216953,-0.531936527165962,
-0.871441544594511));
#69452=CARTESIAN_POINT('Ctrl Pts',(-0.253032344216126,-0.742853372969652,
-0.855599431166274));
#69453=CARTESIAN_POINT('Ctrl Pts',(0.132303212542429,-0.773532391631306,
-0.83975731773804));
#69454=CARTESIAN_POINT('Ctrl Pts',(0.485538163151441,-0.616529961214717,
-0.823915204309804));
#69455=CARTESIAN_POINT('Ctrl Pts',(0.720967438097831,-0.309939436268682,
-0.808073090881569));
#69456=CARTESIAN_POINT('Ctrl Pts',(0.781469050047366,0.0718514075712125,
-0.792230977453334));
#69457=CARTESIAN_POINT('Ctrl Pts',(0.652363548824324,0.43620901081618,-0.776388864025098));
#69458=CARTESIAN_POINT('Ctrl Pts',(0.364975682836995,0.694729625026577,
-0.760546750596864));
#69459=CARTESIAN_POINT('Ctrl Pts',(-0.0109658956700025,0.784688632569665,
-0.744704637168627));
#69460=CARTESIAN_POINT('Ctrl Pts',(-0.384246829048165,0.684259362609184,
-0.728862523740393));
#69461=CARTESIAN_POINT('Ctrl Pts',(-0.664298309516936,0.417808876072346,
-0.713020410312157));
#69462=CARTESIAN_POINT('Ctrl Pts',(-0.783171705267838,0.0499858081835622,
-0.697178296883922));
#69463=CARTESIAN_POINT('Ctrl Pts',(-0.712024874184065,-0.329965270134697,
-0.681336183455686));
#69464=CARTESIAN_POINT('Ctrl Pts',(-0.46812010611875,-0.629857180001361,
-0.665494070027452));
#69465=CARTESIAN_POINT('Ctrl Pts',(-0.110635789466275,-0.776927424564915,
-0.649651956599216));
#69466=CARTESIAN_POINT('Ctrl Pts',(0.27369198650554,-0.735492486348126,
-0.633809843170981));
#69467=CARTESIAN_POINT('Ctrl Pts',(0.591614128810049,-0.515605686105404,
-0.617967729742745));
#69468=CARTESIAN_POINT('Ctrl Pts',(0.76599348196765,-0.170617954902095,
-0.60212561631451));
#69469=CARTESIAN_POINT('Ctrl Pts',(0.75452054472924,0.215766652968861,-0.586283502886275));
#69470=CARTESIAN_POINT('Ctrl Pts',(0.559978985250664,0.549799997298597,
-0.570441389458039));
#69471=CARTESIAN_POINT('Ctrl Pts',(0.22957024226141,0.750435876554373,-0.554599276029805));
#69472=CARTESIAN_POINT('Ctrl Pts',(-0.156538916378148,0.768994192833109,
-0.538757162601569));
#69473=CARTESIAN_POINT('Ctrl Pts',(-0.50466718245163,0.600972159012604,
-0.522915049173334));
#69474=CARTESIAN_POINT('Ctrl Pts',(-0.730348516593625,0.287136805828302,
-0.507072935745098));
#69475=CARTESIAN_POINT('Ctrl Pts',(-0.778826065336109,-0.0963662851063081,
-0.491230822316863));
#69476=CARTESIAN_POINT('Ctrl Pts',(-0.638337765842564,-0.456488113372826,
-0.475388708888627));
#69477=CARTESIAN_POINT('Ctrl Pts',(-0.342970164344439,-0.705852652698681,
-0.459546595460393));
#69478=CARTESIAN_POINT('Ctrl Pts',(0.0356119710671365,-0.78395681543616,
-0.443704482032157));
#69479=CARTESIAN_POINT('Ctrl Pts',(0.405553606856166,-0.67185026078431,
-0.427862368603922));
#69480=CARTESIAN_POINT('Ctrl Pts',(0.677096145942502,-0.396733298460725,
-0.412020255175687));
#69481=CARTESIAN_POINT('Ctrl Pts',(0.784355473072728,-0.0253573026962391,
-0.396178141747451));
#69482=CARTESIAN_POINT('Ctrl Pts',(0.701307356914353,0.352171111977085,
-0.380336028319216));
#69483=CARTESIAN_POINT('Ctrl Pts',(0.448101685014491,0.644252575325862,
-0.364493914890981));
#69484=CARTESIAN_POINT('Ctrl Pts',(0.0861735156653512,0.780019631902653,
-0.348651801462745));
#69485=CARTESIAN_POINT('Ctrl Pts',(-0.296662854383594,0.726531246309671,
-0.33280968803451));
#69486=CARTESIAN_POINT('Ctrl Pts',(-0.607520189821113,0.496765256041073,
-0.316967574606275));
#69487=CARTESIAN_POINT('Ctrl Pts',(-0.770975464226936,0.146469571011442,
-0.30112546117804));
#69488=CARTESIAN_POINT('Ctrl Pts',(-0.747369672537648,-0.239363890764772,
-0.285283347749805));
#69489=CARTESIAN_POINT('Ctrl Pts',(-0.542430271940636,-0.567120712737478,
-0.269441234321568));
#69490=CARTESIAN_POINT('Ctrl Pts',(-0.205881508420772,-0.7572775609926,
-0.253599120893334));
#69491=CARTESIAN_POINT('Ctrl Pts',(0.180620080446991,-0.763696853658917,
-0.237757007465098));
#69492=CARTESIAN_POINT('Ctrl Pts',(0.523298015026439,-0.584821086775341,
-0.221914894036863));
#69493=CARTESIAN_POINT('Ctrl Pts',(0.739008579394253,-0.264050716247043,
-0.206072780608628));
#69494=CARTESIAN_POINT('Ctrl Pts',(0.775414286343801,0.120786027599504,
-0.190230667180393));
#69495=CARTESIAN_POINT('Ctrl Pts',(0.623681724089946,0.476316584647831,
-0.174388553752157));
#69496=CARTESIAN_POINT('Ctrl Pts',(0.320626268807888,0.7162788588628,-0.158546440323922));
#69497=CARTESIAN_POINT('Ctrl Pts',(-0.060223279451711,0.782451115037967,
-0.142704326895687));
#69498=CARTESIAN_POINT('Ctrl Pts',(-0.426459265784379,0.658777864179818,
-0.126862213467451));
#69499=CARTESIAN_POINT('Ctrl Pts',(-0.689227058061626,0.375266177359453,
-0.111020100039216));
#69500=CARTESIAN_POINT('Ctrl Pts',(-0.784762003573733,0.000703557140667915,
-0.0951779866109806));
#69501=CARTESIAN_POINT('Ctrl Pts',(-0.689903274611894,-0.374028887441819,
-0.0793358731827455));
#69502=CARTESIAN_POINT('Ctrl Pts',(-0.427629588929981,-0.65801278284077,
-0.0634937597545103));
#69503=CARTESIAN_POINT('Ctrl Pts',(-0.0616486583102524,-0.782340136422,
-0.0476516463262753));
#69504=CARTESIAN_POINT('Ctrl Pts',(0.319388156045572,-0.71685708433609,
-0.0318095328980398));
#69505=CARTESIAN_POINT('Ctrl Pts',(0.521593541223493,-0.557227910382347,
-0.0212481239458828));
#69506=CARTESIAN_POINT('Ctrl Pts',(0.597589667152306,-0.458088845993774,
-0.0159674194698044));
#69507=CARTESIAN_POINT('Ctrl Pts',(-0.342067962509744,0.713322310757509,
-2.9089));
#69508=CARTESIAN_POINT('Ctrl Pts',(-0.460406866917156,0.656573843331485,
-2.90361929552392));
#69509=CARTESIAN_POINT('Ctrl Pts',(-0.66818005485177,0.483105216441118,
-2.89305788657176));
#69510=CARTESIAN_POINT('Ctrl Pts',(-0.817739637008241,0.105437811674842,
-2.87721577314354));
#69511=CARTESIAN_POINT('Ctrl Pts',(-0.768878917407871,-0.297709234697778,
-2.86137365971529));
#69512=CARTESIAN_POINT('Ctrl Pts',(-0.533472594856222,-0.628673607988602,
-2.84553154628707));
#69513=CARTESIAN_POINT('Ctrl Pts',(-0.16862683527399,-0.807078059683254,
-2.82968943285882));
#69514=CARTESIAN_POINT('Ctrl Pts',(0.237130924373097,-0.78967485289565,
-2.81384731943059));
#69515=CARTESIAN_POINT('Ctrl Pts',(0.585354731164429,-0.580666968551218,
-2.79800520600235));
#69516=CARTESIAN_POINT('Ctrl Pts',(0.79155399973086,-0.230775758073293,
-2.78216309257412));
#69517=CARTESIAN_POINT('Ctrl Pts',(0.805699488103364,0.175110076068112,
-2.76632097914588));
#69518=CARTESIAN_POINT('Ctrl Pts',(0.624358734712405,0.538508240090762,
-2.75047886571765));
#69519=CARTESIAN_POINT('Ctrl Pts',(0.291530459794522,0.77124909335653,-2.73463675228941));
#69520=CARTESIAN_POINT('Ctrl Pts',(-0.112031612212736,0.816862264866122,
-2.71879463886118));
#69521=CARTESIAN_POINT('Ctrl Pts',(-0.488411541842896,0.664281016055754,
-2.70295252543294));
#69522=CARTESIAN_POINT('Ctrl Pts',(-0.746288638688284,0.350525819364675,
-2.68711041200471));
#69523=CARTESIAN_POINT('Ctrl Pts',(-0.823094408919947,-0.0482771027207467,
-2.67126829857647));
#69524=CARTESIAN_POINT('Ctrl Pts',(-0.700193545740531,-0.43536661135378,
-2.65542618514824));
#69525=CARTESIAN_POINT('Ctrl Pts',(-0.407405368789744,-0.716823513729212,
-2.63958407172));
#69526=CARTESIAN_POINT('Ctrl Pts',(-0.015768804388061,-0.824358193636169,
-2.62374195829176));
#69527=CARTESIAN_POINT('Ctrl Pts',(0.379693730723338,-0.731879605077058,
-2.60789984486353));
#69528=CARTESIAN_POINT('Ctrl Pts',(0.683031526820612,-0.461825745571817,
-2.59205773143529));
#69529=CARTESIAN_POINT('Ctrl Pts',(0.820646015076266,-0.0797195318313355,
-2.57621561800706));
#69530=CARTESIAN_POINT('Ctrl Pts',(0.759147919315163,0.32172895794998,-2.56037350457882));
#69531=CARTESIAN_POINT('Ctrl Pts',(0.513458465714772,0.645116648228309,
-2.54453139115059));
#69532=CARTESIAN_POINT('Ctrl Pts',(0.143189059242546,0.811980282464406,
-2.52868927772235));
#69533=CARTESIAN_POINT('Ctrl Pts',(-0.261822176295599,0.78183389144885,
-2.51284716429412));
#69534=CARTESIAN_POINT('Ctrl Pts',(-0.603307739246953,0.561991866110547,
-2.49700505086588));
#69535=CARTESIAN_POINT('Ctrl Pts',(-0.798413303160151,0.205794273848672,
-2.48116293743765));
#69536=CARTESIAN_POINT('Ctrl Pts',(-0.799800585433026,-0.200334992832333,
-2.46532082400941));
#69537=CARTESIAN_POINT('Ctrl Pts',(-0.607132991049227,-0.557857165402611,
-2.44947871058118));
#69538=CARTESIAN_POINT('Ctrl Pts',(-0.267157280320236,-0.780026969651644,
-2.43363659715294));
#69539=CARTESIAN_POINT('Ctrl Pts',(0.137638554355512,-0.812939551360736,
-2.41779448372471));
#69540=CARTESIAN_POINT('Ctrl Pts',(0.509039273829898,-0.64860936125727,
-2.40195237029647));
#69541=CARTESIAN_POINT('Ctrl Pts',(0.756932264883711,-0.326907681448137,
-2.38611025686824));
#69542=CARTESIAN_POINT('Ctrl Pts',(0.821171480265806,0.0741113068961196,
-2.37026814344));
#69543=CARTESIAN_POINT('Ctrl Pts',(0.686170618534919,0.457148737361488,
-2.35442603001176));
#69544=CARTESIAN_POINT('Ctrl Pts',(0.384684813969298,0.729268592298606,
-2.33858391658353));
#69545=CARTESIAN_POINT('Ctrl Pts',(-0.0101367113822268,0.824446682869273,
-2.32274180315529));
#69546=CARTESIAN_POINT('Ctrl Pts',(-0.402498775822114,0.719590036947071,
-2.30689968972706));
#69547=CARTESIAN_POINT('Ctrl Pts',(-0.697202934380121,0.440139925595871,
-2.29105757629882));
#69548=CARTESIAN_POINT('Ctrl Pts',(-0.822745389508861,0.0538990709910901,
-2.27521546287059));
#69549=CARTESIAN_POINT('Ctrl Pts',(-0.748665891379994,-0.345419265380477,
-2.25937334944235));
#69550=CARTESIAN_POINT('Ctrl Pts',(-0.492938280140658,-0.660928844720641,
-2.24353123601412));
#69551=CARTESIAN_POINT('Ctrl Pts',(-0.117609509694749,-0.816077869471505,
-2.22768912258588));
#69552=CARTESIAN_POINT('Ctrl Pts',(0.286254747362578,-0.77322267518754,
-2.21184700915765));
#69553=CARTESIAN_POINT('Ctrl Pts',(0.620665279699681,-0.542761178039759,
-2.19600489572941));
#69554=CARTESIAN_POINT('Ctrl Pts',(0.804484369006286,-0.180610038027646,
-2.18016278230118));
#69555=CARTESIAN_POINT('Ctrl Pts',(0.793112159578158,0.225362348543543,
-2.16432066887294));
#69556=CARTESIAN_POINT('Ctrl Pts',(0.589307880075637,0.576655276827108,
-2.14847855544471));
#69557=CARTESIAN_POINT('Ctrl Pts',(0.242520374424596,0.788034868391458,
-2.13263644201647));
#69558=CARTESIAN_POINT('Ctrl Pts',(-0.163109625471599,0.808214288348271,
-2.11679432858824));
#69559=CARTESIAN_POINT('Ctrl Pts',(-0.529164487728682,0.632297422688588,
-2.10095221516));
#69560=CARTESIAN_POINT('Ctrl Pts',(-0.766828659521958,0.302966817898509,
-2.08511010173177));
#69561=CARTESIAN_POINT('Ctrl Pts',(-0.818437902561313,-0.0998723458362106,
-2.06926798830353));
#69562=CARTESIAN_POINT('Ctrl Pts',(-0.671470313919026,-0.478479574629131,
-2.05342587487529));
#69563=CARTESIAN_POINT('Ctrl Pts',(-0.361584503761051,-0.740993746567179,
-2.03758376144706));
#69564=CARTESIAN_POINT('Ctrl Pts',(0.0360322202724218,-0.823721290798065,
-2.02174164801882));
#69565=CARTESIAN_POINT('Ctrl Pts',(0.424906480011704,-0.706590099743728,
-2.00589953459059));
#69566=CARTESIAN_POINT('Ctrl Pts',(0.710686073316714,-0.418019606006058,
-1.99005742116235));
#69567=CARTESIAN_POINT('Ctrl Pts',(0.824032561656957,-0.0280254017074349,
-1.97421530773412));
#69568=CARTESIAN_POINT('Ctrl Pts',(0.737444791351247,0.368768579898975,
-1.95837319430588));
#69569=CARTESIAN_POINT('Ctrl Pts',(0.471931473061532,0.676088581877968,
-1.94253108087765));
#69570=CARTESIAN_POINT('Ctrl Pts',(0.0919138577468047,0.819369836255821,
-1.92668896744941));
#69571=CARTESIAN_POINT('Ctrl Pts',(-0.310404731901931,0.76384814474127,
-1.91084685402118));
#69572=CARTESIAN_POINT('Ctrl Pts',(-0.637410108407462,0.522994684018659,
-1.89500474059294));
#69573=CARTESIAN_POINT('Ctrl Pts',(-0.809761259573127,0.155247506602632,
-1.87916262716471));
#69574=CARTESIAN_POINT('Ctrl Pts',(-0.78564078492412,-0.250167229819576,
-1.86332051373647));
#69575=CARTESIAN_POINT('Ctrl Pts',(-0.570901012926016,-0.594884122541389,
-1.84747840030824));
#69576=CARTESIAN_POINT('Ctrl Pts',(-0.217644055939408,-0.795264830560256,
-1.83163628688));
#69577=CARTESIAN_POINT('Ctrl Pts',(0.18841967713557,-0.802691167934417,
-1.81579417345177));
#69578=CARTESIAN_POINT('Ctrl Pts',(0.548767318134455,-0.615361289292159,
-1.79995206002353));
#69579=CARTESIAN_POINT('Ctrl Pts',(0.775968052050294,-0.278726869908628,
-1.78410994659529));
#69580=CARTESIAN_POINT('Ctrl Pts',(0.81489637485211,0.12553479224773,-1.76826783316706));
#69581=CARTESIAN_POINT('Ctrl Pts',(0.656107143566346,0.499338063813484,
-1.75242571973882));
#69582=CARTESIAN_POINT('Ctrl Pts',(0.338127242584864,0.751987402576497,
-1.73658360631059));
#69583=CARTESIAN_POINT('Ctrl Pts',(-0.0618921586783426,0.822182733038054,
-1.72074149288235));
#69584=CARTESIAN_POINT('Ctrl Pts',(-0.446894722698526,0.692892627061363,
-1.70489937945412));
#69585=CARTESIAN_POINT('Ctrl Pts',(-0.72346763328869,0.395486623535428,
-1.68905726602588));
#69586=CARTESIAN_POINT('Ctrl Pts',(-0.82450626083418,0.00212406615444509,
-1.67321515259765));
#69587=CARTESIAN_POINT('Ctrl Pts',(-0.725495696540265,-0.391753851433967,
-1.65737303916941));
#69588=CARTESIAN_POINT('Ctrl Pts',(-0.450458782089819,-0.690580894211494,
-1.64153092574118));
#69589=CARTESIAN_POINT('Ctrl Pts',(-0.0661274697740855,-0.821852933044026,
-1.62568881231294));
#69590=CARTESIAN_POINT('Ctrl Pts',(0.334248289400433,-0.753719554505967,
-1.60984669888471));
#69591=CARTESIAN_POINT('Ctrl Pts',(0.653525695118409,-0.502711897245121,
-1.59400458545647));
#69592=CARTESIAN_POINT('Ctrl Pts',(0.814238765591132,-0.129731717095008,
-1.57816247202824));
#69593=CARTESIAN_POINT('Ctrl Pts',(0.777393837103336,0.274725149641497,
-1.5623203586));
#69594=CARTESIAN_POINT('Ctrl Pts',(0.551930560592181,0.612525707294143,
-1.54647824517177));
#69595=CARTESIAN_POINT('Ctrl Pts',(0.192552882404771,0.801709718844298,
-1.53063613174353));
#69596=CARTESIAN_POINT('Ctrl Pts',(-0.2135437236322,0.796375642463458,-1.51479401831529));
#69597=CARTESIAN_POINT('Ctrl Pts',(-0.567828413417889,0.597817680172738,
-1.49895190488706));
#69598=CARTESIAN_POINT('Ctrl Pts',(-0.784341420193217,0.254211766802947,
-1.48310979145882));
#69599=CARTESIAN_POINT('Ctrl Pts',(-0.810550393282888,-0.15107331253648,
-1.46726767803059));
#69600=CARTESIAN_POINT('Ctrl Pts',(-0.64009627377542,-0.519703613717099,
-1.45142556460236));
#69601=CARTESIAN_POINT('Ctrl Pts',(-0.314336187108121,-0.762238707549098,
-1.43558345117412));
#69602=CARTESIAN_POINT('Ctrl Pts',(0.0876909980445682,-0.819832528431104,
-1.41974133774588));
#69603=CARTESIAN_POINT('Ctrl Pts',(0.468441797408921,-0.678511140845962,
-1.40389922431765));
#69604=CARTESIAN_POINT('Ctrl Pts',(0.735534996525771,-0.372563222416845,
-1.38805711088941));
#69605=CARTESIAN_POINT('Ctrl Pts',(0.824166019411586,0.0237793662457898,
-1.37221499746118));
#69606=CARTESIAN_POINT('Ctrl Pts',(0.712830402919816,0.414352389259386,
-1.35637288403294));
#69607=CARTESIAN_POINT('Ctrl Pts',(0.428541404754035,0.704391475121063,
-1.34053077060471));
#69608=CARTESIAN_POINT('Ctrl Pts',(0.0402758017241118,0.823524708559051,
-1.32468865717647));
#69609=CARTESIAN_POINT('Ctrl Pts',(-0.357761881844586,0.742846903278738,
-1.30884654374824));
#69610=CARTESIAN_POINT('Ctrl Pts',(-0.668996130759501,0.481932840591515,
-1.29300443032));
#69611=CARTESIAN_POINT('Ctrl Pts',(-0.817912466931429,0.104087858321388,
-1.27716231689177));
#69612=CARTESIAN_POINT('Ctrl Pts',(-0.768379457382846,-0.299011864787725,
-1.26132020346353));
#69613=CARTESIAN_POINT('Ctrl Pts',(-0.532415250429014,-0.629562615569254,
-1.2454780900353));
#69614=CARTESIAN_POINT('Ctrl Pts',(-0.167271623462604,-0.807363170943519,
-1.22963597660706));
#69615=CARTESIAN_POINT('Ctrl Pts',(0.238456962867854,-0.789273946530371,
-1.21379386317883));
#69616=CARTESIAN_POINT('Ctrl Pts',(0.586328956742687,-0.57968391412633,
-1.19795174975059));
#69617=CARTESIAN_POINT('Ctrl Pts',(0.791940497883369,-0.22944570953503,
-1.18210963632235));
#69618=CARTESIAN_POINT('Ctrl Pts',(0.805404248143504,0.176462695446335,
-1.16626752289412));
#69619=CARTESIAN_POINT('Ctrl Pts',(0.62345351024424,0.539556119765059,-1.15042540946588));
#69620=CARTESIAN_POINT('Ctrl Pts',(0.290234823515067,0.771737541545678,
-1.13458329603765));
#69621=CARTESIAN_POINT('Ctrl Pts',(-0.113403270131766,0.81667299706505,
-1.11874118260941));
#69622=CARTESIAN_POINT('Ctrl Pts',(-0.489526433183827,0.663459838291745,
-1.10289906918118));
#69623=CARTESIAN_POINT('Ctrl Pts',(-0.746876250302318,0.349272032298804,
-1.08705695575294));
#69624=CARTESIAN_POINT('Ctrl Pts',(-0.823012173270564,-0.0496593240011921,
-1.07121484232471));
#69625=CARTESIAN_POINT('Ctrl Pts',(-0.699461413483729,-0.436541884427066,
-1.05537272889647));
#69626=CARTESIAN_POINT('Ctrl Pts',(-0.406200977570603,-0.717506691001887,
-1.03953061546824));
#69627=CARTESIAN_POINT('Ctrl Pts',(-0.0143843739879145,-0.824383512448402,
-1.02368850204));
#69628=CARTESIAN_POINT('Ctrl Pts',(0.380922296957617,-0.731240924382876,
-1.00784638861177));
#69629=CARTESIAN_POINT('Ctrl Pts',(0.683806143141474,-0.460678026840626,
-0.99200427518353));
#69630=CARTESIAN_POINT('Ctrl Pts',(0.820778736969435,-0.078341245526529,
-0.976162161755294));
#69631=CARTESIAN_POINT('Ctrl Pts',(0.758606544627331,0.323003399765964,
-0.96032004832706));
#69632=CARTESIAN_POINT('Ctrl Pts',(0.51237434766714,0.645978028778427,-0.944477934898824));
#69633=CARTESIAN_POINT('Ctrl Pts',(0.141825236404382,0.812219605852155,
-0.928635821470589));
#69634=CARTESIAN_POINT('Ctrl Pts',(-0.263134800854775,0.781393090826191,
-0.912793708042353));
#69635=CARTESIAN_POINT('Ctrl Pts',(-0.604250684641326,0.56097789254326,
-0.896951594614119));
#69636=CARTESIAN_POINT('Ctrl Pts',(-0.798757783421676,0.20445314679672,
-0.881109481185882));
#69637=CARTESIAN_POINT('Ctrl Pts',(-0.799463019633659,-0.201677876947427,
-0.865267367757648));
#69638=CARTESIAN_POINT('Ctrl Pts',(-0.606195282467129,-0.558875983851863,
-0.849425254329413));
#69639=CARTESIAN_POINT('Ctrl Pts',(-0.265846944321634,-0.780474527455342,
-0.833583140901176));
#69640=CARTESIAN_POINT('Ctrl Pts',(0.139003592158546,-0.812707257983346,
-0.817741027472943));
#69641=CARTESIAN_POINT('Ctrl Pts',(0.510127815577188,-0.647753577825886,
-0.801898914044706));
#69642=CARTESIAN_POINT('Ctrl Pts',(0.75748019869741,-0.325636045905737,
-0.786056800616472));
#69643=CARTESIAN_POINT('Ctrl Pts',(0.821045861471253,0.0754902587935505,
-0.770214687188235));
#69644=CARTESIAN_POINT('Ctrl Pts',(0.685401925904101,0.458300431789825,
-0.754372573760001));
#69645=CARTESIAN_POINT('Ctrl Pts',(0.383459554684601,0.729913594703426,
-0.738530460331766));
#69646=CARTESIAN_POINT('Ctrl Pts',(-0.0115212537932657,0.824428496913359,
-0.722688346903529));
#69647=CARTESIAN_POINT('Ctrl Pts',(-0.403706671114261,0.718913075072106,
-0.706846233475295));
#69648=CARTESIAN_POINT('Ctrl Pts',(-0.6979411120353,0.438968438435745,-0.691004120047059));
#69649=CARTESIAN_POINT('Ctrl Pts',(-0.822834746165019,0.0525172953924725,
-0.675162006618824));
#69650=CARTESIAN_POINT('Ctrl Pts',(-0.748084746514252,-0.346676070481504,
-0.659319893190589));
#69651=CARTESIAN_POINT('Ctrl Pts',(-0.491827636394545,-0.661755741864282,
-0.643477779762354));
#69652=CARTESIAN_POINT('Ctrl Pts',(-0.11623884153363,-0.816274229368237,
-0.627635666334118));
#69653=CARTESIAN_POINT('Ctrl Pts',(0.287552875989903,-0.772740855217146,
-0.611793552905883));
#69654=CARTESIAN_POINT('Ctrl Pts',(0.621575905044439,-0.541718081736226,
-0.595951439477648));
#69655=CARTESIAN_POINT('Ctrl Pts',(0.804786546882918,-0.179258750882796,
-0.580109326049412));
#69656=CARTESIAN_POINT('Ctrl Pts',(0.792732572847805,0.226693964978968,
-0.564267212621177));
#69657=CARTESIAN_POINT('Ctrl Pts',(0.588338627515784,0.577644133688412,
-0.548425099192942));
#69658=CARTESIAN_POINT('Ctrl Pts',(0.241196624887782,0.788441040252554,
-0.532582985764707));
#69659=CARTESIAN_POINT('Ctrl Pts',(-0.164466691858981,0.807939226105988,
-0.516740872336471));
#69660=CARTESIAN_POINT('Ctrl Pts',(-0.530225607203705,0.631407864440488,
-0.500898758908237));
#69661=CARTESIAN_POINT('Ctrl Pts',(-0.767336373647194,0.301678596339951,
-0.48505664548));
#69662=CARTESIAN_POINT('Ctrl Pts',(-0.818269025128244,-0.101246670699364,
-0.469214532051766));
#69663=CARTESIAN_POINT('Ctrl Pts',(-0.670665819502484,-0.479606551625889,
-0.453372418623529));
#69664=CARTESIAN_POINT('Ctrl Pts',(-0.360339586098838,-0.741599938310583,
-0.437530305195295));
#69665=CARTESIAN_POINT('Ctrl Pts',(0.0374155079612326,-0.823659617545991,
-0.42168819176706));
#69666=CARTESIAN_POINT('Ctrl Pts',(0.426092511909218,-0.705875525219977,
-0.405846078338824));
#69667=CARTESIAN_POINT('Ctrl Pts',(0.711387083609428,-0.416825506767385,
-0.390003964910589));
#69668=CARTESIAN_POINT('Ctrl Pts',(0.824078464847273,-0.0266415009469172,
-0.374161851482353));
#69669=CARTESIAN_POINT('Ctrl Pts',(0.73682445002649,0.370006507616631,-0.358319738054118));
#69670=CARTESIAN_POINT('Ctrl Pts',(0.470795399993314,0.676880179300043,
-0.342477624625883));
#69671=CARTESIAN_POINT('Ctrl Pts',(0.0905376974317523,0.8195230388218,-0.326635511197647));
#69672=CARTESIAN_POINT('Ctrl Pts',(-0.311687083230146,0.763325781073419,
-0.310793397769413));
#69673=CARTESIAN_POINT('Ctrl Pts',(-0.638287514499288,0.521923494693118,
-0.294951284341177));
#69674=CARTESIAN_POINT('Ctrl Pts',(-0.810020837243697,0.153887393369101,
-0.279109170912942));
#69675=CARTESIAN_POINT('Ctrl Pts',(-0.785219551035283,-0.251486264089612,
-0.263267057484706));
#69676=CARTESIAN_POINT('Ctrl Pts',(-0.569901175083765,-0.595842041498009,
-0.247424944056471));
#69677=CARTESIAN_POINT('Ctrl Pts',(-0.21630819599585,-0.79562921577039,
-0.231582830628236));
#69678=CARTESIAN_POINT('Ctrl Pts',(0.189767425262224,-0.802373607857236,
-0.2157407172));
#69679=CARTESIAN_POINT('Ctrl Pts',(0.549799981877126,-0.614438835381788,
-0.199898603771766));
#69680=CARTESIAN_POINT('Ctrl Pts',(0.776435017697278,-0.277423332094875,
-0.18405649034353));
#69681=CARTESIAN_POINT('Ctrl Pts',(0.814684459595264,0.126903129532913,
-0.168214376915295));
#69682=CARTESIAN_POINT('Ctrl Pts',(0.655267535429932,0.500439218356143,
-0.152372263487059));
#69683=CARTESIAN_POINT('Ctrl Pts',(0.336864103661856,0.752554170498509,
-0.136530150058825));
#69684=CARTESIAN_POINT('Ctrl Pts',(-0.0632732343719237,0.822077662277926,
-0.120688036630589));
#69685=CARTESIAN_POINT('Ctrl Pts',(-0.448056919512178,0.692141088608601,
-0.104845923202354));
#69686=CARTESIAN_POINT('Ctrl Pts',(-0.724132355083295,0.394271202234359,
-0.0890038097741183));
#69687=CARTESIAN_POINT('Ctrl Pts',(-0.824505583727274,0.000739188172099202,
-0.0731616963458828));
#69688=CARTESIAN_POINT('Ctrl Pts',(-0.724842818024885,-0.392971250859118,
-0.0573195829176476));
#69689=CARTESIAN_POINT('Ctrl Pts',(-0.449286512642228,-0.691337260399308,
-0.0414774694894125));
#69690=CARTESIAN_POINT('Ctrl Pts',(-0.0647708002867455,-0.821961063247746,
-0.0256353560611774));
#69691=CARTESIAN_POINT('Ctrl Pts',(0.335563287769688,-0.753161679691374,
-0.00979324263294204));
#69692=CARTESIAN_POINT('Ctrl Pts',(0.548009186500381,-0.585448226884957,
0.000768166319215033));
#69693=CARTESIAN_POINT('Ctrl Pts',(0.627854069260509,-0.481288351939895,
0.00604887079529348));
#69694=CARTESIAN_POINT('Ctrl Pts',(-0.79116656670867,1.93884184799344E-7,
-0.0731331508237035));
#69695=CARTESIAN_POINT('Ctrl Pts',(-0.791165138234783,-0.108770838987923,
-0.068755433882469));
#69696=CARTESIAN_POINT('Ctrl Pts',(-0.768256400998376,-0.217542593998915,
-0.0643777169412344));
#69697=CARTESIAN_POINT('Ctrl Pts',(-0.724732793080687,-0.317244732932517,
-0.0599999999999999));
#69698=CARTESIAN_POINT('',(-0.392913737924004,-0.550974480436018,-2.9089));
#69699=CARTESIAN_POINT('Ctrl Pts',(-0.392913737924002,-0.550974480436019,
-2.9089));
#69700=CARTESIAN_POINT('Ctrl Pts',(-0.409359766126388,-0.541179376730804,
-2.9089));
#69701=CARTESIAN_POINT('Ctrl Pts',(-0.425363363493956,-0.530696820512708,
-2.9089));
#69702=CARTESIAN_POINT('Ctrl Pts',(-0.440878330451655,-0.51955234426649,
-2.9089));
#69703=CARTESIAN_POINT('Ctrl Pts',(-0.464344956425318,-0.502696152664185,
-2.9089));
#69704=CARTESIAN_POINT('Ctrl Pts',(-0.486694654013419,-0.484326991024549,
-2.9089));
#69705=CARTESIAN_POINT('Ctrl Pts',(-0.507833441829143,-0.464597152324595,
-2.9089));
#69706=CARTESIAN_POINT('Ctrl Pts',(-0.515025378158515,-0.457884575191231,
-2.9089));
#69707=CARTESIAN_POINT('Ctrl Pts',(-0.522077024083522,-0.451014259706751,
-2.9089));
#69708=CARTESIAN_POINT('Ctrl Pts',(-0.528984244396564,-0.44399152039105,
-2.9089));
#69709=CARTESIAN_POINT('Ctrl Pts',(-0.534887861339321,-0.437989169093459,
-2.9089));
#69710=CARTESIAN_POINT('Ctrl Pts',(-0.540684793267629,-0.431876452002257,
-2.9089));
#69711=CARTESIAN_POINT('Ctrl Pts',(-0.546364587743398,-0.425665844041185,
-2.9089));
#69712=CARTESIAN_POINT('Ctrl Pts',(-0.569500373077027,-0.400367870110675,
-2.9089));
#69713=CARTESIAN_POINT('Ctrl Pts',(-0.590733194895916,-0.373411181702835,
-2.9089));
#69714=CARTESIAN_POINT('Ctrl Pts',(-0.609906853654402,-0.345037909562405,
-2.9089));
#69715=CARTESIAN_POINT('Ctrl Pts',(-0.61723018226465,-0.334200812780321,
-2.9089));
#69716=CARTESIAN_POINT('Ctrl Pts',(-0.624252776542584,-0.323156582520568,
-2.9089));
#69717=CARTESIAN_POINT('Ctrl Pts',(-0.630964508213922,-0.311917121560154,
-2.9089));
#69718=CARTESIAN_POINT('Ctrl Pts',(-0.635277847467634,-0.304694006792599,
-2.9089));
#69719=CARTESIAN_POINT('Ctrl Pts',(-0.639463497654007,-0.297388934158588,
-2.9089));
#69720=CARTESIAN_POINT('Ctrl Pts',(-0.643516328199236,-0.290008987870708,
-2.9089));
#69721=CARTESIAN_POINT('Ctrl Pts',(-0.649668223487523,-0.278806778380437,
-2.9089));
#69722=CARTESIAN_POINT('Ctrl Pts',(-0.655504229181834,-0.267450350249753,
-2.9089));
#69723=CARTESIAN_POINT('Ctrl Pts',(-0.661017337842235,-0.25595243742994,
-2.9089));
#69724=CARTESIAN_POINT('Ctrl Pts',(-0.67572645112639,-0.225275715345224,
-2.9089));
#69725=CARTESIAN_POINT('Ctrl Pts',(-0.688140193377098,-0.193594372368486,
-2.9089));
#69726=CARTESIAN_POINT('Ctrl Pts',(-0.698261510376344,-0.161185561047533,
-2.9089));
#69727=CARTESIAN_POINT('Ctrl Pts',(-0.705141449214773,-0.139155756059611,
-2.9089));
#69728=CARTESIAN_POINT('Ctrl Pts',(-0.710961336057706,-0.116788935860317,
-2.9089));
#69729=CARTESIAN_POINT('Ctrl Pts',(-0.715710431828713,-0.0941649192640481,
-2.9089));
#69730=CARTESIAN_POINT('Ctrl Pts',(-0.719357292099036,-0.0767917957773035,
-2.9089));
#69731=CARTESIAN_POINT('Ctrl Pts',(-0.722372543094714,-0.0592668759475071,
-2.9089));
#69732=CARTESIAN_POINT('Ctrl Pts',(-0.72474721180396,-0.041625047399535,
-2.9089));
#69733=CARTESIAN_POINT('Ctrl Pts',(-0.726025787999834,-0.0321262815526122,
-2.9089));
#69734=CARTESIAN_POINT('Ctrl Pts',(-0.727118789016985,-0.0225894136711933,
-2.9089));
#69735=CARTESIAN_POINT('Ctrl Pts',(-0.728022317948154,-0.0130479136047751,
-2.9089));
#69736=CARTESIAN_POINT('Ctrl Pts',(-0.731403409697682,0.0226572929910528,
-2.9089));
#69737=CARTESIAN_POINT('Ctrl Pts',(-0.732147066811708,0.0584956871592241,
-2.9089));
#69738=CARTESIAN_POINT('Ctrl Pts',(-0.730236974451504,0.0941715601595828,
-2.9089));
#69739=CARTESIAN_POINT('Ctrl Pts',(-0.728572567971089,0.125258619326665,
-2.9089));
#69740=CARTESIAN_POINT('Ctrl Pts',(-0.72489265561043,0.156223354823441,
-2.9089));
#69741=CARTESIAN_POINT('Ctrl Pts',(-0.719274620967193,0.186892382374801,
-2.9089));
#69742=CARTESIAN_POINT('Ctrl Pts',(-0.71600434450303,0.204744924295439,
-2.9089));
#69743=CARTESIAN_POINT('Ctrl Pts',(-0.712076711511137,0.222497338567289,
-2.9089));
#69744=CARTESIAN_POINT('Ctrl Pts',(-0.707501869156712,0.240115064096392,
-2.9089));
#69745=CARTESIAN_POINT('Ctrl Pts',(-0.70486229707856,0.250280060567185,
-2.9089));
#69746=CARTESIAN_POINT('Ctrl Pts',(-0.702005320648755,0.260405624416952,
-2.9089));
#69747=CARTESIAN_POINT('Ctrl Pts',(-0.69894255661829,0.270453695927041,
-2.9089));
#69748=CARTESIAN_POINT('Ctrl Pts',(-0.688468965167679,0.304814617896998,
-2.9089));
#69749=CARTESIAN_POINT('Ctrl Pts',(-0.675580529064114,0.33832823878394,
-2.9089));
#69750=CARTESIAN_POINT('Ctrl Pts',(-0.660407686502252,0.370740116386383,
-2.9089));
#69751=CARTESIAN_POINT('Ctrl Pts',(-0.648075258027009,0.397084366690881,
-2.9089));
#69752=CARTESIAN_POINT('Ctrl Pts',(-0.634232555647159,0.422701237310616,
-2.9089));
#69753=CARTESIAN_POINT('Ctrl Pts',(-0.618924570005842,0.447450319236685,
-2.9089));
#69754=CARTESIAN_POINT('Ctrl Pts',(-0.610065535171487,0.461773103699558,
-2.9089));
#69755=CARTESIAN_POINT('Ctrl Pts',(-0.600715341027939,0.475805141443812,
-2.9089));
#69756=CARTESIAN_POINT('Ctrl Pts',(-0.590894184902779,0.489528828314774,
-2.9089));
#69757=CARTESIAN_POINT('Ctrl Pts',(-0.585545297999762,0.497003146819615,
-2.9089));
#69758=CARTESIAN_POINT('Ctrl Pts',(-0.580056674884228,0.504385979354654,
-2.9089));
#69759=CARTESIAN_POINT('Ctrl Pts',(-0.574431315468417,0.511674297783051,
-2.9089));
#69760=CARTESIAN_POINT('Ctrl Pts',(-0.569921668564276,0.517517078698459,
-2.9089));
#69761=CARTESIAN_POINT('Ctrl Pts',(-0.565324592131169,0.523298328689192,
-2.9089));
#69762=CARTESIAN_POINT('Ctrl Pts',(-0.560650192799266,0.529006583378885,
-2.9089));
#69763=CARTESIAN_POINT('Ctrl Pts',(-0.537633044250205,0.557114525559133,
-2.9089));
#69764=CARTESIAN_POINT('Ctrl Pts',(-0.512694828279584,0.583520233685232,
-2.9089));
#69765=CARTESIAN_POINT('Ctrl Pts',(-0.486073668914314,0.608074069631979,
-2.9089));
#69766=CARTESIAN_POINT('Ctrl Pts',(-0.45923537508389,0.632828177999722,
-2.9089));
#69767=CARTESIAN_POINT('Ctrl Pts',(-0.43068580735773,0.655701030012639,
-2.9089));
#69768=CARTESIAN_POINT('Ctrl Pts',(-0.400624822626115,0.676511476791734,
-2.9089));
#69769=CARTESIAN_POINT('Ctrl Pts',(-0.381691858478924,0.689618281052249,
-2.9089));
#69770=CARTESIAN_POINT('Ctrl Pts',(-0.362158516231663,0.701906388619064,
-2.9089));
#69771=CARTESIAN_POINT('Ctrl Pts',(-0.342067962509744,0.713322310757509,
-2.9089));
#69772=CARTESIAN_POINT('Ctrl Pts',(-0.392913737924004,-0.550974480436018,
-2.9089));
#69773=CARTESIAN_POINT('Ctrl Pts',(-0.316929799842835,-0.605044757612097,
-2.90451276788471));
#69774=CARTESIAN_POINT('Ctrl Pts',(-0.124667012097903,-0.689527912099726,
-2.89484483129333));
#69775=CARTESIAN_POINT('Ctrl Pts',(0.202839712455166,-0.675480941669175,
-2.87989619022589));
#69776=CARTESIAN_POINT('Ctrl Pts',(0.500707301958,-0.496697430942489,-2.86405407679764));
#69777=CARTESIAN_POINT('Ctrl Pts',(0.677088347387025,-0.197403558953597,
-2.84821196336941));
#69778=CARTESIAN_POINT('Ctrl Pts',(0.689188274048217,0.149787622898873,
-2.83236984994118));
#69779=CARTESIAN_POINT('Ctrl Pts',(0.534070984426596,0.460635224458885,
-2.81652773651294));
#69780=CARTESIAN_POINT('Ctrl Pts',(0.249372597829536,0.659719708601146,
-2.80068562308471));
#69781=CARTESIAN_POINT('Ctrl Pts',(-0.095830858278809,0.69873681536456,
-2.78484350965647));
#69782=CARTESIAN_POINT('Ctrl Pts',(-0.417782948255712,0.568220153665686,
-2.76900139622824));
#69783=CARTESIAN_POINT('Ctrl Pts',(-0.629713345155285,0.31036761779697,
-2.75378090021574));
#69784=CARTESIAN_POINT('Ctrl Pts',(-0.676654539125682,0.099017931234991,
-2.74384110867933));
#69785=CARTESIAN_POINT('Ctrl Pts',(-0.676738003850817,-1.23232206217291E-5,
-2.739182021619));
#69786=CARTESIAN_POINT('Origin',(-1.87869726832665E-16,-4.25270154953079E-17,
-2.9089));
#69787=CARTESIAN_POINT('',(-0.7911,-9.68818082805471E-17,-2.9089));
#69788=CARTESIAN_POINT('Origin',(0.,0.,-2.9089));
#69789=CARTESIAN_POINT('Origin',(0.,0.,-2.9089));
#69790=CARTESIAN_POINT('',(0.392888236737279,-0.550964357679762,-2.9089));
#69791=CARTESIAN_POINT('Ctrl Pts',(0.342095308501471,0.713339076749545,
-2.9089));
#69792=CARTESIAN_POINT('Ctrl Pts',(0.361421457667255,0.702382391769599,
-2.9089));
#69793=CARTESIAN_POINT('Ctrl Pts',(0.380253116542679,0.690624130244962,
-2.9089));
#69794=CARTESIAN_POINT('Ctrl Pts',(0.398533666067781,0.67808073602098,-2.9089));
#69795=CARTESIAN_POINT('Ctrl Pts',(0.425013708871964,0.659911171943888,
-2.9089));
#69796=CARTESIAN_POINT('Ctrl Pts',(0.450338555601534,0.640094850049735,
-2.9089));
#69797=CARTESIAN_POINT('Ctrl Pts',(0.474378541812238,0.618766150097485,
-2.9089));
#69798=CARTESIAN_POINT('Ctrl Pts',(0.484755880862577,0.609559191783637,
-2.9089));
#69799=CARTESIAN_POINT('Ctrl Pts',(0.494893503862243,0.600070177957475,
-2.9089));
#69800=CARTESIAN_POINT('Ctrl Pts',(0.504779505517662,0.590308982482977,
-2.9089));
#69801=CARTESIAN_POINT('Ctrl Pts',(0.511746361070153,0.58343008024719,-2.9089));
#69802=CARTESIAN_POINT('Ctrl Pts',(0.518582035916023,0.576422022636668,
-2.9089));
#69803=CARTESIAN_POINT('Ctrl Pts',(0.525279345939323,0.56929274522698,-2.9089));
#69804=CARTESIAN_POINT('Ctrl Pts',(0.550202482175477,0.54276210060566,-2.9089));
#69805=CARTESIAN_POINT('Ctrl Pts',(0.573230055554725,0.514538002482786,
-2.9089));
#69806=CARTESIAN_POINT('Ctrl Pts',(0.594163530853824,0.484814447194274,
-2.9089));
#69807=CARTESIAN_POINT('Ctrl Pts',(0.601840751795605,0.473913519476122,
-2.9089));
#69808=CARTESIAN_POINT('Ctrl Pts',(0.609235863492435,0.462810666846166,
-2.9089));
#69809=CARTESIAN_POINT('Ctrl Pts',(0.61633739280612,0.451514753928317,-2.9089));
#69810=CARTESIAN_POINT('Ctrl Pts',(0.620979176071088,0.444131389412231,
-2.9089));
#69811=CARTESIAN_POINT('Ctrl Pts',(0.625495511580747,0.436665536531298,
-2.9089));
#69812=CARTESIAN_POINT('Ctrl Pts',(0.629882962628105,0.429119616277332,
-2.9089));
#69813=CARTESIAN_POINT('Ctrl Pts',(0.633948112087592,0.42212801835165,-2.9089));
#69814=CARTESIAN_POINT('Ctrl Pts',(0.637897862824706,0.415075813183006,
-2.9089));
#69815=CARTESIAN_POINT('Ctrl Pts',(0.641729261349816,0.407967103368741,
-2.9089));
#69816=CARTESIAN_POINT('Ctrl Pts',(0.64468657514332,0.402480155078196,-2.9089));
#69817=CARTESIAN_POINT('Ctrl Pts',(0.647573584485386,0.396959182713758,
-2.9089));
#69818=CARTESIAN_POINT('Ctrl Pts',(0.650389374318831,0.391405199216917,
-2.9089));
#69819=CARTESIAN_POINT('Ctrl Pts',(0.666501897875371,0.359624173210447,
-2.9089));
#69820=CARTESIAN_POINT('Ctrl Pts',(0.680286508535265,0.326763593217329,
-2.9089));
#69821=CARTESIAN_POINT('Ctrl Pts',(0.691692293406641,0.293090804439526,
-2.9089));
#69822=CARTESIAN_POINT('Ctrl Pts',(0.702996182480478,0.259718838069524,
-2.9089));
#69823=CARTESIAN_POINT('Ctrl Pts',(0.711963660398992,0.22554786022234,-2.9089));
#69824=CARTESIAN_POINT('Ctrl Pts',(0.718494894315197,0.190832889778513,
-2.9089));
#69825=CARTESIAN_POINT('Ctrl Pts',(0.720554421264328,0.17988604296754,-2.9089));
#69826=CARTESIAN_POINT('Ctrl Pts',(0.722371313086546,0.168885139159948,
-2.9089));
#69827=CARTESIAN_POINT('Ctrl Pts',(0.72394136251251,0.157838367402538,-2.9089));
#69828=CARTESIAN_POINT('Ctrl Pts',(0.724918609600457,0.150962516647377,
-2.9089));
#69829=CARTESIAN_POINT('Ctrl Pts',(0.725799613851594,0.144072570993966,
-2.9089));
#69830=CARTESIAN_POINT('Ctrl Pts',(0.726582863853827,0.137178847898393,
-2.9089));
#69831=CARTESIAN_POINT('Ctrl Pts',(0.730549180008782,0.102269578567019,
-2.9089));
#69832=CARTESIAN_POINT('Ctrl Pts',(0.732022348457187,0.0671998437829258,
-2.9089));
#69833=CARTESIAN_POINT('Ctrl Pts',(0.730931128253835,0.0322245814176823,
-2.9089));
#69834=CARTESIAN_POINT('Ctrl Pts',(0.730000903408154,0.00240946441705488,
-2.9089));
#69835=CARTESIAN_POINT('Ctrl Pts',(0.727206070274835,-0.0273375730699786,
-2.9089));
#69836=CARTESIAN_POINT('Ctrl Pts',(0.722582103198713,-0.0568465663805478,
-2.9089));
#69837=CARTESIAN_POINT('Ctrl Pts',(0.720073144499858,-0.0728581089028451,
-2.9089));
#69838=CARTESIAN_POINT('Ctrl Pts',(0.717025201034188,-0.0887994130225833,
-2.9089));
#69839=CARTESIAN_POINT('Ctrl Pts',(0.713440842181997,-0.104641669857954,
-2.9089));
#69840=CARTESIAN_POINT('Ctrl Pts',(0.711820150259532,-0.111804852660087,
-2.9089));
#69841=CARTESIAN_POINT('Ctrl Pts',(0.710089762375051,-0.118947765994846,
-2.9089));
#69842=CARTESIAN_POINT('Ctrl Pts',(0.708249780343376,-0.126067638780641,
-2.9089));
#69843=CARTESIAN_POINT('Ctrl Pts',(0.706460247497159,-0.132992296734754,
-2.9089));
#69844=CARTESIAN_POINT('Ctrl Pts',(0.704569208219147,-0.139886700115112,
-2.9089));
#69845=CARTESIAN_POINT('Ctrl Pts',(0.702578191106992,-0.146746082325932,
-2.9089));
#69846=CARTESIAN_POINT('Ctrl Pts',(0.693113370508214,-0.179353949755858,
-2.9089));
#69847=CARTESIAN_POINT('Ctrl Pts',(0.681388128385,-0.21119079851327,-2.9089));
#69848=CARTESIAN_POINT('Ctrl Pts',(0.667466886654037,-0.242007940169088,
-2.9089));
#69849=CARTESIAN_POINT('Ctrl Pts',(0.657168215657122,-0.264805877961715,
-2.9089));
#69850=CARTESIAN_POINT('Ctrl Pts',(0.64566666415709,-0.287045565613572,
-2.9089));
#69851=CARTESIAN_POINT('Ctrl Pts',(0.632973022387535,-0.308616041115058,
-2.9089));
#69852=CARTESIAN_POINT('Ctrl Pts',(0.624870735660704,-0.322384365487209,
-2.9089));
#69853=CARTESIAN_POINT('Ctrl Pts',(0.616282481939985,-0.335879827360128,
-2.9089));
#69854=CARTESIAN_POINT('Ctrl Pts',(0.607225187511364,-0.349079425631144,
-2.9089));
#69855=CARTESIAN_POINT('Ctrl Pts',(0.602385167740514,-0.356133001851115,
-2.9089));
#69856=CARTESIAN_POINT('Ctrl Pts',(0.597411183937436,-0.363102055610617,
-2.9089));
#69857=CARTESIAN_POINT('Ctrl Pts',(0.592305668509312,-0.369982813438398,
-2.9089));
#69858=CARTESIAN_POINT('Ctrl Pts',(0.58851755331426,-0.375088096861362,
-2.9089));
#69859=CARTESIAN_POINT('Ctrl Pts',(0.584658275650617,-0.380142949743923,
-2.9089));
#69860=CARTESIAN_POINT('Ctrl Pts',(0.580734572874794,-0.385139090101267,
-2.9089));
#69861=CARTESIAN_POINT('Ctrl Pts',(0.560140903620934,-0.411361479498082,
-2.9089));
#69862=CARTESIAN_POINT('Ctrl Pts',(0.537733933544869,-0.43602603165254,
-2.9089));
#69863=CARTESIAN_POINT('Ctrl Pts',(0.513699242000695,-0.458953879868942,
-2.9089));
#69864=CARTESIAN_POINT('Ctrl Pts',(0.490112295372544,-0.481454602675586,
-2.9089));
#69865=CARTESIAN_POINT('Ctrl Pts',(0.464956687258441,-0.502283358877662,
-2.9089));
#69866=CARTESIAN_POINT('Ctrl Pts',(0.43838137497774,-0.52122970548998,-2.9089));
#69867=CARTESIAN_POINT('Ctrl Pts',(0.423646031374266,-0.53173497912192,
-2.9089));
#69868=CARTESIAN_POINT('Ctrl Pts',(0.408473826265608,-0.541660727795806,
-2.9089));
#69869=CARTESIAN_POINT('Ctrl Pts',(0.392888236737283,-0.550964357679758,
-2.9089));
#69870=CARTESIAN_POINT('Origin',(0.,0.,-2.9089));
#69871=CARTESIAN_POINT('Origin',(0.,0.,-3.278617978381));
#69872=CARTESIAN_POINT('Ctrl Pts',(0.392888236737278,-0.550964357679762,
-2.9089));
#69873=CARTESIAN_POINT('Ctrl Pts',(0.484292245096581,-0.485784897022383,
-2.90361929552392));
#69874=CARTESIAN_POINT('Ctrl Pts',(0.633945837478465,-0.309125594940106,
-2.89305788657177));
#69875=CARTESIAN_POINT('Ctrl Pts',(0.704592787855342,0.0310787463577468,
-2.87721577314353));
#69876=CARTESIAN_POINT('Ctrl Pts',(0.604289094090405,0.363654317141465,
-2.8613736597153));
#69877=CARTESIAN_POINT('Ctrl Pts',(0.357365708044879,0.608039989146884,
-2.84553154628705));
#69878=CARTESIAN_POINT('Ctrl Pts',(0.0237357764082632,0.704875616667608,
-2.82968943285883));
#69879=CARTESIAN_POINT('Ctrl Pts',(-0.315653531008585,0.630699052042456,
-2.81384731943059));
#69880=CARTESIAN_POINT('Ctrl Pts',(-0.578455917520507,0.403490890783857,
-2.79800520600235));
#69881=CARTESIAN_POINT('Ctrl Pts',(-0.669224793849843,0.162504610084219,
-2.78626209231916));
#69882=CARTESIAN_POINT('Ctrl Pts',(-0.676728171233119,0.0251386911605121,
-2.77979968311204));
#69883=CARTESIAN_POINT('Ctrl Pts',(-0.676702457484846,1.74000875470086E-5,
-2.778617978381));
#69884=CARTESIAN_POINT('Ctrl Pts',(0.459308237155098,-0.644108029201217,
-2.97494887079529));
#69885=CARTESIAN_POINT('Ctrl Pts',(0.566164615185311,-0.567909608444529,
-2.96966816631922));
#69886=CARTESIAN_POINT('Ctrl Pts',(0.74111800211203,-0.361385042348344,
-2.95910675736706));
#69887=CARTESIAN_POINT('Ctrl Pts',(0.823708222953097,0.0363327859370564,
-2.94326464393882));
#69888=CARTESIAN_POINT('Ctrl Pts',(0.706447616868514,0.425132156480872,
-2.9274225305106));
#69889=CARTESIAN_POINT('Ctrl Pts',(0.417780422098877,0.710832622157672,
-2.91158041708234));
#69890=CARTESIAN_POINT('Ctrl Pts',(0.0277484449779586,0.824038865591465,
-2.89573830365413));
#69891=CARTESIAN_POINT('Ctrl Pts',(-0.369016563293757,0.737322329053924,
-2.87989619022588));
#69892=CARTESIAN_POINT('Ctrl Pts',(-0.676247194252207,0.471703330425765,
-2.86405407679765));
#69893=CARTESIAN_POINT('Ctrl Pts',(-0.819400710647197,0.0916387655639853,
-2.84821196336941));
#69894=CARTESIAN_POINT('Ctrl Pts',(-0.763743730503373,-0.310661748928857,
-2.83236984994118));
#69895=CARTESIAN_POINT('Ctrl Pts',(-0.522780345462078,-0.637585813690765,
-2.81652773651294));
#69896=CARTESIAN_POINT('Ctrl Pts',(-0.154975233012397,-0.80981346867949,
-2.80068562308471));
#69897=CARTESIAN_POINT('Ctrl Pts',(0.250431369065524,-0.785556602744988,
-2.78484350965647));
#69898=CARTESIAN_POINT('Ctrl Pts',(0.595076043601661,-0.570700980513612,
-2.76900139622823));
#69899=CARTESIAN_POINT('Ctrl Pts',(0.795337965757144,-0.217376647859616,
-2.7531592828));
#69900=CARTESIAN_POINT('Ctrl Pts',(0.802627773586437,0.188689549785515,
-2.73731716937176));
#69901=CARTESIAN_POINT('Ctrl Pts',(0.61517674617951,0.548974191752079,-2.72147505594353));
#69902=CARTESIAN_POINT('Ctrl Pts',(0.27846595382714,0.776061725259662,-2.7056329425153));
#69903=CARTESIAN_POINT('Ctrl Pts',(-0.125808775608511,0.814854123794499,
-2.68979082908706));
#69904=CARTESIAN_POINT('Ctrl Pts',(-0.499558638053648,0.65593921754596,
-2.67394871565883));
#69905=CARTESIAN_POINT('Ctrl Pts',(-0.752101050007928,0.33787438637163,
-2.65810660223059));
#69906=CARTESIAN_POINT('Ctrl Pts',(-0.822161879471254,-0.0621685953424848,
-2.64226448880235));
#69907=CARTESIAN_POINT('Ctrl Pts',(-0.692742332187273,-0.447127667972609,
-2.62642237537412));
#69908=CARTESIAN_POINT('Ctrl Pts',(-0.395243353255664,-0.723600568013129,
-2.61058026194588));
#69909=CARTESIAN_POINT('Ctrl Pts',(-0.00184684491450912,-0.824506931109911,
-2.59473814851765));
#69910=CARTESIAN_POINT('Ctrl Pts',(0.391997761702142,-0.725363939774458,
-2.57889603508941));
#69911=CARTESIAN_POINT('Ctrl Pts',(0.6907323137844,-0.450226566286644,-2.56305392166118));
#69912=CARTESIAN_POINT('Ctrl Pts',(0.821875123130991,-0.0658511372484234,
-2.54721180823294));
#69913=CARTESIAN_POINT('Ctrl Pts',(0.753607131146545,0.334501692348047,
-2.53136969480471));
#69914=CARTESIAN_POINT('Ctrl Pts',(0.502492137615154,0.653694685562662,
-2.51552758137647));
#69915=CARTESIAN_POINT('Ctrl Pts',(0.129457941270315,0.814282341537978,
-2.49968546794824));
#69916=CARTESIAN_POINT('Ctrl Pts',(-0.274986515685645,0.777301425760453,
-2.48384335452));
#69917=CARTESIAN_POINT('Ctrl Pts',(-0.612711248556089,0.551724583638581,
-2.46800124109177));
#69918=CARTESIAN_POINT('Ctrl Pts',(-0.801774417619176,0.192283315838124,
-2.45215912766353));
#69919=CARTESIAN_POINT('Ctrl Pts',(-0.796303800947335,-0.21381147512495,
-2.4363170142353));
#69920=CARTESIAN_POINT('Ctrl Pts',(-0.597626729206255,-0.568029385539622,
-2.42047490080706));
#69921=CARTESIAN_POINT('Ctrl Pts',(-0.253948036642577,-0.784426851263813,
-2.40463278737882));
#69922=CARTESIAN_POINT('Ctrl Pts',(0.151345833285741,-0.810499555240673,
-2.38879067395059));
#69923=CARTESIAN_POINT('Ctrl Pts',(0.519918803597792,-0.639921501407573,
-2.37294856052235));
#69924=CARTESIAN_POINT('Ctrl Pts',(0.762344355239403,-0.314079885272683,
-2.35710644709412));
#69925=CARTESIAN_POINT('Ctrl Pts',(0.819803000729591,0.0879666430702042,
-2.34126433366588));
#69926=CARTESIAN_POINT('Ctrl Pts',(0.678353602031553,0.468669906127011,
-2.32542222023765));
#69927=CARTESIAN_POINT('Ctrl Pts',(0.37231589598644,0.735660223128922,-2.30958010680941));
#69928=CARTESIAN_POINT('Ctrl Pts',(-0.0240564717090212,0.824157980284845,
-2.29373799338118));
#69929=CARTESIAN_POINT('Ctrl Pts',(-0.41459203991308,0.712691048589075,
-2.27789587995294));
#69930=CARTESIAN_POINT('Ctrl Pts',(-0.704535524748661,0.428304546631728,
-2.2620537665247));
#69931=CARTESIAN_POINT('Ctrl Pts',(-0.823538206532577,0.0399989084774863,
-2.24621165309647));
#69932=CARTESIAN_POINT('Ctrl Pts',(-0.74272657459735,-0.358011627863076,
-2.23036953966823));
#69933=CARTESIAN_POINT('Ctrl Pts',(-0.481707880491941,-0.669158133904268,
-2.21452742624));
#69934=CARTESIAN_POINT('Ctrl Pts',(-0.103812848664622,-0.81794742052923,
-2.19868531281176));
#69935=CARTESIAN_POINT('Ctrl Pts',(0.2992701986629,-0.768278880674557,-2.18284319938353));
#69936=CARTESIAN_POINT('Ctrl Pts',(0.629741594353524,-0.532203546248392,
-2.1670010859553));
#69937=CARTESIAN_POINT('Ctrl Pts',(0.80741936917992,-0.167000157399278,
-2.15115897252706));
#69938=CARTESIAN_POINT('Ctrl Pts',(0.789193728892756,0.238722325253902,
-2.13531685909882));
#69939=CARTESIAN_POINT('Ctrl Pts',(0.57948674374595,0.58652383082105,-2.11947474567059));
#69940=CARTESIAN_POINT('Ctrl Pts',(0.229179425679003,0.792017601536559,
-2.10363263224235));
#69941=CARTESIAN_POINT('Ctrl Pts',(-0.17673348457219,0.805344873783433,
-2.08779051881412));
#69942=CARTESIAN_POINT('Ctrl Pts',(-0.539765712845471,0.623272063817001,
-2.07194840538588));
#69943=CARTESIAN_POINT('Ctrl Pts',(-0.771835085205309,0.289975329199564,
-2.05610629195765));
#69944=CARTESIAN_POINT('Ctrl Pts',(-0.816634824375942,-0.113677851469657,
-2.04026417852941));
#69945=CARTESIAN_POINT('Ctrl Pts',(-0.663295211058166,-0.489749480127937,
-2.02442206510118));
#69946=CARTESIAN_POINT('Ctrl Pts',(-0.349020893874242,-0.746993645178798,
-2.00857995167294));
#69947=CARTESIAN_POINT('Ctrl Pts',(0.0499360401329562,-0.822995432669054,
-1.99273783824471));
#69948=CARTESIAN_POINT('Ctrl Pts',(0.43677703888679,-0.699314599160899,
-1.97689572481647));
#69949=CARTESIAN_POINT('Ctrl Pts',(0.717643228480402,-0.405959710949878,
-1.96105361138824));
#69950=CARTESIAN_POINT('Ctrl Pts',(0.824388304983522,-0.01410719336644,
-1.94521149796));
#69951=CARTESIAN_POINT('Ctrl Pts',(0.731112809166235,0.3811681395019,-1.92936938453177));
#69952=CARTESIAN_POINT('Ctrl Pts',(0.4604480883488,0.683960999059316,-1.91352727110353));
#69953=CARTESIAN_POINT('Ctrl Pts',(0.0780652735232223,0.820805033712652,
-1.8976851576753));
#69954=CARTESIAN_POINT('Ctrl Pts',(-0.32325844644872,0.758497901841424,
-1.88184304424706));
#69955=CARTESIAN_POINT('Ctrl Pts',(-0.646150268399774,0.512157125250817,
-1.86600093081883));
#69956=CARTESIAN_POINT('Ctrl Pts',(-0.812267248071997,0.141552138831698,
-1.85015881739059));
#69957=CARTESIAN_POINT('Ctrl Pts',(-0.781304576256766,-0.263397512172226,
-1.83431670396235));
#69958=CARTESIAN_POINT('Ctrl Pts',(-0.560774697392722,-0.604439268299457,
-1.81847459053412));
#69959=CARTESIAN_POINT('Ctrl Pts',(-0.204184572116599,-0.798826483541854,
-1.80263247710588));
#69960=CARTESIAN_POINT('Ctrl Pts',(0.201946667130782,-0.799395167569239,
-1.78679036367765));
#69961=CARTESIAN_POINT('Ctrl Pts',(0.55907977322475,-0.606007341101776,
-1.77094825024941));
#69962=CARTESIAN_POINT('Ctrl Pts',(0.780563870790618,-0.26558451369508,
-1.75510613682118));
#69963=CARTESIAN_POINT('Ctrl Pts',(0.812660477990166,0.139276838745992,
-1.73926402339294));
#69964=CARTESIAN_POINT('Ctrl Pts',(0.647582024690746,0.510345580558623,
-1.72342190996471));
#69965=CARTESIAN_POINT('Ctrl Pts',(0.325381343407219,0.757589645956699,
-1.70757979653647));
#69966=CARTESIAN_POINT('Ctrl Pts',(-0.07576631242369,0.821020435921054,
-1.69173768310823));
#69967=CARTESIAN_POINT('Ctrl Pts',(-0.458530857914507,0.685247796522155,
-1.67589556968));
#69968=CARTESIAN_POINT('Ctrl Pts',(-0.730042485245041,0.383214117740366,
-1.66005345625176));
#69969=CARTESIAN_POINT('Ctrl Pts',(-0.824424579278952,-0.0117984481609103,
-1.64421134282353));
#69970=CARTESIAN_POINT('Ctrl Pts',(-0.71877729979369,-0.403948367492151,
-1.6283692293953));
#69971=CARTESIAN_POINT('Ctrl Pts',(-0.438733748543603,-0.698088667854708,
-1.61252711596706));
#69972=CARTESIAN_POINT('Ctrl Pts',(-0.0522406334781668,-0.822852360093889,
-1.59668500253882));
#69973=CARTESIAN_POINT('Ctrl Pts',(0.346927578193464,-0.747968144901305,
-1.58084288911059));
#69974=CARTESIAN_POINT('Ctrl Pts',(0.661921072290253,-0.491605110181337,
-1.56500077568235));
#69975=CARTESIAN_POINT('Ctrl Pts',(0.816313268539809,-0.115964382049556,
-1.54915866225412));
#69976=CARTESIAN_POINT('Ctrl Pts',(0.772644131096213,0.28781267689395,-1.53331654882588));
#69977=CARTESIAN_POINT('Ctrl Pts',(0.541509062406833,0.621758012115288,
-1.51747443539765));
#69978=CARTESIAN_POINT('Ctrl Pts',(0.178988150511605,0.80484677565032,-1.50163232196941));
#69979=CARTESIAN_POINT('Ctrl Pts',(-0.226960490874059,0.792656310061612,
-1.48579020854118));
#69980=CARTESIAN_POINT('Ctrl Pts',(-0.577841918175875,0.588144376745292,
-1.46994809511294));
#69981=CARTESIAN_POINT('Ctrl Pts',(-0.788522095065032,0.240931517017877,
-1.45410598168471));
#69982=CARTESIAN_POINT('Ctrl Pts',(-0.807883884989266,-0.164738333950945,
-1.43826386825647));
#69983=CARTESIAN_POINT('Ctrl Pts',(-0.631229554758549,-0.530437875247995,
-1.42242175482823));
#69984=CARTESIAN_POINT('Ctrl Pts',(-0.301420581206097,-0.767437765244623,
-1.4065796414));
#69985=CARTESIAN_POINT('Ctrl Pts',(0.101521789311754,-0.818234939728941,
-1.39073752797176));
#69986=CARTESIAN_POINT('Ctrl Pts',(0.479832021942188,-0.670504527216002,
-1.37489541454353));
#69987=CARTESIAN_POINT('Ctrl Pts',(0.741721054676472,-0.360090221122297,
-1.35905330111529));
#69988=CARTESIAN_POINT('Ctrl Pts',(0.823646993609409,0.0376924424316771,
-1.34321118768706));
#69989=CARTESIAN_POINT('Ctrl Pts',(0.705732223915323,0.426329823523777,
-1.32736907425882));
#69990=CARTESIAN_POINT('Ctrl Pts',(0.416586297157071,0.711527193661101,
-1.31152696083059));
#69991=CARTESIAN_POINT('Ctrl Pts',(0.0263644222388554,0.824087378582086,
-1.29568484740235));
#69992=CARTESIAN_POINT('Ctrl Pts',(-0.370254228074203,0.736700004677249,
-1.27984273397412));
#69993=CARTESIAN_POINT('Ctrl Pts',(-0.677038437316519,0.470567789690592,
-1.26400062054588));
#69994=CARTESIAN_POINT('Ctrl Pts',(-0.819553436410745,0.090262146914535,
-1.24815850711765));
#69995=CARTESIAN_POINT('Ctrl Pts',(-0.763220942876712,-0.311943717123242,
-1.23231639368941));
#69996=CARTESIAN_POINT('Ctrl Pts',(-0.521708857543189,-0.63846296545631,
-1.21647428026118));
#69997=CARTESIAN_POINT('Ctrl Pts',(-0.153615034405297,-0.810072534717071,
-1.20063216683294));
#69998=CARTESIAN_POINT('Ctrl Pts',(0.251750262518701,-0.785134953762758,
-1.18479005340471));
#69999=CARTESIAN_POINT('Ctrl Pts',(0.596033625981975,-0.569700804806402,
-1.16894793997647));
#70000=CARTESIAN_POINT('Ctrl Pts',(0.79570190178519,-0.216040676248052,
-1.15310582654824));
#70001=CARTESIAN_POINT('Ctrl Pts',(0.802309760756444,0.190037201866422,
-1.13726371312));
#70002=CARTESIAN_POINT('Ctrl Pts',(0.614253944182277,0.550006529374697,
-1.12142159969176));
#70003=CARTESIAN_POINT('Ctrl Pts',(0.277162260987144,0.776528281122316,
-1.10557948626353));
#70004=CARTESIAN_POINT('Ctrl Pts',(-0.127177045364621,0.814641693894075,
-1.08973737283529));
#70005=CARTESIAN_POINT('Ctrl Pts',(-0.500659502770236,0.655099345583663,
-1.07389525940706));
#70006=CARTESIAN_POINT('Ctrl Pts',(-0.752667407860654,0.336610848670395,
-1.05805314597882));
#70007=CARTESIAN_POINT('Ctrl Pts',(-0.822056315596167,-0.0635492272709786,
-1.04221103255059));
#70008=CARTESIAN_POINT('Ctrl Pts',(-0.691990459440485,-0.448290412948603,
-1.02636891912235));
#70009=CARTESIAN_POINT('Ctrl Pts',(-0.394027597831391,-0.724263310161095,
-1.01052680569412));
#70010=CARTESIAN_POINT('Ctrl Pts',(-0.000462184425002042,-0.824508869984938,
-0.994684692265883));
#70011=CARTESIAN_POINT('Ctrl Pts',(0.393215368361151,-0.724704604913538,
-0.978842578837647));
#70012=CARTESIAN_POINT('Ctrl Pts',(0.691487439835499,-0.449065931515664,
-0.963000465409414));
#70013=CARTESIAN_POINT('Ctrl Pts',(0.821984553038164,-0.0644708062996728,
-0.947158351981175));
#70014=CARTESIAN_POINT('Ctrl Pts',(0.753044314032747,0.335766811047835,
-0.931316238552943));
#70015=CARTESIAN_POINT('Ctrl Pts',(0.50139362927632,0.654537637435314,-0.915474125124704));
#70016=CARTESIAN_POINT('Ctrl Pts',(0.128090271769204,0.814498601948693,
-0.899632011696473));
#70017=CARTESIAN_POINT('Ctrl Pts',(-0.276291509962364,0.776838523646324,
-0.883789898268234));
#70018=CARTESIAN_POINT('Ctrl Pts',(-0.613636938053462,0.550694832511305,
-0.867947784840001));
#70019=CARTESIAN_POINT('Ctrl Pts',(-0.802096203150231,0.190936563261905,
-0.852105671411765));
#70020=CARTESIAN_POINT('Ctrl Pts',(-0.795943607986144,-0.21514846781765,
-0.83626355798353));
#70021=CARTESIAN_POINT('Ctrl Pts',(-0.59667195103801,-0.569032225047738,
-0.820421444555294));
#70022=CARTESIAN_POINT('Ctrl Pts',(-0.252630330211578,-0.784852219564593,
-0.804579331127059));
#70023=CARTESIAN_POINT('Ctrl Pts',(0.152706754086307,-0.810244245616536,
-0.788737217698825));
#70024=CARTESIAN_POINT('Ctrl Pts',(0.520992739812211,-0.639047459396599,
-0.772895104270588));
#70025=CARTESIAN_POINT('Ctrl Pts',(0.762870738716788,-0.312799178879975,
-0.757052990842355));
#70026=CARTESIAN_POINT('Ctrl Pts',(0.819654115533445,0.0893432772365556,
-0.741210877414117));
#70027=CARTESIAN_POINT('Ctrl Pts',(0.677565572039378,0.469808456591869,
-0.725368763985883));
#70028=CARTESIAN_POINT('Ctrl Pts',(0.371079920186729,0.736284444445551,
-0.709526650557647));
#70029=CARTESIAN_POINT('Ctrl Pts',(-0.0254405096505967,0.824116418212256,
-0.693684537129412));
#70030=CARTESIAN_POINT('Ctrl Pts',(-0.415788332150249,0.711993787294522,
-0.677842423701178));
#70031=CARTESIAN_POINT('Ctrl Pts',(-0.70525381600185,0.427120761978518,
-0.662000310272941));
#70032=CARTESIAN_POINT('Ctrl Pts',(-0.823604218459063,0.0386158210416587,
-0.646158196844706));
#70033=CARTESIAN_POINT('Ctrl Pts',(-0.742124290784431,-0.359258440855583,
-0.630316083416471));
#70034=CARTESIAN_POINT('Ctrl Pts',(-0.480583432504365,-0.669966159369718,
-0.614473969988236));
#70035=CARTESIAN_POINT('Ctrl Pts',(-0.102439060278077,-0.818120607995927,
-0.598631856560001));
#70036=CARTESIAN_POINT('Ctrl Pts',(0.30056000644216,-0.767775209827565,
-0.582789743131765));
#70037=CARTESIAN_POINT('Ctrl Pts',(0.630634476656484,-0.53114522227968,
-0.566947629703531));
#70038=CARTESIAN_POINT('Ctrl Pts',(0.807698686798682,-0.165643960475012,
-0.551105516275293));
#70039=CARTESIAN_POINT('Ctrl Pts',(0.788791711252022,0.240047342327775,
-0.53526340284706));
#70040=CARTESIAN_POINT('Ctrl Pts',(0.578500932013622,0.587496180376762,
-0.519421289418824));
#70041=CARTESIAN_POINT('Ctrl Pts',(0.227849006445562,0.792401363300445,
-0.503579175990589));
#70042=CARTESIAN_POINT('Ctrl Pts',(-0.178085712920448,0.805046935993242,
-0.487737062562353));
#70043=CARTESIAN_POINT('Ctrl Pts',(-0.540811660389811,0.62236471484382,
-0.471894949134118));
#70044=CARTESIAN_POINT('Ctrl Pts',(-0.772320974669179,0.28867871828499,
-0.456052835705883));
#70045=CARTESIAN_POINT('Ctrl Pts',(-0.816442764829873,-0.115049128816222,
-0.440210722277647));
#70046=CARTESIAN_POINT('Ctrl Pts',(-0.662471801767662,-0.490862712155255,
-0.424368608849413));
#70047=CARTESIAN_POINT('Ctrl Pts',(-0.347765917804802,-0.747578729422039,
-0.408526495421177));
#70048=CARTESIAN_POINT('Ctrl Pts',(0.0513180891615079,-0.822910410693275,
-0.392684381992942));
#70049=CARTESIAN_POINT('Ctrl Pts',(0.437950835863752,-0.698580099741808,
-0.376842268564706));
#70050=CARTESIAN_POINT('Ctrl Pts',(0.71832397560555,-0.40475394505682,-0.361000155136471));
#70051=CARTESIAN_POINT('Ctrl Pts',(0.824410834241176,-0.0127227147567732,
-0.345158041708236));
#70052=CARTESIAN_POINT('Ctrl Pts',(0.730471652282162,0.38239541585384,-0.32931592828));
#70053=CARTESIAN_POINT('Ctrl Pts',(0.459298812591734,0.684733300637323,
-0.313473814851765));
#70054=CARTESIAN_POINT('Ctrl Pts',(0.0766867188231743,0.820934976893245,
-0.29763170142353));
#70055=CARTESIAN_POINT('Ctrl Pts',(-0.324531787362575,0.757953960211733,
-0.281789587995295));
#70056=CARTESIAN_POINT('Ctrl Pts',(-0.647009475978688,0.511071271763133,
-0.265947474567059));
#70057=CARTESIAN_POINT('Ctrl Pts',(-0.812503794740706,0.140187839202379,
-0.250105361138824));
#70058=CARTESIAN_POINT('Ctrl Pts',(-0.780861184376679,-0.264709251133773,
-0.234263247710588));
#70059=CARTESIAN_POINT('Ctrl Pts',(-0.559758720137868,-0.605380157133335,
-0.218421134282353));
#70060=CARTESIAN_POINT('Ctrl Pts',(-0.202842959779694,-0.799168281276578,
-0.202579020854118));
#70061=CARTESIAN_POINT('Ctrl Pts',(0.203289273038814,-0.799054853830805,
-0.186736907425883));
#70062=CARTESIAN_POINT('Ctrl Pts',(0.560095904927298,-0.605067663119104,
-0.170894793997648));
#70063=CARTESIAN_POINT('Ctrl Pts',(0.781010346026423,-0.264273116881618,
-0.155052680569412));
#70064=CARTESIAN_POINT('Ctrl Pts',(0.812422373100201,0.140641088911458,
-0.139210567141177));
#70065=CARTESIAN_POINT('Ctrl Pts',(0.646730057822694,0.51143301626051,-0.123368453712942));
#70066=CARTESIAN_POINT('Ctrl Pts',(0.32409678542623,0.758133800545566,-0.107526340284707));
#70067=CARTESIAN_POINT('Ctrl Pts',(-0.0771214967823103,0.820894379703354,
-0.0916842268564712));
#70068=CARTESIAN_POINT('Ctrl Pts',(-0.459730603216706,0.684472654204421,
-0.0758421134282357));
#70069=CARTESIAN_POINT('Ctrl Pts',(-0.640274482293033,0.4828170276367,-0.0652807044760789));
#70070=CARTESIAN_POINT('Ctrl Pts',(-0.701077753000059,0.366509473613423,
-0.0600000000000005));
#70071=CARTESIAN_POINT('Ctrl Pts',(0.437168237015825,-0.613060138694066,
-2.9529325805302));
#70072=CARTESIAN_POINT('Ctrl Pts',(0.538873825155734,-0.540534704637147,
-2.94765187605412));
#70073=CARTESIAN_POINT('Ctrl Pts',(0.705393947234175,-0.343965226545598,
-2.93709046710196));
#70074=CARTESIAN_POINT('Ctrl Pts',(0.784003077920512,0.0345814394106197,
-2.92124835367372));
#70075=CARTESIAN_POINT('Ctrl Pts',(0.672394775942478,0.404639543367737,
-2.90540624024549));
#70076=CARTESIAN_POINT('Ctrl Pts',(0.397642184080878,0.676568411154076,
-2.88956412681725));
#70077=CARTESIAN_POINT('Ctrl Pts',(0.02641088878806,0.784317782616846,-2.87372201338902));
#70078=CARTESIAN_POINT('Ctrl Pts',(-0.351228885865366,0.701781236716768,
-2.85787989996078));
#70079=CARTESIAN_POINT('Ctrl Pts',(-0.643650102008308,0.448965850545129,
-2.84203778653255));
#70080=CARTESIAN_POINT('Ctrl Pts',(-0.779903200303776,0.0872215090938687,
-2.82619567310431));
#70081=CARTESIAN_POINT('Ctrl Pts',(-0.726929049354935,-0.295686944193908,
-2.81035355967608));
#70082=CARTESIAN_POINT('Ctrl Pts',(-0.497580804097368,-0.606852313043473,
-2.79451144624784));
#70083=CARTESIAN_POINT('Ctrl Pts',(-0.147504973602872,-0.770778091433911,
-2.77866933281961));
#70084=CARTESIAN_POINT('Ctrl Pts',(0.238359844765566,-0.747690477369339,
-2.76282721939137));
#70085=CARTESIAN_POINT('Ctrl Pts',(0.566391638179665,-0.543191524409974,
-2.74698510596314));
#70086=CARTESIAN_POINT('Ctrl Pts',(0.757000350081665,-0.20689845778034,
-2.7311429925349));
#70087=CARTESIAN_POINT('Ctrl Pts',(0.763938767856739,0.179594161720182,
-2.71530087910667));
#70088=CARTESIAN_POINT('Ctrl Pts',(0.585523428114815,0.522512030400192,
-2.69945876567843));
#70089=CARTESIAN_POINT('Ctrl Pts',(0.265043080562979,0.738653280743715,
-2.6836166522502));
#70090=CARTESIAN_POINT('Ctrl Pts',(-0.119744424734367,0.775575772232499,
-2.66777453882196));
#70091=CARTESIAN_POINT('Ctrl Pts',(-0.475478450890907,0.624321029163851,
-2.65193242539373));
#70092=CARTESIAN_POINT('Ctrl Pts',(-0.715847580104881,0.321587852936783,
-2.63609031196549));
#70093=CARTESIAN_POINT('Ctrl Pts',(-0.782531272716308,-0.059171887253674,
-2.62024819853726));
#70094=CARTESIAN_POINT('Ctrl Pts',(-0.659350126059844,-0.425574806886333,
-2.60440608510902));
#70095=CARTESIAN_POINT('Ctrl Pts',(-0.376191467858767,-0.688720904683293,
-2.58856397168079));
#70096=CARTESIAN_POINT('Ctrl Pts',(-0.00175782158908592,-0.784763286008587,
-2.57272185825255));
#70097=CARTESIAN_POINT('Ctrl Pts',(0.373102323308885,-0.690399276769274,
-2.55687974482431));
#70098=CARTESIAN_POINT('Ctrl Pts',(0.657436996421685,-0.428524329239833,
-2.54103763139608));
#70099=CARTESIAN_POINT('Ctrl Pts',(0.782258338870179,-0.0626769198712575,
-2.52519551796784));
#70100=CARTESIAN_POINT('Ctrl Pts',(0.717281063728533,0.318377732627569,
-2.50935340453961));
#70101=CARTESIAN_POINT('Ctrl Pts',(0.47827054719541,0.622184690185607,-2.49351129111137));
#70102=CARTESIAN_POINT('Ctrl Pts',(0.123217689940382,0.775031551552749,
-2.47766917768314));
#70103=CARTESIAN_POINT('Ctrl Pts',(-0.261731361514479,0.739833224055233,
-2.4618270642549));
#70104=CARTESIAN_POINT('Ctrl Pts',(-0.58317677468645,0.525129845355069,
-2.44598495082667));
#70105=CARTESIAN_POINT('Ctrl Pts',(-0.763126546142486,0.183014697740164,
-2.43014283739843));
#70106=CARTESIAN_POINT('Ctrl Pts',(-0.757919629191393,-0.203505136796763,
-2.41430072397019));
#70107=CARTESIAN_POINT('Ctrl Pts',(-0.568819373279402,-0.540648708126009,
-2.39845861054196));
#70108=CARTESIAN_POINT('Ctrl Pts',(-0.241706998681967,-0.746615183213176,
-2.38261649711372));
#70109=CARTESIAN_POINT('Ctrl Pts',(0.144050521556132,-0.771431106616591,
-2.36677438368549));
#70110=CARTESIAN_POINT('Ctrl Pts',(0.494857196918661,-0.609075413782312,
-2.35093227025725));
#70111=CARTESIAN_POINT('Ctrl Pts',(0.725597128070741,-0.298940316370648,
-2.33509015682902));
#70112=CARTESIAN_POINT('Ctrl Pts',(0.780286098827823,0.083726393642309,
-2.31924804340078));
#70113=CARTESIAN_POINT('Ctrl Pts',(0.645654974773131,0.446078646167914,
-2.30340592997255));
#70114=CARTESIAN_POINT('Ctrl Pts',(0.354369181074354,0.700199249157682,
-2.28756381654431));
#70115=CARTESIAN_POINT('Ctrl Pts',(-0.0228968794267542,0.784431155633691,
-2.27172170311608));
#70116=CARTESIAN_POINT('Ctrl Pts',(-0.394607491239903,0.678337255997074,
-2.25587958968784));
#70117=CARTESIAN_POINT('Ctrl Pts',(-0.670574852254142,0.407659015036618,
-2.24003747625961));
#70118=CARTESIAN_POINT('Ctrl Pts',(-0.783841256788622,0.0380708441241249,
-2.22419536283137));
#70119=CARTESIAN_POINT('Ctrl Pts',(-0.706924981821915,-0.340754420503058,
-2.20835324940314));
#70120=CARTESIAN_POINT('Ctrl Pts',(-0.458488152042827,-0.636902755098958,
-2.1925111359749));
#70121=CARTESIAN_POINT('Ctrl Pts',(-0.0988087657896205,-0.778519963019204,
-2.17666902254667));
#70122=CARTESIAN_POINT('Ctrl Pts',(0.284844499961923,-0.73124559202619,
-2.16082690911843));
#70123=CARTESIAN_POINT('Ctrl Pts',(0.599386208016341,-0.506549779050472,
-2.1449847956902));
#70124=CARTESIAN_POINT('Ctrl Pts',(0.768499394531042,-0.158950261471042,
-2.12914268226196));
#70125=CARTESIAN_POINT('Ctrl Pts',(0.751152283401107,0.227215211105232,
-2.11330056883372));
#70126=CARTESIAN_POINT('Ctrl Pts',(0.551553788163199,0.558251667063445,
-2.09745845540549));
#70127=CARTESIAN_POINT('Ctrl Pts',(0.218132307195168,0.753840037125916,
-2.08161634197725));
#70128=CARTESIAN_POINT('Ctrl Pts',(-0.168214413812045,0.7665248958789,-2.06577422854902));
#70129=CARTESIAN_POINT('Ctrl Pts',(-0.513747427104302,0.593228527769866,
-2.04993211512079));
#70130=CARTESIAN_POINT('Ctrl Pts',(-0.734630377099514,0.275997670386755,
-2.03409000169254));
#70131=CARTESIAN_POINT('Ctrl Pts',(-0.777270637838795,-0.108198246612234,
-2.01824788826432));
#70132=CARTESIAN_POINT('Ctrl Pts',(-0.631322442278385,-0.46614212306114,
-2.00240577483608));
#70133=CARTESIAN_POINT('Ctrl Pts',(-0.33219706618317,-0.710986367123579,
-1.98656366140784));
#70134=CARTESIAN_POINT('Ctrl Pts',(0.0475289769756635,-0.7833246462125,
-1.97072154797961));
#70135=CARTESIAN_POINT('Ctrl Pts',(0.415723108389742,-0.665605590546729,
-1.95487943455137));
#70136=CARTESIAN_POINT('Ctrl Pts',(0.683050726336488,-0.386391265775365,
-1.93903732112314));
#70137=CARTESIAN_POINT('Ctrl Pts',(0.784650378008375,-0.0134271853939425,
-1.9231952076949));
#70138=CARTESIAN_POINT('Ctrl Pts',(0.695871033845534,0.362794720566657,
-1.90735309426667));
#70139=CARTESIAN_POINT('Ctrl Pts',(0.438253144048835,0.650992078867018,
-1.89151098083843));
#70140=CARTESIAN_POINT('Ctrl Pts',(0.0743022990610538,0.781239830890958,
-1.8756688674102));
#70141=CARTESIAN_POINT('Ctrl Pts',(-0.30767644405807,0.721936084974336,
-1.85982675398196));
#70142=CARTESIAN_POINT('Ctrl Pts',(-0.615003935991344,0.487469654164693,
-1.84398464055373));
#70143=CARTESIAN_POINT('Ctrl Pts',(-0.773113591484361,0.134728911813473,
-1.82814252712549));
#70144=CARTESIAN_POINT('Ctrl Pts',(-0.743643410991619,-0.250700981858951,
-1.81230041369726));
#70145=CARTESIAN_POINT('Ctrl Pts',(-0.533743717161932,-0.5753035280671,
-1.79645830026902));
#70146=CARTESIAN_POINT('Ctrl Pts',(-0.194342278664382,-0.760320711108034,
-1.78061618684078));
#70147=CARTESIAN_POINT('Ctrl Pts',(0.192212247242966,-0.760861982902353,
-1.76477407341255));
#70148=CARTESIAN_POINT('Ctrl Pts',(0.532130493295156,-0.576796015174987,
-1.74893195998431));
#70149=CARTESIAN_POINT('Ctrl Pts',(0.742938409694909,-0.252782563513171,
-1.73308984655608));
#70150=CARTESIAN_POINT('Ctrl Pts',(0.773487866570592,0.132563287845333,
-1.71724773312784));
#70151=CARTESIAN_POINT('Ctrl Pts',(0.616366677442347,0.485745431223982,
-1.70140561969961));
#70152=CARTESIAN_POINT('Ctrl Pts',(0.309697011175393,0.721071609679177,
-1.68556350627137));
#70153=CARTESIAN_POINT('Ctrl Pts',(-0.0721141546091439,0.781444850083036,
-1.66972139284314));
#70154=CARTESIAN_POINT('Ctrl Pts',(-0.436428329727842,0.652216848929293,
-1.6538792794149));
#70155=CARTESIAN_POINT('Ctrl Pts',(-0.694852302667184,0.364742076671178,
-1.63803716598667));
#70156=CARTESIAN_POINT('Ctrl Pts',(-0.784684903776692,-0.0112297284585551,
-1.62219505255843));
#70157=CARTESIAN_POINT('Ctrl Pts',(-0.684130132096222,-0.384476874953873,
-1.6063529391302));
#70158=CARTESIAN_POINT('Ctrl Pts',(-0.417585498919284,-0.664438752714366,
-1.59051082570196));
#70159=CARTESIAN_POINT('Ctrl Pts',(-0.0497224821825411,-0.783188470153831,
-1.57466871227372));
#70160=CARTESIAN_POINT('Ctrl Pts',(0.330204654439483,-0.711913893109829,
-1.55882659884549));
#70161=CARTESIAN_POINT('Ctrl Pts',(0.630014541017341,-0.46790830631973,
-1.54298448541725));
#70162=CARTESIAN_POINT('Ctrl Pts',(0.776964581934259,-0.110374559731907,
-1.52714237198902));
#70163=CARTESIAN_POINT('Ctrl Pts',(0.735400424612663,0.273939264246303,
-1.51130025856078));
#70164=CARTESIAN_POINT('Ctrl Pts',(0.515406742118902,0.591787457787566,
-1.49545814513255));
#70165=CARTESIAN_POINT('Ctrl Pts',(0.170360398260084,0.766050807532343,
-1.47961603170431));
#70166=CARTESIAN_POINT('Ctrl Pts',(-0.216020331536435,0.754447958032348,
-1.46377391827608));
#70167=CARTESIAN_POINT('Ctrl Pts',(-0.549988247995402,0.559794097935337,
-1.44793180484784));
#70168=CARTESIAN_POINT('Ctrl Pts',(-0.750513024287871,0.229317913366062,
-1.43208969141961));
#70169=CARTESIAN_POINT('Ctrl Pts',(-0.76894151932004,-0.156797464526944,
-1.41624757799137));
#70170=CARTESIAN_POINT('Ctrl Pts',(-0.600802444378748,-0.504869218555471,
-1.40040546456314));
#70171=CARTESIAN_POINT('Ctrl Pts',(-0.286891227778387,-0.730445020819569,
-1.3845633511349));
#70172=CARTESIAN_POINT('Ctrl Pts',(0.0966281421970794,-0.778793622952724,
-1.36872123770667));
#70173=CARTESIAN_POINT('Ctrl Pts',(0.456702715360558,-0.638184248315942,
-1.35287912427843));
#70174=CARTESIAN_POINT('Ctrl Pts',(0.705967930901566,-0.34273281948896,
-1.3370370108502));
#70175=CARTESIAN_POINT('Ctrl Pts',(0.783944800010236,0.0358755564862942,
-1.32119489742196));
#70176=CARTESIAN_POINT('Ctrl Pts',(0.671713867021582,0.405779479356957,
-1.30535278399373));
#70177=CARTESIAN_POINT('Ctrl Pts',(0.396505619453125,0.677229502279976,
-1.28951067056549));
#70178=CARTESIAN_POINT('Ctrl Pts',(0.0250935799921388,0.784363957139456,
-1.27366855713726));
#70179=CARTESIAN_POINT('Ctrl Pts',(-0.352406891584218,0.70118891019485,
-1.25782644370902));
#70180=CARTESIAN_POINT('Ctrl Pts',(-0.644403204843168,0.447885046193937,
-1.24198433028078));
#70181=CARTESIAN_POINT('Ctrl Pts',(-0.780048564238921,0.0859112474888284,
-1.22614221685255));
#70182=CARTESIAN_POINT('Ctrl Pts',(-0.726431461620614,-0.296907117772595,
-1.21030010342431));
#70183=CARTESIAN_POINT('Ctrl Pts',(-0.496560965029412,-0.607687183528952,
-1.19445798999608));
#70184=CARTESIAN_POINT('Ctrl Pts',(-0.146210340546125,-0.77102466973092,
-1.17861587656784));
#70185=CARTESIAN_POINT('Ctrl Pts',(0.239615163697594,-0.747289153101038,
-1.16277376313961));
#70186=CARTESIAN_POINT('Ctrl Pts',(0.567303062289086,-0.542239560096563,
-1.14693164971137));
#70187=CARTESIAN_POINT('Ctrl Pts',(0.757346743328938,-0.205626883907099,
-1.13108953628314));
#70188=CARTESIAN_POINT('Ctrl Pts',(0.763636084175085,0.180876853029987,
-1.1152474228549));
#70189=CARTESIAN_POINT('Ctrl Pts',(0.584645107872305,0.52349460633064,-1.09940530942667));
#70190=CARTESIAN_POINT('Ctrl Pts',(0.263802229530127,0.739097347249484,
-1.08356319599843));
#70191=CARTESIAN_POINT('Ctrl Pts',(-0.12104673988714,0.775373582074464,
-1.0677210825702));
#70192=CARTESIAN_POINT('Ctrl Pts',(-0.47652625070901,0.623521641486088,
-1.05187896914196));
#70193=CARTESIAN_POINT('Ctrl Pts',(-0.716386637852962,0.320385221447583,
-1.03603685571372));
#70194=CARTESIAN_POINT('Ctrl Pts',(-0.78243079732869,-0.0604859686859734,
-1.02019474228549));
#70195=CARTESIAN_POINT('Ctrl Pts',(-0.658634495778076,-0.426681504154387,
-1.00435262885725));
#70196=CARTESIAN_POINT('Ctrl Pts',(-0.375034315401055,-0.689351700721738,
-0.988510515429021));
#70197=CARTESIAN_POINT('Ctrl Pts',(-0.000439905784195014,-0.784765131424169,
-0.972668402000785));
#70198=CARTESIAN_POINT('Ctrl Pts',(0.374261237766406,-0.689771723776676,
-0.956826288572549));
#70199=CARTESIAN_POINT('Ctrl Pts',(0.658155723188982,-0.42741964045874,
-0.940984175144316));
#70200=CARTESIAN_POINT('Ctrl Pts',(0.782362493935833,-0.0613631249105981,
-0.925142061716077));
#70201=CARTESIAN_POINT('Ctrl Pts',(0.716745376045408,0.31958186890657,-0.909299948287845));
#70202=CARTESIAN_POINT('Ctrl Pts',(0.477224990170764,0.622987009313038,
-0.893457834859608));
#70203=CARTESIAN_POINT('Ctrl Pts',(0.12191594610856,0.77523738757928,-0.877615721431374));
#70204=CARTESIAN_POINT('Ctrl Pts',(-0.262973451250997,0.739392635176622,
-0.861773608003137));
#70205=CARTESIAN_POINT('Ctrl Pts',(-0.584057843243151,0.524149731243324,
-0.845931494574904));
#70206=CARTESIAN_POINT('Ctrl Pts',(-0.763432820669978,0.181732862576291,
-0.830089381146666));
#70207=CARTESIAN_POINT('Ctrl Pts',(-0.757576798584207,-0.204777682532043,
-0.814247267718432));
#70208=CARTESIAN_POINT('Ctrl Pts',(-0.567910618210827,-0.541603207837332,
-0.798405154290196));
#70209=CARTESIAN_POINT('Ctrl Pts',(-0.240452809554177,-0.747020047517997,
-0.782563040861961));
#70210=CARTESIAN_POINT('Ctrl Pts',(0.145345841994508,-0.771188103662912,
-0.766720927433726));
#70211=CARTESIAN_POINT('Ctrl Pts',(0.495879366267142,-0.60824350315214,
-0.750878814005491));
#70212=CARTESIAN_POINT('Ctrl Pts',(0.726098138325266,-0.297721343771107,
-0.735036700577256));
#70213=CARTESIAN_POINT('Ctrl Pts',(0.780144390333501,0.0850366700162907,
-0.71919458714902));
#70214=CARTESIAN_POINT('Ctrl Pts',(0.644904930130934,0.447162315171019,
-0.703352473720785));
#70215=CARTESIAN_POINT('Ctrl Pts',(0.353192782922427,0.700793381181502,
-0.68751036029255));
#70216=CARTESIAN_POINT('Ctrl Pts',(-0.0242142026923446,0.784391596974536,
-0.671668246864314));
#70217=CARTESIAN_POINT('Ctrl Pts',(-0.395746118693045,0.67767360473585,
-0.655826133436079));
#70218=CARTESIAN_POINT('Ctrl Pts',(-0.671258519768501,0.406532292265314,
-0.639984020007844));
#70219=CARTESIAN_POINT('Ctrl Pts',(-0.78390408674722,0.0367544255471266,
-0.624141906579608));
#70220=CARTESIAN_POINT('Ctrl Pts',(-0.706351729849976,-0.341941133463399,
-0.608299793151373));
#70221=CARTESIAN_POINT('Ctrl Pts',(-0.457417905736359,-0.637671831374146,
-0.592457679723138));
#70222=CARTESIAN_POINT('Ctrl Pts',(-0.0975011980205375,-0.778684802343572,
-0.576615566294902));
#70223=CARTESIAN_POINT('Ctrl Pts',(0.28607213523457,-0.730766199586856,
-0.560773452866667));
#70224=CARTESIAN_POINT('Ctrl Pts',(0.600236050781331,-0.505542469391802,
-0.544931339438432));
#70225=CARTESIAN_POINT('Ctrl Pts',(0.7687652482238,-0.157659437204313,-0.529089226010197));
#70226=CARTESIAN_POINT('Ctrl Pts',(0.750769644186234,0.228476358481531,
-0.513247112581962));
#70227=CARTESIAN_POINT('Ctrl Pts',(0.550615495439079,0.55917714652723,-0.497404999153727));
#70228=CARTESIAN_POINT('Ctrl Pts',(0.216866018059188,0.754205300450586,
-0.481562885725491));
#70229=CARTESIAN_POINT('Ctrl Pts',(-0.169501460799733,0.766241319561427,
-0.465720772297256));
#70230=CARTESIAN_POINT('Ctrl Pts',(-0.514742956918447,0.592364915670458,
-0.44987865886902));
#70231=CARTESIAN_POINT('Ctrl Pts',(-0.735092845270387,0.274763559909812,
-0.434036545440785));
#70232=CARTESIAN_POINT('Ctrl Pts',(-0.777087836124468,-0.109503424380808,
-0.418194432012549));
#70233=CARTESIAN_POINT('Ctrl Pts',(-0.630538723723493,-0.467201694049429,
-0.402352318584315));
#70234=CARTESIAN_POINT('Ctrl Pts',(-0.331002583630077,-0.711543248595394,
-0.386510205156079));
#70235=CARTESIAN_POINT('Ctrl Pts',(0.0488444071996538,-0.783243722544574,
-0.370668091727844));
#70236=CARTESIAN_POINT('Ctrl Pts',(0.41684032492,-0.66490649614746,-0.354825978299608));
#70237=CARTESIAN_POINT('Ctrl Pts',(0.683698659459563,-0.385243621324251,
-0.338983864871373));
#70238=CARTESIAN_POINT('Ctrl Pts',(0.784671821289931,-0.0121094427017519,
-0.323141751443138));
#70239=CARTESIAN_POINT('Ctrl Pts',(0.695260782598142,0.363962838609635,
-0.307299638014903));
#70240=CARTESIAN_POINT('Ctrl Pts',(0.43715926674397,0.651727153250601,-0.291457524586667));
#70241=CARTESIAN_POINT('Ctrl Pts',(0.0729901947287151,0.781363510430267,
-0.275615411158432));
#70242=CARTESIAN_POINT('Ctrl Pts',(-0.308888406216377,0.721418362921788,
-0.259773297730197));
#70243=CARTESIAN_POINT('Ctrl Pts',(-0.61582172725246,0.486436141990367,
-0.243931184301961));
#70244=CARTESIAN_POINT('Ctrl Pts',(-0.77333873591193,0.133430375415769,
-0.228089070873726));
#70245=CARTESIAN_POINT('Ctrl Pts',(-0.743221391896717,-0.251949491166766,
-0.212246957445491));
#70246=CARTESIAN_POINT('Ctrl Pts',(-0.532776712981681,-0.57619906330784,
-0.196404844017256));
#70247=CARTESIAN_POINT('Ctrl Pts',(-0.193065335965257,-0.760646033192459,
-0.18056273058902));
#70248=CARTESIAN_POINT('Ctrl Pts',(0.193490135620185,-0.760538073281255,
-0.164720617160785));
#70249=CARTESIAN_POINT('Ctrl Pts',(0.53309764447827,-0.575901632418885,
-0.14887850373255));
#70250=CARTESIAN_POINT('Ctrl Pts',(0.743363363518767,-0.251534379860902,
-0.133036390304315));
#70251=CARTESIAN_POINT('Ctrl Pts',(0.773261239032588,0.133861777163485,
-0.117194276876079));
#70252=CARTESIAN_POINT('Ctrl Pts',(0.615555777868655,0.486780449345162,
-0.101352163447844));
#70253=CARTESIAN_POINT('Ctrl Pts',(0.308474372645389,0.721589534425644,
-0.0855100500196088));
#70254=CARTESIAN_POINT('Ctrl Pts',(-0.0734040151188502,0.781324870143642,
-0.0696679365913733));
#70255=CARTESIAN_POINT('Ctrl Pts',(-0.437570243798181,0.651479070737944,
-0.0538258231631379));
#70256=CARTESIAN_POINT('Ctrl Pts',(-0.609411379956911,0.459543835051841,
-0.0432644142109811));
#70257=CARTESIAN_POINT('Ctrl Pts',(-0.667283755215033,0.348842645238846,
-0.0379837097349027));
#70258=CARTESIAN_POINT('Ctrl Pts',(0.415028236876551,-0.582012248186914,
-2.9309162902651));
#70259=CARTESIAN_POINT('Ctrl Pts',(0.511583035126158,-0.513159800829765,
-2.92563558578902));
#70260=CARTESIAN_POINT('Ctrl Pts',(0.669669892356321,-0.326545410742852,
-2.91507417683687));
#70261=CARTESIAN_POINT('Ctrl Pts',(0.744297932887927,0.0328300928841836,
-2.89923206340863));
#70262=CARTESIAN_POINT('Ctrl Pts',(0.638341935016441,0.3841469302546,-2.88338994998039));
#70263=CARTESIAN_POINT('Ctrl Pts',(0.377503946062879,0.642304200150481,
-2.86754783655216));
#70264=CARTESIAN_POINT('Ctrl Pts',(0.0250733325981615,0.744596699642227,
-2.85170572312392));
#70265=CARTESIAN_POINT('Ctrl Pts',(-0.333441208436975,0.666240144379612,
-2.83586360969569));
#70266=CARTESIAN_POINT('Ctrl Pts',(-0.611053009764407,0.426228370664493,
-2.82002149626745));
#70267=CARTESIAN_POINT('Ctrl Pts',(-0.740405689960357,0.0828042526237523,
-2.80417938283922));
#70268=CARTESIAN_POINT('Ctrl Pts',(-0.690114368206497,-0.280712139458959,
-2.78833726941098));
#70269=CARTESIAN_POINT('Ctrl Pts',(-0.472381262732657,-0.576118812396181,
-2.77249515598275));
#70270=CARTESIAN_POINT('Ctrl Pts',(-0.140034714193347,-0.731742714188332,
-2.75665304255451));
#70271=CARTESIAN_POINT('Ctrl Pts',(0.226288320465609,-0.709824351993689,
-2.74081092912627));
#70272=CARTESIAN_POINT('Ctrl Pts',(0.537707232757668,-0.515682068306337,
-2.72496881569804));
#70273=CARTESIAN_POINT('Ctrl Pts',(0.718662734406186,-0.196420267701063,
-2.7091267022698));
#70274=CARTESIAN_POINT('Ctrl Pts',(0.725249762127042,0.170498773654849,
-2.69328458884157));
#70275=CARTESIAN_POINT('Ctrl Pts',(0.555870110050121,0.496049869048306,
-2.67744247541333));
#70276=CARTESIAN_POINT('Ctrl Pts',(0.251620207298818,0.701244836227764,
-2.6616003619851));
#70277=CARTESIAN_POINT('Ctrl Pts',(-0.113680073860222,0.736297420670501,
-2.64575824855686));
#70278=CARTESIAN_POINT('Ctrl Pts',(-0.451398263728168,0.59270284078174,
-2.62991613512863));
#70279=CARTESIAN_POINT('Ctrl Pts',(-0.679594110201831,0.305301319501937,
-2.61407402170039));
#70280=CARTESIAN_POINT('Ctrl Pts',(-0.742900665961364,-0.0561751791648646,
-2.59823190827216));
#70281=CARTESIAN_POINT('Ctrl Pts',(-0.625957919932414,-0.404021945800056,
-2.58238979484392));
#70282=CARTESIAN_POINT('Ctrl Pts',(-0.357139582461871,-0.653841241353458,
-2.56654768141569));
#70283=CARTESIAN_POINT('Ctrl Pts',(-0.00166879826366219,-0.745019640907262,
-2.55070556798745));
#70284=CARTESIAN_POINT('Ctrl Pts',(0.354206884915627,-0.655434613764092,
-2.53486345455922));
#70285=CARTESIAN_POINT('Ctrl Pts',(0.62414167905897,-0.40682209219302,-2.51902134113098));
#70286=CARTESIAN_POINT('Ctrl Pts',(0.742641554609368,-0.0595027024940923,
-2.50317922770275));
#70287=CARTESIAN_POINT('Ctrl Pts',(0.68095499631052,0.302253772907092,-2.48733711427451));
#70288=CARTESIAN_POINT('Ctrl Pts',(0.454048956775666,0.590674694808553,
-2.47149500084627));
#70289=CARTESIAN_POINT('Ctrl Pts',(0.116977438610447,0.73578076156752,-2.45565288741804));
#70290=CARTESIAN_POINT('Ctrl Pts',(-0.248476207343311,0.702365022350014,
-2.43981077398981));
#70291=CARTESIAN_POINT('Ctrl Pts',(-0.553642300816813,0.498535107071557,
-2.42396866056157));
#70292=CARTESIAN_POINT('Ctrl Pts',(-0.724478674665794,0.173746079642204,
-2.40812654713333));
#70293=CARTESIAN_POINT('Ctrl Pts',(-0.719535457435451,-0.193198798468575,
-2.3922844337051));
#70294=CARTESIAN_POINT('Ctrl Pts',(-0.540012017352549,-0.513268030712396,
-2.37644232027686));
#70295=CARTESIAN_POINT('Ctrl Pts',(-0.229465960721355,-0.708803515162537,
-2.36060020684863));
#70296=CARTESIAN_POINT('Ctrl Pts',(0.136755209826522,-0.73236265799251,
-2.34475809342039));
#70297=CARTESIAN_POINT('Ctrl Pts',(0.46979559023953,-0.578229326157051,
-2.32891597999216));
#70298=CARTESIAN_POINT('Ctrl Pts',(0.68884990090208,-0.283800747468612,
-2.31307386656392));
#70299=CARTESIAN_POINT('Ctrl Pts',(0.740769196926055,0.0794861442144139,
-2.29723175313569));
#70300=CARTESIAN_POINT('Ctrl Pts',(0.612956347514708,0.423487386208817,
-2.28138963970745));
#70301=CARTESIAN_POINT('Ctrl Pts',(0.336422466162267,0.664738275186441,
-2.26554752627922));
#70302=CARTESIAN_POINT('Ctrl Pts',(-0.0217372871444871,0.744704330982535,
-2.24970541285098));
#70303=CARTESIAN_POINT('Ctrl Pts',(-0.374622942566726,0.643983463405074,
-2.23386329942275));
#70304=CARTESIAN_POINT('Ctrl Pts',(-0.636614179759623,0.387013483441507,
-2.21802118599451));
#70305=CARTESIAN_POINT('Ctrl Pts',(-0.744144307044669,0.0361427797707638,
-2.20217907256628));
#70306=CARTESIAN_POINT('Ctrl Pts',(-0.67112338904648,-0.32349721314304,
-2.18633695913804));
#70307=CARTESIAN_POINT('Ctrl Pts',(-0.435268423593712,-0.604647376293648,
-2.17049484570981));
#70308=CARTESIAN_POINT('Ctrl Pts',(-0.0938046829146193,-0.739092505509178,
-2.15465273228157));
#70309=CARTESIAN_POINT('Ctrl Pts',(0.270418801260945,-0.694212303377822,
-2.13881061885333));
#70310=CARTESIAN_POINT('Ctrl Pts',(0.569030821679157,-0.480896011852553,
-2.1229685054251));
#70311=CARTESIAN_POINT('Ctrl Pts',(0.729579419882164,-0.150900365542804,
-2.10712639199686));
#70312=CARTESIAN_POINT('Ctrl Pts',(0.713110837909455,0.215708096956561,
-2.09128427856863));
#70313=CARTESIAN_POINT('Ctrl Pts',(0.523620832580449,0.529979503305841,
-2.07544216514039));
#70314=CARTESIAN_POINT('Ctrl Pts',(0.207085188711333,0.715662472715273,
-2.05960005171216));
#70315=CARTESIAN_POINT('Ctrl Pts',(-0.159695343051901,0.727704917974369,
-2.04375793828392));
#70316=CARTESIAN_POINT('Ctrl Pts',(-0.487729141363133,0.563184991722728,
-2.02791582485569));
#70317=CARTESIAN_POINT('Ctrl Pts',(-0.697425668993718,0.262020011573948,
-2.01207371142745));
#70318=CARTESIAN_POINT('Ctrl Pts',(-0.73790645130165,-0.102718641754811,
-1.99623159799922));
#70319=CARTESIAN_POINT('Ctrl Pts',(-0.599349673498601,-0.442534765994343,
-1.98038948457098));
#70320=CARTESIAN_POINT('Ctrl Pts',(-0.315373238492099,-0.674979089068359,
-1.96454737114274));
#70321=CARTESIAN_POINT('Ctrl Pts',(0.0451219138183706,-0.743653859755946,
-1.94870525771451));
#70322=CARTESIAN_POINT('Ctrl Pts',(0.394669177892695,-0.631896581932559,
-1.93286314428627));
#70323=CARTESIAN_POINT('Ctrl Pts',(0.648458224192572,-0.366822820600851,
-1.91702103085804));
#70324=CARTESIAN_POINT('Ctrl Pts',(0.744912451033229,-0.0127471774214454,
-1.90117891742981));
#70325=CARTESIAN_POINT('Ctrl Pts',(0.660629258524832,0.344421301631415,
-1.88533680400157));
#70326=CARTESIAN_POINT('Ctrl Pts',(0.416058199748869,0.618023158674719,
-1.86949469057334));
#70327=CARTESIAN_POINT('Ctrl Pts',(0.0705393245988857,0.741674628069264,
-1.8536525771451));
#70328=CARTESIAN_POINT('Ctrl Pts',(-0.292094441667422,0.685374268107247,
-1.83781046371687));
#70329=CARTESIAN_POINT('Ctrl Pts',(-0.583857603582913,0.462782183078569,
-1.82196835028863));
#70330=CARTESIAN_POINT('Ctrl Pts',(-0.733959934896726,0.127905684795247,
-1.80612623686039));
#70331=CARTESIAN_POINT('Ctrl Pts',(-0.705982245726471,-0.238004451545676,
-1.79028412343216));
#70332=CARTESIAN_POINT('Ctrl Pts',(-0.506712736931143,-0.546167787834743,
-1.77444201000392));
#70333=CARTESIAN_POINT('Ctrl Pts',(-0.184499985212165,-0.721814938674213,
-1.75859989657569));
#70334=CARTESIAN_POINT('Ctrl Pts',(0.182477827355149,-0.722328798235466,
-1.74275778314745));
#70335=CARTESIAN_POINT('Ctrl Pts',(0.505181213365562,-0.547584689248198,
-1.72691566971922));
#70336=CARTESIAN_POINT('Ctrl Pts',(0.7053129485992,-0.239980613331262,-1.71107355629098));
#70337=CARTESIAN_POINT('Ctrl Pts',(0.734315255151018,0.125849736944674,
-1.69523144286275));
#70338=CARTESIAN_POINT('Ctrl Pts',(0.585151330193947,0.461145281889343,
-1.67938932943451));
#70339=CARTESIAN_POINT('Ctrl Pts',(0.294012678943567,0.684553573401655,
-1.66354721600628));
#70340=CARTESIAN_POINT('Ctrl Pts',(-0.0684619967945975,0.741869264245018,
-1.64770510257804));
#70341=CARTESIAN_POINT('Ctrl Pts',(-0.414325801541176,0.619185901336431,
-1.6318629891498));
#70342=CARTESIAN_POINT('Ctrl Pts',(-0.659662120089326,0.346270035601989,
-1.61602087572157));
#70343=CARTESIAN_POINT('Ctrl Pts',(-0.744945228274433,-0.0106610087561992,
-1.60017876229333));
#70344=CARTESIAN_POINT('Ctrl Pts',(-0.649482964398754,-0.365005382415594,
-1.5843366488651));
#70345=CARTESIAN_POINT('Ctrl Pts',(-0.396437249294967,-0.630788837574024,
-1.56849453543686));
#70346=CARTESIAN_POINT('Ctrl Pts',(-0.0472043308869144,-0.743524580213772,
-1.55265242200863));
#70347=CARTESIAN_POINT('Ctrl Pts',(0.3134817306855,-0.675859641318353,-1.53681030858039));
#70348=CARTESIAN_POINT('Ctrl Pts',(0.59810800974443,-0.444211502458123,
-1.52096819515216));
#70349=CARTESIAN_POINT('Ctrl Pts',(0.737615895328708,-0.104784737414259,
-1.50512608172392));
#70350=CARTESIAN_POINT('Ctrl Pts',(0.698156718129113,0.260065851598656,
-1.48928396829569));
#70351=CARTESIAN_POINT('Ctrl Pts',(0.489304421830971,0.561816903459843,
-1.47344185486745));
#70352=CARTESIAN_POINT('Ctrl Pts',(0.161732646008563,0.727254839414366,
-1.45759974143922));
#70353=CARTESIAN_POINT('Ctrl Pts',(-0.20508017219881,0.716239606003086,
-1.44175762801098));
#70354=CARTESIAN_POINT('Ctrl Pts',(-0.52213457781493,0.531443819125382,
-1.42591551458275));
#70355=CARTESIAN_POINT('Ctrl Pts',(-0.712503953510709,0.217704309714247,
-1.41007340115451));
#70356=CARTESIAN_POINT('Ctrl Pts',(-0.729999153650814,-0.148856595102944,
-1.39423128772627));
#70357=CARTESIAN_POINT('Ctrl Pts',(-0.570375333998946,-0.479300561862948,
-1.37838917429804));
#70358=CARTESIAN_POINT('Ctrl Pts',(-0.272361874350678,-0.693452276394514,
-1.3625470608698));
#70359=CARTESIAN_POINT('Ctrl Pts',(0.091734495082405,-0.739352306176509,
-1.34670494744157));
#70360=CARTESIAN_POINT('Ctrl Pts',(0.433573408778929,-0.60586396941588,
-1.33086283401333));
#70361=CARTESIAN_POINT('Ctrl Pts',(0.67021480712666,-0.325375417855625,
-1.3150207205851));
#70362=CARTESIAN_POINT('Ctrl Pts',(0.744242606411063,0.0340586705409123,
-1.29917860715686));
#70363=CARTESIAN_POINT('Ctrl Pts',(0.63769551012784,0.385229135190137,-1.28333649372863));
#70364=CARTESIAN_POINT('Ctrl Pts',(0.376424941749179,0.64293181089885,-1.26749438030039));
#70365=CARTESIAN_POINT('Ctrl Pts',(0.0238227377454225,0.744640535696828,
-1.25165226687216));
#70366=CARTESIAN_POINT('Ctrl Pts',(-0.334559555094233,0.665677815712449,
-1.23581015344392));
#70367=CARTESIAN_POINT('Ctrl Pts',(-0.611767972369815,0.425202302697283,
-1.21996804001569));
#70368=CARTESIAN_POINT('Ctrl Pts',(-0.740543692067099,0.0815603480631216,
-1.20412592658745));
#70369=CARTESIAN_POINT('Ctrl Pts',(-0.689641980364514,-0.281870518421948,
-1.18828381315922));
#70370=CARTESIAN_POINT('Ctrl Pts',(-0.471413072515636,-0.576911401601594,
-1.17244169973098));
#70371=CARTESIAN_POINT('Ctrl Pts',(-0.138805646686953,-0.731976804744769,
-1.15659958630274));
#70372=CARTESIAN_POINT('Ctrl Pts',(0.227480064876487,-0.709443352439317,
-1.14075747287451));
#70373=CARTESIAN_POINT('Ctrl Pts',(0.538572498596197,-0.514778315386726,
-1.12491535944627));
#70374=CARTESIAN_POINT('Ctrl Pts',(0.718991584872685,-0.195213091566146,
-1.10907324601804));
#70375=CARTESIAN_POINT('Ctrl Pts',(0.724962407593727,0.171716504193551,
-1.0932311325898));
#70376=CARTESIAN_POINT('Ctrl Pts',(0.555036271562332,0.496982683286584,
-1.07738901916157));
#70377=CARTESIAN_POINT('Ctrl Pts',(0.250442198073112,0.701666413376653,
-1.06154690573333));
#70378=CARTESIAN_POINT('Ctrl Pts',(-0.11491643440966,0.736105470254853,
-1.0457047923051));
#70379=CARTESIAN_POINT('Ctrl Pts',(-0.452392998647782,0.591943937388512,
-1.02986267887686));
#70380=CARTESIAN_POINT('Ctrl Pts',(-0.680105867845271,0.304159594224771,
-1.01402056544863));
#70381=CARTESIAN_POINT('Ctrl Pts',(-0.742805279061213,-0.0574227101009686,
-0.998178452020394));
#70382=CARTESIAN_POINT('Ctrl Pts',(-0.625278532115667,-0.40507259536017,
-0.982336338592156));
#70383=CARTESIAN_POINT('Ctrl Pts',(-0.356041032970718,-0.654440091282382,
-0.966494225163925));
#70384=CARTESIAN_POINT('Ctrl Pts',(-0.000417627143387664,-0.745021392863397,
-0.950652111735685));
#70385=CARTESIAN_POINT('Ctrl Pts',(0.355307107171661,-0.654838842639816,
-0.934809998307453));
#70386=CARTESIAN_POINT('Ctrl Pts',(0.624824006542467,-0.405773349401816,
-0.918967884879216));
#70387=CARTESIAN_POINT('Ctrl Pts',(0.742740434833499,-0.0582554435215241,
-0.903125771450982));
#70388=CARTESIAN_POINT('Ctrl Pts',(0.680446438058071,0.303396926765304,
-0.887283658022746));
#70389=CARTESIAN_POINT('Ctrl Pts',(0.453056351065208,0.591436381190763,
-0.871441544594511));
#70390=CARTESIAN_POINT('Ctrl Pts',(0.115741620447917,0.735976173209866,
-0.855599431166276));
#70391=CARTESIAN_POINT('Ctrl Pts',(-0.24965539253963,0.701946746706922,
-0.839757317738039));
#70392=CARTESIAN_POINT('Ctrl Pts',(-0.55447874843284,0.497604629975343,
-0.823915204309805));
#70393=CARTESIAN_POINT('Ctrl Pts',(-0.724769438189725,0.172529161890676,
-0.808073090881569));
#70394=CARTESIAN_POINT('Ctrl Pts',(-0.71920998918227,-0.194406897246436,
-0.792230977453334));
#70395=CARTESIAN_POINT('Ctrl Pts',(-0.539149285383643,-0.514174190626926,
-0.776388864025099));
#70396=CARTESIAN_POINT('Ctrl Pts',(-0.228275288896775,-0.709187875471401,
-0.760546750596862));
#70397=CARTESIAN_POINT('Ctrl Pts',(0.13798492990271,-0.732131961709289,
-0.74470463716863));
#70398=CARTESIAN_POINT('Ctrl Pts',(0.470765992722073,-0.577439546907681,
-0.728862523740392));
#70399=CARTESIAN_POINT('Ctrl Pts',(0.689325537933745,-0.282643508662239,
-0.713020410312158));
#70400=CARTESIAN_POINT('Ctrl Pts',(0.740634665133557,0.0807300627960256,
-0.697178296883922));
#70401=CARTESIAN_POINT('Ctrl Pts',(0.61224428822249,0.424516173750169,-0.681336183455687));
#70402=CARTESIAN_POINT('Ctrl Pts',(0.335305645658125,0.665302317917453,
-0.665494070027452));
#70403=CARTESIAN_POINT('Ctrl Pts',(-0.022987895734092,0.744666775736816,
-0.649651956599217));
#70404=CARTESIAN_POINT('Ctrl Pts',(-0.375703905235841,0.643353422177177,
-0.633809843170981));
#70405=CARTESIAN_POINT('Ctrl Pts',(-0.637263223535151,0.38594382255211,
-0.617967729742746));
#70406=CARTESIAN_POINT('Ctrl Pts',(-0.744203955035377,0.0348930300525936,
-0.602125616314511));
#70407=CARTESIAN_POINT('Ctrl Pts',(-0.670579168915521,-0.324623826071213,
-0.586283502886275));
#70408=CARTESIAN_POINT('Ctrl Pts',(-0.434252378968355,-0.605377503378576,
-0.570441389458041));
#70409=CARTESIAN_POINT('Ctrl Pts',(-0.0925633357629972,-0.739248996691216,
-0.554599276029804));
#70410=CARTESIAN_POINT('Ctrl Pts',(0.271584264026978,-0.693757189346148,
-0.53875716260157));
#70411=CARTESIAN_POINT('Ctrl Pts',(0.569837624906181,-0.479939716503923,
-0.522915049173334));
#70412=CARTESIAN_POINT('Ctrl Pts',(0.729831809648918,-0.149674913933615,
-0.507072935745098));
#70413=CARTESIAN_POINT('Ctrl Pts',(0.712747577120447,0.216905374635287,
-0.491230822316864));
#70414=CARTESIAN_POINT('Ctrl Pts',(0.522730058864535,0.530858112677697,
-0.475388708888629));
#70415=CARTESIAN_POINT('Ctrl Pts',(0.205883029672815,0.716009237600728,
-0.459546595460393));
#70416=CARTESIAN_POINT('Ctrl Pts',(-0.160917208679019,0.727435703129611,
-0.443704482032157));
#70417=CARTESIAN_POINT('Ctrl Pts',(-0.488674253447083,0.562365116497098,
-0.427862368603923));
#70418=CARTESIAN_POINT('Ctrl Pts',(-0.697864715871596,0.260848401534634,
-0.412020255175687));
#70419=CARTESIAN_POINT('Ctrl Pts',(-0.737732907419063,-0.103957719945394,
-0.396178141747452));
#70420=CARTESIAN_POINT('Ctrl Pts',(-0.598605645679325,-0.443540675943605,
-0.380336028319217));
#70421=CARTESIAN_POINT('Ctrl Pts',(-0.314239249455351,-0.675507767768747,
-0.364493914890981));
#70422=CARTESIAN_POINT('Ctrl Pts',(0.0463707252377993,-0.743577034395874,
-0.348651801462746));
#70423=CARTESIAN_POINT('Ctrl Pts',(0.395729813976248,-0.631232892553112,
-0.33280968803451));
#70424=CARTESIAN_POINT('Ctrl Pts',(0.649073343313576,-0.365733297591681,
-0.316967574606276));
#70425=CARTESIAN_POINT('Ctrl Pts',(0.744932808338686,-0.0114961706467306,
-0.30112546117804));
#70426=CARTESIAN_POINT('Ctrl Pts',(0.660049912914123,0.345530261365429,
-0.285283347749805));
#70427=CARTESIAN_POINT('Ctrl Pts',(0.415019720896205,0.61872100586388,-0.269441234321569));
#70428=CARTESIAN_POINT('Ctrl Pts',(0.0692936706342567,0.741792043967289,
-0.253599120893334));
#70429=CARTESIAN_POINT('Ctrl Pts',(-0.293245025070179,0.684882765631844,
-0.237757007465099));
#70430=CARTESIAN_POINT('Ctrl Pts',(-0.584633978526232,0.461801012217599,
-0.221914894036864));
#70431=CARTESIAN_POINT('Ctrl Pts',(-0.734173677083153,0.12667291162916,
-0.206072780608629));
#70432=CARTESIAN_POINT('Ctrl Pts',(-0.705581599416755,-0.23918973119976,
-0.190230667180393));
#70433=CARTESIAN_POINT('Ctrl Pts',(-0.505794705825495,-0.547017969482345,
-0.174388553752158));
#70434=CARTESIAN_POINT('Ctrl Pts',(-0.183287712150819,-0.72212378510834,
-0.158546440323923));
#70435=CARTESIAN_POINT('Ctrl Pts',(0.183690998201556,-0.722021292731707,
-0.142704326895687));
#70436=CARTESIAN_POINT('Ctrl Pts',(0.506099384029242,-0.546735601718665,
-0.126862213467452));
#70437=CARTESIAN_POINT('Ctrl Pts',(0.705716381011111,-0.238795642840187,
-0.111020100039217));
#70438=CARTESIAN_POINT('Ctrl Pts',(0.734100104964976,0.127082465415513,
-0.0951779866109815));
#70439=CARTESIAN_POINT('Ctrl Pts',(0.584381497914616,0.462127882429814,
-0.0793358731827458));
#70440=CARTESIAN_POINT('Ctrl Pts',(0.29285195986455,0.685045268305722,-0.063493759754511));
#70441=CARTESIAN_POINT('Ctrl Pts',(-0.0696865334553906,0.741755360583931,
-0.0476516463262754));
#70442=CARTESIAN_POINT('Ctrl Pts',(-0.415409884379656,0.618485487271467,
-0.03180953289804));
#70443=CARTESIAN_POINT('Ctrl Pts',(-0.578548277620789,0.436270642466983,
-0.0212481239458833));
#70444=CARTESIAN_POINT('Ctrl Pts',(-0.633489757430006,0.33117581686427,
-0.0159674194698048));
#70445=CARTESIAN_POINT('Ctrl Pts',(0.392888236737278,-0.550964357679762,
-2.9089));
#70446=CARTESIAN_POINT('Ctrl Pts',(0.484292245096581,-0.485784897022383,
-2.90361929552392));
#70447=CARTESIAN_POINT('Ctrl Pts',(0.633945837478465,-0.309125594940106,
-2.89305788657177));
#70448=CARTESIAN_POINT('Ctrl Pts',(0.704592787855342,0.0310787463577468,
-2.87721577314353));
#70449=CARTESIAN_POINT('Ctrl Pts',(0.604289094090405,0.363654317141465,
-2.8613736597153));
#70450=CARTESIAN_POINT('Ctrl Pts',(0.357365708044879,0.608039989146884,
-2.84553154628705));
#70451=CARTESIAN_POINT('Ctrl Pts',(0.0237357764082632,0.704875616667608,
-2.82968943285883));
#70452=CARTESIAN_POINT('Ctrl Pts',(-0.315653531008585,0.630699052042456,
-2.81384731943059));
#70453=CARTESIAN_POINT('Ctrl Pts',(-0.578455917520507,0.403490890783857,
-2.79800520600235));
#70454=CARTESIAN_POINT('Ctrl Pts',(-0.700908179616937,0.0783869961536362,
-2.78216309257412));
#70455=CARTESIAN_POINT('Ctrl Pts',(-0.653299687058058,-0.26573733472401,
-2.76632097914588));
#70456=CARTESIAN_POINT('Ctrl Pts',(-0.447181721367947,-0.545385311748889,
-2.75047886571765));
#70457=CARTESIAN_POINT('Ctrl Pts',(-0.132564454783822,-0.692707336942753,
-2.73463675228941));
#70458=CARTESIAN_POINT('Ctrl Pts',(0.214216796165651,-0.67195822661804,
-2.71879463886118));
#70459=CARTESIAN_POINT('Ctrl Pts',(0.509022827335671,-0.488172612202699,
-2.70295252543294));
#70460=CARTESIAN_POINT('Ctrl Pts',(0.680325118730706,-0.185942077621786,
-2.68711041200471));
#70461=CARTESIAN_POINT('Ctrl Pts',(0.686560756397345,0.161403385589515,
-2.67126829857647));
#70462=CARTESIAN_POINT('Ctrl Pts',(0.526216791985425,0.469587707696419,
-2.65542618514823));
#70463=CARTESIAN_POINT('Ctrl Pts',(0.238197334034658,0.663836391711814,
-2.63958407172001));
#70464=CARTESIAN_POINT('Ctrl Pts',(-0.107615722986078,0.697019069108502,
-2.62374195829176));
#70465=CARTESIAN_POINT('Ctrl Pts',(-0.427318076565427,0.561084652399629,
-2.60789984486353));
#70466=CARTESIAN_POINT('Ctrl Pts',(-0.643340640298785,0.28901478606709,
-2.59205773143529));
#70467=CARTESIAN_POINT('Ctrl Pts',(-0.703270059206417,-0.0531784710760548,
-2.57621561800706));
#70468=CARTESIAN_POINT('Ctrl Pts',(-0.592565713804986,-0.382469084713778,
-2.56037350457882));
#70469=CARTESIAN_POINT('Ctrl Pts',(-0.338087697064974,-0.618961578023624,
-2.54453139115059));
#70470=CARTESIAN_POINT('Ctrl Pts',(-0.00157977493823928,-0.705275995805936,
-2.52868927772235));
#70471=CARTESIAN_POINT('Ctrl Pts',(0.335311446522369,-0.62046995075891,
-2.51284716429412));
#70472=CARTESIAN_POINT('Ctrl Pts',(0.590846361696255,-0.385119855146208,
-2.49700505086588));
#70473=CARTESIAN_POINT('Ctrl Pts',(0.703024770348556,-0.0563284851169273,
-2.48116293743765));
#70474=CARTESIAN_POINT('Ctrl Pts',(0.644628928892509,0.286129813186614,
-2.46532082400941));
#70475=CARTESIAN_POINT('Ctrl Pts',(0.429827366355921,0.559164699431498,
-2.44947871058118));
#70476=CARTESIAN_POINT('Ctrl Pts',(0.110737187280514,0.696529971582292,
-2.43363659715294));
#70477=CARTESIAN_POINT('Ctrl Pts',(-0.235221053172144,0.664896820644794,
-2.41779448372471));
#70478=CARTESIAN_POINT('Ctrl Pts',(-0.524107826947175,0.471940368788045,
-2.40195237029647));
#70479=CARTESIAN_POINT('Ctrl Pts',(-0.685830803189103,0.164477461544244,
-2.38611025686824));
#70480=CARTESIAN_POINT('Ctrl Pts',(-0.681151285679508,-0.182892460140387,
-2.37026814344));
#70481=CARTESIAN_POINT('Ctrl Pts',(-0.511204661425697,-0.485887353298784,
-2.35442603001177));
#70482=CARTESIAN_POINT('Ctrl Pts',(-0.217224922760744,-0.6709918471119,
-2.33858391658353));
#70483=CARTESIAN_POINT('Ctrl Pts',(0.129459898096913,-0.693294209368428,
-2.32274180315529));
#70484=CARTESIAN_POINT('Ctrl Pts',(0.4447339835604,-0.54738323853179,-2.30689968972706));
#70485=CARTESIAN_POINT('Ctrl Pts',(0.652102673733417,-0.268661178566577,
-2.29105757629882));
#70486=CARTESIAN_POINT('Ctrl Pts',(0.701252295024287,0.0752458947865185,
-2.27521546287059));
#70487=CARTESIAN_POINT('Ctrl Pts',(0.580257720256285,0.400896126249721,
-2.25937334944235));
#70488=CARTESIAN_POINT('Ctrl Pts',(0.318475751250181,0.629277301215201,
-2.24353123601412));
#70489=CARTESIAN_POINT('Ctrl Pts',(-0.0205776948622204,0.70497750633138,
-2.22768912258588));
#70490=CARTESIAN_POINT('Ctrl Pts',(-0.354638393893549,0.609629670813075,
-2.21184700915765));
#70491=CARTESIAN_POINT('Ctrl Pts',(-0.602653507265104,0.366367951846396,
-2.19600489572941));
#70492=CARTESIAN_POINT('Ctrl Pts',(-0.704447357300714,0.0342147154174032,
-2.18016278230118));
#70493=CARTESIAN_POINT('Ctrl Pts',(-0.635321796271045,-0.306240005783024,
-2.16432066887294));
#70494=CARTESIAN_POINT('Ctrl Pts',(-0.412048695144598,-0.572391997488336,
-2.14847855544471));
#70495=CARTESIAN_POINT('Ctrl Pts',(-0.0888006000396183,-0.699665047999155,
-2.13263644201647));
#70496=CARTESIAN_POINT('Ctrl Pts',(0.255993102559969,-0.657179014729453,
-2.11679432858824));
#70497=CARTESIAN_POINT('Ctrl Pts',(0.538675435341973,-0.455242244654634,
-2.10095221516));
#70498=CARTESIAN_POINT('Ctrl Pts',(0.690659445233286,-0.142850469614568,
-2.08511010173177));
#70499=CARTESIAN_POINT('Ctrl Pts',(0.675069392417806,0.204200982807891,
-2.06926798830353));
#70500=CARTESIAN_POINT('Ctrl Pts',(0.495687876997698,0.501707339548235,
-2.0534258748753));
#70501=CARTESIAN_POINT('Ctrl Pts',(0.196038070227499,0.67748490830463,-2.03758376144706));
#70502=CARTESIAN_POINT('Ctrl Pts',(-0.151176272291756,0.688884940069836,
-2.02174164801882));
#70503=CARTESIAN_POINT('Ctrl Pts',(-0.461710855621964,0.533141455675591,
-2.00589953459059));
#70504=CARTESIAN_POINT('Ctrl Pts',(-0.660220960887921,0.24804235276114,
-1.99005742116235));
#70505=CARTESIAN_POINT('Ctrl Pts',(-0.698542264764505,-0.0972390368973889,
-1.97421530773412));
#70506=CARTESIAN_POINT('Ctrl Pts',(-0.567376904718818,-0.418927408927545,
-1.95837319430588));
#70507=CARTESIAN_POINT('Ctrl Pts',(-0.298549410801028,-0.638971811013141,
-1.94253108087765));
#70508=CARTESIAN_POINT('Ctrl Pts',(0.0427148506610781,-0.703983073299391,
-1.92668896744941));
#70509=CARTESIAN_POINT('Ctrl Pts',(0.373615247395648,-0.598187573318388,
-1.91084685402117));
#70510=CARTESIAN_POINT('Ctrl Pts',(0.613865722048657,-0.347254375426338,
-1.89500474059294));
#70511=CARTESIAN_POINT('Ctrl Pts',(0.705174524058082,-0.0120671694489478,
-1.87916262716471));
#70512=CARTESIAN_POINT('Ctrl Pts',(0.625387483204131,0.326047882696172,
-1.86332051373647));
#70513=CARTESIAN_POINT('Ctrl Pts',(0.393863255448903,0.585054238482422,
-1.84747840030823));
#70514=CARTESIAN_POINT('Ctrl Pts',(0.0667763501367175,0.702109425247569,
-1.83163628688));
#70515=CARTESIAN_POINT('Ctrl Pts',(-0.276512439276773,0.648812451240159,
-1.81579417345177));
#70516=CARTESIAN_POINT('Ctrl Pts',(-0.552711271174482,0.438094711992443,
-1.79995206002353));
#70517=CARTESIAN_POINT('Ctrl Pts',(-0.69480627830909,0.121082457777023,
-1.78410994659529));
#70518=CARTESIAN_POINT('Ctrl Pts',(-0.668321080461322,-0.225307921232401,
-1.76826783316706));
#70519=CARTESIAN_POINT('Ctrl Pts',(-0.479681756700353,-0.517032047602386,
-1.75242571973882));
#70520=CARTESIAN_POINT('Ctrl Pts',(-0.174657691759948,-0.683309166240393,
-1.73658360631059));
#70521=CARTESIAN_POINT('Ctrl Pts',(0.172743407467333,-0.683795613568578,
-1.72074149288235));
#70522=CARTESIAN_POINT('Ctrl Pts',(0.478231933435968,-0.518373363321409,
-1.70489937945412));
#70523=CARTESIAN_POINT('Ctrl Pts',(0.667687487503493,-0.227178663149353,
-1.68905726602588));
#70524=CARTESIAN_POINT('Ctrl Pts',(0.695142643731443,0.119136186044015,
-1.67321515259765));
#70525=CARTESIAN_POINT('Ctrl Pts',(0.553935982945549,0.436545132554703,
-1.65737303916941));
#70526=CARTESIAN_POINT('Ctrl Pts',(0.278328346711741,0.648035537124133,
-1.64153092574118));
#70527=CARTESIAN_POINT('Ctrl Pts',(-0.0648098389800511,0.702293678406998,
-1.62568881231294));
#70528=CARTESIAN_POINT('Ctrl Pts',(-0.392223273354511,0.58615495374357,
-1.60984669888471));
#70529=CARTESIAN_POINT('Ctrl Pts',(-0.624471937511469,0.327797994532801,
-1.59400458545647));
#70530=CARTESIAN_POINT('Ctrl Pts',(-0.705205552772174,-0.0100922890538433,
-1.57816247202824));
#70531=CARTESIAN_POINT('Ctrl Pts',(-0.614835796701285,-0.345533889877317,
-1.5623203586));
#70532=CARTESIAN_POINT('Ctrl Pts',(-0.375288999670649,-0.597138922433682,
-1.54647824517177));
#70533=CARTESIAN_POINT('Ctrl Pts',(-0.0446861795912879,-0.703860690273713,
-1.53063613174353));
#70534=CARTESIAN_POINT('Ctrl Pts',(0.296758806931518,-0.639805389526875,
-1.5147940183153));
#70535=CARTESIAN_POINT('Ctrl Pts',(0.566201478471519,-0.420514698596517,
-1.49895190488706));
#70536=CARTESIAN_POINT('Ctrl Pts',(0.698267208723158,-0.0991949150966095,
-1.48310979145883));
#70537=CARTESIAN_POINT('Ctrl Pts',(0.660913011645563,0.246192438951009,
-1.46726767803059));
#70538=CARTESIAN_POINT('Ctrl Pts',(0.46320210154304,0.53184634913212,-1.45142556460235));
#70539=CARTESIAN_POINT('Ctrl Pts',(0.153104893757042,0.688458871296389,
-1.43558345117412));
#70540=CARTESIAN_POINT('Ctrl Pts',(-0.194140012861185,0.678031253973823,
-1.41974133774588));
#70541=CARTESIAN_POINT('Ctrl Pts',(-0.494280907634458,0.503093540315427,
-1.40389922431765));
#70542=CARTESIAN_POINT('Ctrl Pts',(-0.674494882733548,0.206090706062433,
-1.38805711088941));
#70543=CARTESIAN_POINT('Ctrl Pts',(-0.691056787981589,-0.140915725678943,
-1.37221499746118));
#70544=CARTESIAN_POINT('Ctrl Pts',(-0.539948223619144,-0.453731905170425,
-1.35637288403294));
#70545=CARTESIAN_POINT('Ctrl Pts',(-0.257832520922968,-0.65645953196946,
-1.34053077060471));
#70546=CARTESIAN_POINT('Ctrl Pts',(0.0868408479677307,-0.699910989400294,
-1.32468865717647));
#70547=CARTESIAN_POINT('Ctrl Pts',(0.4104441021973,-0.57354369051582,-1.30884654374824));
#70548=CARTESIAN_POINT('Ctrl Pts',(0.634461683351754,-0.308018016222288,
-1.29300443032));
#70549=CARTESIAN_POINT('Ctrl Pts',(0.70454041281189,0.0322417845955294,
-1.27716231689176));
#70550=CARTESIAN_POINT('Ctrl Pts',(0.603677153234099,0.364678791023317,
-1.26132020346353));
#70551=CARTESIAN_POINT('Ctrl Pts',(0.356344264045233,0.608634119517723,
-1.2454780900353));
#70552=CARTESIAN_POINT('Ctrl Pts',(0.022551895498706,0.7049171142542,-1.22963597660706));
#70553=CARTESIAN_POINT('Ctrl Pts',(-0.316712218604248,0.630166721230049,
-1.21379386317883));
#70554=CARTESIAN_POINT('Ctrl Pts',(-0.579132739896463,0.402519559200629,
-1.19795174975059));
#70555=CARTESIAN_POINT('Ctrl Pts',(-0.701038819895276,0.0772094486374146,
-1.18210963632235));
#70556=CARTESIAN_POINT('Ctrl Pts',(-0.652852499108416,-0.2668339190713,
-1.16626752289412));
#70557=CARTESIAN_POINT('Ctrl Pts',(-0.446265180001859,-0.546135619674237,
-1.15042540946588));
#70558=CARTESIAN_POINT('Ctrl Pts',(-0.13140095282778,-0.692928939758619,
-1.13458329603765));
#70559=CARTESIAN_POINT('Ctrl Pts',(0.215344966055381,-0.671597551777596,
-1.11874118260941));
#70560=CARTESIAN_POINT('Ctrl Pts',(0.509841934903309,-0.487317070676889,
-1.10289906918118));
#70561=CARTESIAN_POINT('Ctrl Pts',(0.680636426416433,-0.184799299225192,
-1.08705695575294));
#70562=CARTESIAN_POINT('Ctrl Pts',(0.686288731012368,0.162556155357116,
-1.07121484232471));
#70563=CARTESIAN_POINT('Ctrl Pts',(0.52542743525236,0.470470760242527,-1.05537272889647));
#70564=CARTESIAN_POINT('Ctrl Pts',(0.237082166616096,0.664235479503821,
-1.03953061546824));
#70565=CARTESIAN_POINT('Ctrl Pts',(-0.108786128932179,0.696837358435242,
-1.02368850204));
#70566=CARTESIAN_POINT('Ctrl Pts',(-0.428259746586556,0.560366233290937,
-1.00784638861177));
#70567=CARTESIAN_POINT('Ctrl Pts',(-0.643825097837578,0.287933967001959,
-0.99200427518353));
#70568=CARTESIAN_POINT('Ctrl Pts',(-0.703179760793738,-0.0543594515159633,
-0.976162161755296));
#70569=CARTESIAN_POINT('Ctrl Pts',(-0.591922568453257,-0.383463686565954,
-0.960320048327059));
#70570=CARTESIAN_POINT('Ctrl Pts',(-0.337047750540382,-0.619528481843024,
-0.944477934898826));
#70571=CARTESIAN_POINT('Ctrl Pts',(-0.000395348502580347,-0.705277654302627,
-0.928635821470588));
#70572=CARTESIAN_POINT('Ctrl Pts',(0.336352976576915,-0.619905961502954,
-0.912793708042355));
#70573=CARTESIAN_POINT('Ctrl Pts',(0.59149228989595,-0.384127058344892,
-0.896951594614118));
#70574=CARTESIAN_POINT('Ctrl Pts',(0.703118375731167,-0.0551477621324492,
-0.881109481185884));
#70575=CARTESIAN_POINT('Ctrl Pts',(0.644147500070733,0.287211984624038,
-0.865267367757648));
#70576=CARTESIAN_POINT('Ctrl Pts',(0.428887711959651,0.559885753068489,
-0.849425254329413));
#70577=CARTESIAN_POINT('Ctrl Pts',(0.109567294787274,0.696714958840452,
-0.833583140901177));
#70578=CARTESIAN_POINT('Ctrl Pts',(-0.236337333828263,0.664500858237221,
-0.817741027472942));
#70579=CARTESIAN_POINT('Ctrl Pts',(-0.524899653622529,0.471059528707363,
-0.801898914044707));
#70580=CARTESIAN_POINT('Ctrl Pts',(-0.686106055709472,0.163325461205062,
-0.786056800616471));
#70581=CARTESIAN_POINT('Ctrl Pts',(-0.680843179780333,-0.184036111960829,
-0.770214687188236));
#70582=CARTESIAN_POINT('Ctrl Pts',(-0.510387952556461,-0.48674517341652,
-0.754372573760001));
#70583=CARTESIAN_POINT('Ctrl Pts',(-0.216097768239373,-0.671355703424805,
-0.738530460331765));
#70584=CARTESIAN_POINT('Ctrl Pts',(0.13062401781091,-0.693075819755666,
-0.722688346903532));
#70585=CARTESIAN_POINT('Ctrl Pts',(0.445652619177005,-0.546635590663221,
-0.706846233475294));
#70586=CARTESIAN_POINT('Ctrl Pts',(0.652552937542223,-0.267565673553371,
-0.69100412004706));
#70587=CARTESIAN_POINT('Ctrl Pts',(0.701124939933614,0.0764234555757611,
-0.675162006618824));
#70588=CARTESIAN_POINT('Ctrl Pts',(0.579583646314047,0.401870032329318,
-0.659319893190589));
#70589=CARTESIAN_POINT('Ctrl Pts',(0.317418508393823,0.629811254653404,
-0.643477779762354));
#70590=CARTESIAN_POINT('Ctrl Pts',(-0.0217615887758392,0.704941954499094,
-0.627635666334118));
#70591=CARTESIAN_POINT('Ctrl Pts',(-0.355661691778637,0.609033239618506,
-0.611793552905885));
#70592=CARTESIAN_POINT('Ctrl Pts',(-0.603267927301802,0.365355352838904,
-0.595951439477647));
#70593=CARTESIAN_POINT('Ctrl Pts',(-0.704503823323535,0.0330316345580622,
-0.580109326049413));
#70594=CARTESIAN_POINT('Ctrl Pts',(-0.634806607981066,-0.307306518679029,
-0.564267212621177));
#70595=CARTESIAN_POINT('Ctrl Pts',(-0.411086852200351,-0.573083175383003,
-0.548425099192943));
#70596=CARTESIAN_POINT('Ctrl Pts',(-0.0876254735054571,-0.699813191038862,
-0.532582985764706));
#70597=CARTESIAN_POINT('Ctrl Pts',(0.257096392819387,-0.656748179105437,
-0.516740872336472));
#70598=CARTESIAN_POINT('Ctrl Pts',(0.539439199031029,-0.454336963616046,
-0.500898758908236));
#70599=CARTESIAN_POINT('Ctrl Pts',(0.690898371074035,-0.141690390662916,
-0.485056645480001));
#70600=CARTESIAN_POINT('Ctrl Pts',(0.67472551005466,0.205334390789043,-0.469214532051766));
#70601=CARTESIAN_POINT('Ctrl Pts',(0.494844622289992,0.502539078828164,
-0.45337241862353));
#70602=CARTESIAN_POINT('Ctrl Pts',(0.194900041286442,0.67781317475087,-0.437530305195295));
#70603=CARTESIAN_POINT('Ctrl Pts',(-0.152332956558304,0.688630086697795,
-0.42168819176706));
#70604=CARTESIAN_POINT('Ctrl Pts',(-0.462605549975718,0.532365317323737,
-0.405846078338825));
#70605=CARTESIAN_POINT('Ctrl Pts',(-0.660636586472805,0.246933243159456,
-0.390003964910589));
#70606=CARTESIAN_POINT('Ctrl Pts',(-0.698377978713657,-0.0984120155099795,
-0.374161851482354));
#70607=CARTESIAN_POINT('Ctrl Pts',(-0.566672567635157,-0.419879657837779,
-0.358319738054119));
#70608=CARTESIAN_POINT('Ctrl Pts',(-0.297475915280626,-0.639472286942102,
-0.342477624625884));
#70609=CARTESIAN_POINT('Ctrl Pts',(0.043897043275945,-0.703910346247173,
-0.326635511197648));
#70610=CARTESIAN_POINT('Ctrl Pts',(0.374619303032495,-0.597559288958764,
-0.310793397769413));
#70611=CARTESIAN_POINT('Ctrl Pts',(0.614448027167589,-0.346222973859112,
-0.294951284341178));
#70612=CARTESIAN_POINT('Ctrl Pts',(0.70519379538744,-0.0108828985917093,
-0.279109170912942));
#70613=CARTESIAN_POINT('Ctrl Pts',(0.624839043230104,0.327097684121224,
-0.263267057484707));
#70614=CARTESIAN_POINT('Ctrl Pts',(0.392880175048439,0.585714858477159,
-0.247424944056472));
#70615=CARTESIAN_POINT('Ctrl Pts',(0.0655971465397984,0.70222057750431,
-0.231582830628236));
#70616=CARTESIAN_POINT('Ctrl Pts',(-0.277601643923981,0.6483471683419,-0.215740717200002));
#70617=CARTESIAN_POINT('Ctrl Pts',(-0.553446229800004,0.437165882444832,
-0.199898603771766));
#70618=CARTESIAN_POINT('Ctrl Pts',(-0.695008618254376,0.119915447842551,
-0.184056490343531));
#70619=CARTESIAN_POINT('Ctrl Pts',(-0.667941806936793,-0.226429971232753,
-0.168214376915295));
#70620=CARTESIAN_POINT('Ctrl Pts',(-0.478812698669308,-0.517836875656849,
-0.15237226348706));
#70621=CARTESIAN_POINT('Ctrl Pts',(-0.173510088336382,-0.683601537024222,
-0.136530150058825));
#70622=CARTESIAN_POINT('Ctrl Pts',(0.173891860782926,-0.683504512182157,
-0.120688036630589));
#70623=CARTESIAN_POINT('Ctrl Pts',(0.479101123580215,-0.517569571018445,
-0.104845923202354));
#70624=CARTESIAN_POINT('Ctrl Pts',(0.668069398503454,-0.226056905819471,
-0.0890038097741189));
#70625=CARTESIAN_POINT('Ctrl Pts',(0.694938970897365,0.12030315366754,-0.0731616963458836));
#70626=CARTESIAN_POINT('Ctrl Pts',(0.553207217960577,0.437475315514465,
-0.057319582917648));
#70627=CARTESIAN_POINT('Ctrl Pts',(0.27722954708371,0.648501002185801,-0.0414774694894131));
#70628=CARTESIAN_POINT('Ctrl Pts',(-0.0659690517919311,0.702185851024218,
-0.0256353560611776));
#70629=CARTESIAN_POINT('Ctrl Pts',(-0.393249524961131,0.58549190380499,
-0.0097932426329422));
#70630=CARTESIAN_POINT('Ctrl Pts',(-0.547685175284667,0.412997449882125,
0.000768166319214589));
#70631=CARTESIAN_POINT('Ctrl Pts',(-0.59969575964498,0.313508988489694,
0.00604887079529304));
#70632=CARTESIAN_POINT('Origin',(0.,0.,-0.0600000000000001));
#70633=CARTESIAN_POINT('',(0.8511,-1.04229689075431E-16,0.));
#70634=CARTESIAN_POINT('Origin',(0.,0.,0.));
#70635=CARTESIAN_POINT('Origin',(0.8511,-1.04229689075431E-16,-0.0600000000000001));
#70636=CARTESIAN_POINT('Origin',(0.,0.,-0.0600000000000001));
#70637=CARTESIAN_POINT('Origin',(0.,0.,0.));
#70638=CARTESIAN_POINT('',(1.2,-0.692820323027552,0.));
#70639=CARTESIAN_POINT('',(1.2,0.692820323027551,0.));
#70640=CARTESIAN_POINT('',(1.2,-0.692820323027552,0.));
#70641=CARTESIAN_POINT('',(-2.54538057293978E-16,-1.3856406460551,0.));
#70642=CARTESIAN_POINT('',(-2.54538057293978E-16,-1.3856406460551,0.));
#70643=CARTESIAN_POINT('',(-1.2,-0.692820323027551,0.));
#70644=CARTESIAN_POINT('',(-1.2,-0.692820323027551,0.));
#70645=CARTESIAN_POINT('',(-1.2,0.692820323027551,0.));
#70646=CARTESIAN_POINT('',(-1.2,0.692820323027551,0.));
#70647=CARTESIAN_POINT('',(8.48460190979926E-17,1.3856406460551,0.));
#70648=CARTESIAN_POINT('',(8.48460190979926E-17,1.3856406460551,0.));
#70649=CARTESIAN_POINT('',(1.2,0.692820323027551,0.));
#70650=CARTESIAN_POINT('Origin',(0.,0.,-1.425));
#70651=CARTESIAN_POINT('Origin',(0.,0.,0.914655896708346));
#70652=CARTESIAN_POINT('',(1.2,-0.692820323027552,0.858179306876173));
#70653=CARTESIAN_POINT('',(-2.54538057293978E-16,-1.3856406460551,0.858179306876173));
#70654=CARTESIAN_POINT('Ctrl Pts',(1.2,-0.692820323027552,0.858179306876173));
#70655=CARTESIAN_POINT('Ctrl Pts',(0.599999999999999,-1.03923048454133,
1.05817930687617));
#70656=CARTESIAN_POINT('Ctrl Pts',(-2.54538057293978E-16,-1.3856406460551,
0.858179306876173));
#70657=CARTESIAN_POINT('',(1.2,0.692820323027551,0.858179306876173));
#70658=CARTESIAN_POINT('Ctrl Pts',(1.2,0.692820323027551,0.858179306876173));
#70659=CARTESIAN_POINT('Ctrl Pts',(1.2,-6.66133814775094E-16,1.05817930687617));
#70660=CARTESIAN_POINT('Ctrl Pts',(1.2,-0.692820323027552,0.858179306876173));
#70661=CARTESIAN_POINT('',(8.48460190979925E-17,1.3856406460551,0.858179306876173));
#70662=CARTESIAN_POINT('Ctrl Pts',(8.48460190979925E-17,1.3856406460551,
0.858179306876173));
#70663=CARTESIAN_POINT('Ctrl Pts',(0.6,1.03923048454133,1.05817930687617));
#70664=CARTESIAN_POINT('Ctrl Pts',(1.2,0.692820323027551,0.858179306876173));
#70665=CARTESIAN_POINT('',(-1.2,0.692820323027551,0.858179306876173));
#70666=CARTESIAN_POINT('Ctrl Pts',(-1.2,0.692820323027551,0.858179306876173));
#70667=CARTESIAN_POINT('Ctrl Pts',(-0.600000000000001,1.03923048454133,
1.05817930687617));
#70668=CARTESIAN_POINT('Ctrl Pts',(8.48460190979925E-17,1.3856406460551,
0.858179306876173));
#70669=CARTESIAN_POINT('',(-1.2,-1.11389921653139E-16,0.965358983848622));
#70670=CARTESIAN_POINT('Ctrl Pts',(-1.2,-7.58222274085957E-17,0.965358983848622));
#70671=CARTESIAN_POINT('Ctrl Pts',(-1.2,0.321539030917347,0.965358983848622));
#70672=CARTESIAN_POINT('Ctrl Pts',(-1.2,0.692820323027551,0.858179306876173));
#70673=CARTESIAN_POINT('',(-1.14,-1.39609735102798E-16,1.));
#70674=CARTESIAN_POINT('',(-1.28782032302755,-1.5771250364726E-16,0.914655896708346));
#70675=CARTESIAN_POINT('Origin',(0.,0.,1.));
#70676=CARTESIAN_POINT('',(-1.2,-0.692820323027551,0.858179306876173));
#70677=CARTESIAN_POINT('Ctrl Pts',(-1.2,-0.692820323027551,0.858179306876173));
#70678=CARTESIAN_POINT('Ctrl Pts',(-1.2,-0.321539030917347,0.965358983848622));
#70679=CARTESIAN_POINT('Ctrl Pts',(-1.2,-7.58222274085957E-17,0.965358983848622));
#70680=CARTESIAN_POINT('Ctrl Pts',(-2.54538057293978E-16,-1.3856406460551,
0.858179306876173));
#70681=CARTESIAN_POINT('Ctrl Pts',(-0.599999999999999,-1.03923048454133,
1.05817930687617));
#70682=CARTESIAN_POINT('Ctrl Pts',(-1.2,-0.692820323027551,0.858179306876173));
#70683=CARTESIAN_POINT('Origin',(8.48460190979926E-17,1.3856406460551,0.));
#70684=CARTESIAN_POINT('',(8.48460190979926E-17,1.3856406460551,0.));
#70685=CARTESIAN_POINT('',(-1.2,0.692820323027551,0.));
#70686=CARTESIAN_POINT('Origin',(1.2,0.692820323027551,0.));
#70687=CARTESIAN_POINT('',(1.2,0.692820323027551,0.));
#70688=CARTESIAN_POINT('Origin',(1.2,-0.692820323027552,0.));
#70689=CARTESIAN_POINT('',(1.2,-0.692820323027552,0.));
#70690=CARTESIAN_POINT('Origin',(-2.54538057293978E-16,-1.3856406460551,
0.));
#70691=CARTESIAN_POINT('',(-2.54538057293978E-16,-1.3856406460551,0.));
#70692=CARTESIAN_POINT('Origin',(-1.2,-0.692820323027551,0.));
#70693=CARTESIAN_POINT('',(-1.2,-0.692820323027551,0.));
#70694=CARTESIAN_POINT('Origin',(-1.2,0.692820323027551,0.));
#70695=CARTESIAN_POINT('Origin',(0.,0.,1.));
#70696=CARTESIAN_POINT('Origin',(0.7,0.,-3.));
#70697=CARTESIAN_POINT('',(-0.7,-8.57252759403147E-17,-3.));
#70698=CARTESIAN_POINT('Origin',(0.,0.,-3.));
#70699=CARTESIAN_POINT('Origin',(0.,0.,-2.95));
#70700=CARTESIAN_POINT('',(-0.75,-9.18485099360515E-17,-2.95));
#70701=CARTESIAN_POINT('',(0.,0.,0.));
#70702=CARTESIAN_POINT('',(9.31,-21.5,78.));
#70703=CARTESIAN_POINT('',(0.,0.,0.));
#70704=CARTESIAN_POINT('',(0.,0.,0.));
#70705=CARTESIAN_POINT('',(0.,0.,0.));
#70706=CARTESIAN_POINT('',(0.,0.,0.));
#70707=CARTESIAN_POINT('',(-11.995,0.,69.));
#70708=CARTESIAN_POINT('',(-10.,0.,69.));
#70709=CARTESIAN_POINT('',(15.8925468086053,-16.3,80.3958511039963));
#70710=CARTESIAN_POINT('',(9.31,-25.505,78.));
#70711=CARTESIAN_POINT('',(0.,0.,14.));
#70712=CARTESIAN_POINT('',(-11.995,0.,74.));
#70713=CARTESIAN_POINT('',(-11.995,0.,82.));
#70714=CARTESIAN_POINT('',(-11.995,0.,87.));
#70715=CARTESIAN_POINT('',(-10.,0.,74.));
#70716=CARTESIAN_POINT('',(-10.,0.,82.));
#70717=CARTESIAN_POINT('',(-10.,0.,87.));
#70718=CARTESIAN_POINT('',(9.31,15.8,85.005));
#70719=CARTESIAN_POINT('',(0.,0.,0.));
#70720=CARTESIAN_POINT('',(0.,0.,0.));
#70721=CARTESIAN_POINT('',(9.31,-21.5,78.));
#70722=CARTESIAN_POINT('',(0.,0.,0.));
#70723=CARTESIAN_POINT('',(0.,-4.5,61.4601776313845));
#70724=UNCERTAINTY_MEASURE_WITH_UNIT(LENGTH_MEASURE(0.001),#70758,
'DISTANCE_ACCURACY_VALUE',
'Maximum model space distance between geometric entities at asserted c
onnectivities');
#70725=UNCERTAINTY_MEASURE_WITH_UNIT(LENGTH_MEASURE(0.001),#70758,
'DISTANCE_ACCURACY_VALUE',
'Maximum model space distance between geometric entities at asserted c
onnectivities');
#70726=UNCERTAINTY_MEASURE_WITH_UNIT(LENGTH_MEASURE(0.001),#70758,
'DISTANCE_ACCURACY_VALUE',
'Maximum model space distance between geometric entities at asserted c
onnectivities');
#70727=UNCERTAINTY_MEASURE_WITH_UNIT(LENGTH_MEASURE(0.001),#70758,
'DISTANCE_ACCURACY_VALUE',
'Maximum model space distance between geometric entities at asserted c
onnectivities');
#70728=UNCERTAINTY_MEASURE_WITH_UNIT(LENGTH_MEASURE(0.001),#70758,
'DISTANCE_ACCURACY_VALUE',
'Maximum model space distance between geometric entities at asserted c
onnectivities');
#70729=UNCERTAINTY_MEASURE_WITH_UNIT(LENGTH_MEASURE(0.001),#70758,
'DISTANCE_ACCURACY_VALUE',
'Maximum model space distance between geometric entities at asserted c
onnectivities');
#70730=UNCERTAINTY_MEASURE_WITH_UNIT(LENGTH_MEASURE(0.001),#70758,
'DISTANCE_ACCURACY_VALUE',
'Maximum model space distance between geometric entities at asserted c
onnectivities');
#70731=UNCERTAINTY_MEASURE_WITH_UNIT(LENGTH_MEASURE(0.001),#70758,
'DISTANCE_ACCURACY_VALUE',
'Maximum model space distance between geometric entities at asserted c
onnectivities');
#70732=UNCERTAINTY_MEASURE_WITH_UNIT(LENGTH_MEASURE(0.001),#70758,
'DISTANCE_ACCURACY_VALUE',
'Maximum model space distance between geometric entities at asserted c
onnectivities');
#70733=UNCERTAINTY_MEASURE_WITH_UNIT(LENGTH_MEASURE(0.001),#70758,
'DISTANCE_ACCURACY_VALUE',
'Maximum model space distance between geometric entities at asserted c
onnectivities');
#70734=UNCERTAINTY_MEASURE_WITH_UNIT(LENGTH_MEASURE(0.001),#70758,
'DISTANCE_ACCURACY_VALUE',
'Maximum model space distance between geometric entities at asserted c
onnectivities');
#70735=UNCERTAINTY_MEASURE_WITH_UNIT(LENGTH_MEASURE(0.001),#70758,
'DISTANCE_ACCURACY_VALUE',
'Maximum model space distance between geometric entities at asserted c
onnectivities');
#70736=UNCERTAINTY_MEASURE_WITH_UNIT(LENGTH_MEASURE(0.001),#70758,
'DISTANCE_ACCURACY_VALUE',
'Maximum model space distance between geometric entities at asserted c
onnectivities');
#70737=UNCERTAINTY_MEASURE_WITH_UNIT(LENGTH_MEASURE(0.001),#70758,
'DISTANCE_ACCURACY_VALUE',
'Maximum model space distance between geometric entities at asserted c
onnectivities');
#70738=UNCERTAINTY_MEASURE_WITH_UNIT(LENGTH_MEASURE(0.001),#70758,
'DISTANCE_ACCURACY_VALUE',
'Maximum model space distance between geometric entities at asserted c
onnectivities');
#70739=UNCERTAINTY_MEASURE_WITH_UNIT(LENGTH_MEASURE(0.001),#70758,
'DISTANCE_ACCURACY_VALUE',
'Maximum model space distance between geometric entities at asserted c
onnectivities');
#70740=UNCERTAINTY_MEASURE_WITH_UNIT(LENGTH_MEASURE(0.001),#70758,
'DISTANCE_ACCURACY_VALUE',
'Maximum model space distance between geometric entities at asserted c
onnectivities');
#70741=(
GEOMETRIC_REPRESENTATION_CONTEXT(3)
GLOBAL_UNCERTAINTY_ASSIGNED_CONTEXT((#70724))
GLOBAL_UNIT_ASSIGNED_CONTEXT((#70758,#70760,#70761))
REPRESENTATION_CONTEXT('','3D')
);
#70742=(
GEOMETRIC_REPRESENTATION_CONTEXT(3)
GLOBAL_UNCERTAINTY_ASSIGNED_CONTEXT((#70725))
GLOBAL_UNIT_ASSIGNED_CONTEXT((#70758,#70760,#70761))
REPRESENTATION_CONTEXT('','3D')
);
#70743=(
GEOMETRIC_REPRESENTATION_CONTEXT(3)
GLOBAL_UNCERTAINTY_ASSIGNED_CONTEXT((#70726))
GLOBAL_UNIT_ASSIGNED_CONTEXT((#70758,#70760,#70761))
REPRESENTATION_CONTEXT('','3D')
);
#70744=(
GEOMETRIC_REPRESENTATION_CONTEXT(3)
GLOBAL_UNCERTAINTY_ASSIGNED_CONTEXT((#70727))
GLOBAL_UNIT_ASSIGNED_CONTEXT((#70758,#70760,#70761))
REPRESENTATION_CONTEXT('','3D')
);
#70745=(
GEOMETRIC_REPRESENTATION_CONTEXT(3)
GLOBAL_UNCERTAINTY_ASSIGNED_CONTEXT((#70728))
GLOBAL_UNIT_ASSIGNED_CONTEXT((#70758,#70760,#70761))
REPRESENTATION_CONTEXT('','3D')
);
#70746=(
GEOMETRIC_REPRESENTATION_CONTEXT(3)
GLOBAL_UNCERTAINTY_ASSIGNED_CONTEXT((#70729))
GLOBAL_UNIT_ASSIGNED_CONTEXT((#70758,#70760,#70761))
REPRESENTATION_CONTEXT('','3D')
);
#70747=(
GEOMETRIC_REPRESENTATION_CONTEXT(3)
GLOBAL_UNCERTAINTY_ASSIGNED_CONTEXT((#70730))
GLOBAL_UNIT_ASSIGNED_CONTEXT((#70758,#70760,#70761))
REPRESENTATION_CONTEXT('','3D')
);
#70748=(
GEOMETRIC_REPRESENTATION_CONTEXT(3)
GLOBAL_UNCERTAINTY_ASSIGNED_CONTEXT((#70731))
GLOBAL_UNIT_ASSIGNED_CONTEXT((#70758,#70760,#70761))
REPRESENTATION_CONTEXT('','3D')
);
#70749=(
GEOMETRIC_REPRESENTATION_CONTEXT(3)
GLOBAL_UNCERTAINTY_ASSIGNED_CONTEXT((#70732))
GLOBAL_UNIT_ASSIGNED_CONTEXT((#70758,#70760,#70761))
REPRESENTATION_CONTEXT('','3D')
);
#70750=(
GEOMETRIC_REPRESENTATION_CONTEXT(3)
GLOBAL_UNCERTAINTY_ASSIGNED_CONTEXT((#70733))
GLOBAL_UNIT_ASSIGNED_CONTEXT((#70758,#70760,#70761))
REPRESENTATION_CONTEXT('','3D')
);
#70751=(
GEOMETRIC_REPRESENTATION_CONTEXT(3)
GLOBAL_UNCERTAINTY_ASSIGNED_CONTEXT((#70734))
GLOBAL_UNIT_ASSIGNED_CONTEXT((#70758,#70760,#70761))
REPRESENTATION_CONTEXT('','3D')
);
#70752=(
GEOMETRIC_REPRESENTATION_CONTEXT(3)
GLOBAL_UNCERTAINTY_ASSIGNED_CONTEXT((#70735))
GLOBAL_UNIT_ASSIGNED_CONTEXT((#70758,#70760,#70761))
REPRESENTATION_CONTEXT('','3D')
);
#70753=(
GEOMETRIC_REPRESENTATION_CONTEXT(3)
GLOBAL_UNCERTAINTY_ASSIGNED_CONTEXT((#70736))
GLOBAL_UNIT_ASSIGNED_CONTEXT((#70758,#70760,#70761))
REPRESENTATION_CONTEXT('','3D')
);
#70754=(
GEOMETRIC_REPRESENTATION_CONTEXT(3)
GLOBAL_UNCERTAINTY_ASSIGNED_CONTEXT((#70737))
GLOBAL_UNIT_ASSIGNED_CONTEXT((#70758,#70760,#70761))
REPRESENTATION_CONTEXT('','3D')
);
#70755=(
GEOMETRIC_REPRESENTATION_CONTEXT(3)
GLOBAL_UNCERTAINTY_ASSIGNED_CONTEXT((#70738))
GLOBAL_UNIT_ASSIGNED_CONTEXT((#70758,#70760,#70761))
REPRESENTATION_CONTEXT('','3D')
);
#70756=(
GEOMETRIC_REPRESENTATION_CONTEXT(3)
GLOBAL_UNCERTAINTY_ASSIGNED_CONTEXT((#70739))
GLOBAL_UNIT_ASSIGNED_CONTEXT((#70758,#70760,#70761))
REPRESENTATION_CONTEXT('','3D')
);
#70757=(
GEOMETRIC_REPRESENTATION_CONTEXT(3)
GLOBAL_UNCERTAINTY_ASSIGNED_CONTEXT((#70740))
GLOBAL_UNIT_ASSIGNED_CONTEXT((#70758,#70760,#70761))
REPRESENTATION_CONTEXT('','3D')
);
#70758=(
LENGTH_UNIT()
NAMED_UNIT(*)
SI_UNIT(.CENTI.,.METRE.)
);
#70759=(
LENGTH_UNIT()
NAMED_UNIT(*)
SI_UNIT($,.METRE.)
);
#70760=(
NAMED_UNIT(*)
PLANE_ANGLE_UNIT()
SI_UNIT($,.RADIAN.)
);
#70761=(
NAMED_UNIT(*)
SI_UNIT($,.STERADIAN.)
SOLID_ANGLE_UNIT()
);
#70762=SHAPE_DEFINITION_REPRESENTATION(#70778,#70817);
#70763=SHAPE_DEFINITION_REPRESENTATION(#70779,#70818);
#70764=SHAPE_DEFINITION_REPRESENTATION(#70780,#70819);
#70765=SHAPE_DEFINITION_REPRESENTATION(#70781,#70820);
#70766=SHAPE_DEFINITION_REPRESENTATION(#70782,#70821);
#70767=SHAPE_DEFINITION_REPRESENTATION(#70783,#70822);
#70768=SHAPE_DEFINITION_REPRESENTATION(#70784,#70823);
#70769=SHAPE_DEFINITION_REPRESENTATION(#70785,#70824);
#70770=SHAPE_DEFINITION_REPRESENTATION(#70786,#70825);
#70771=SHAPE_DEFINITION_REPRESENTATION(#70787,#70826);
#70772=SHAPE_DEFINITION_REPRESENTATION(#70788,#70827);
#70773=SHAPE_DEFINITION_REPRESENTATION(#70789,#70828);
#70774=SHAPE_DEFINITION_REPRESENTATION(#70790,#70829);
#70775=SHAPE_DEFINITION_REPRESENTATION(#70791,#70830);
#70776=SHAPE_DEFINITION_REPRESENTATION(#70792,#70831);
#70777=SHAPE_DEFINITION_REPRESENTATION(#70793,#70832);
#70778=PRODUCT_DEFINITION_SHAPE('',$,#70834);
#70779=PRODUCT_DEFINITION_SHAPE('',$,#70835);
#70780=PRODUCT_DEFINITION_SHAPE('',$,#70836);
#70781=PRODUCT_DEFINITION_SHAPE('',$,#70837);
#70782=PRODUCT_DEFINITION_SHAPE('',$,#70838);
#70783=PRODUCT_DEFINITION_SHAPE('',$,#70839);
#70784=PRODUCT_DEFINITION_SHAPE('',$,#70840);
#70785=PRODUCT_DEFINITION_SHAPE('',$,#70841);
#70786=PRODUCT_DEFINITION_SHAPE('',$,#70842);
#70787=PRODUCT_DEFINITION_SHAPE('',$,#70843);
#70788=PRODUCT_DEFINITION_SHAPE('',$,#70844);
#70789=PRODUCT_DEFINITION_SHAPE('',$,#70845);
#70790=PRODUCT_DEFINITION_SHAPE('',$,#70846);
#70791=PRODUCT_DEFINITION_SHAPE('',$,#70847);
#70792=PRODUCT_DEFINITION_SHAPE('',$,#70848);
#70793=PRODUCT_DEFINITION_SHAPE('',$,#70849);
#70794=PRODUCT_DEFINITION_SHAPE($,$,#80);
#70795=PRODUCT_DEFINITION_SHAPE($,$,#81);
#70796=PRODUCT_DEFINITION_SHAPE($,$,#82);
#70797=PRODUCT_DEFINITION_SHAPE($,$,#83);
#70798=PRODUCT_DEFINITION_SHAPE($,$,#84);
#70799=PRODUCT_DEFINITION_SHAPE($,$,#85);
#70800=PRODUCT_DEFINITION_SHAPE($,$,#86);
#70801=PRODUCT_DEFINITION_SHAPE($,$,#87);
#70802=PRODUCT_DEFINITION_SHAPE($,$,#88);
#70803=PRODUCT_DEFINITION_SHAPE($,$,#89);
#70804=PRODUCT_DEFINITION_SHAPE($,$,#90);
#70805=PRODUCT_DEFINITION_SHAPE($,$,#91);
#70806=PRODUCT_DEFINITION_SHAPE($,$,#92);
#70807=PRODUCT_DEFINITION_SHAPE($,$,#93);
#70808=PRODUCT_DEFINITION_SHAPE($,$,#94);
#70809=PRODUCT_DEFINITION_SHAPE($,$,#95);
#70810=PRODUCT_DEFINITION_SHAPE($,$,#96);
#70811=PRODUCT_DEFINITION_SHAPE($,$,#97);
#70812=PRODUCT_DEFINITION_SHAPE($,$,#98);
#70813=PRODUCT_DEFINITION_SHAPE($,$,#99);
#70814=PRODUCT_DEFINITION_SHAPE($,$,#100);
#70815=PRODUCT_DEFINITION_SHAPE($,$,#101);
#70816=PRODUCT_DEFINITION_SHAPE($,$,#102);
#70817=SHAPE_REPRESENTATION('',(#27053,#28962,#28963,#28964,#28965,#28966,
#28967,#28968,#28969,#28970,#28971,#28972,#28973,#28974,#28975,#28976,#28977,
#28978,#28979,#28980,#28981,#28982,#28983,#28984),#70741);
#70818=SHAPE_REPRESENTATION('',(#27054),#70742);
#70819=SHAPE_REPRESENTATION('',(#27231),#70743);
#70820=SHAPE_REPRESENTATION('',(#27283),#70744);
#70821=SHAPE_REPRESENTATION('',(#27389),#70745);
#70822=SHAPE_REPRESENTATION('',(#27399),#70746);
#70823=SHAPE_REPRESENTATION('',(#27432),#70747);
#70824=SHAPE_REPRESENTATION('',(#27510),#70748);
#70825=SHAPE_REPRESENTATION('',(#27547),#70749);
#70826=SHAPE_REPRESENTATION('',(#27669),#70750);
#70827=SHAPE_REPRESENTATION('',(#27689),#70751);
#70828=SHAPE_REPRESENTATION('',(#27791),#70752);
#70829=SHAPE_REPRESENTATION('',(#27818),#70753);
#70830=SHAPE_REPRESENTATION('',(#28305),#70754);
#70831=SHAPE_REPRESENTATION('',(#28396),#70755);
#70832=SHAPE_REPRESENTATION('',(#28892),#70756);
#70833=PRODUCT_DEFINITION_CONTEXT('part definition',#70883,'design');
#70834=PRODUCT_DEFINITION('2026-10-19-02-53-34-095','MAS-305',#70850,#70833);
#70835=PRODUCT_DEFINITION('2026-10-19-02-54-55-610',
'03_Pinion_Shaft_m6_z18_D125_Journals',#70851,#70833);
#70836=PRODUCT_DEFINITION('2026-10-19-02-55-26-880',
'05_Operating_Lever_D40x790_M24_End',#70852,#70833);
#70837=PRODUCT_DEFINITION('2026-10-19-02-55-33-757',
'08_Rotary_Anvil_Plate_D315x45_4-Slot',#70853,#70833);
#70838=PRODUCT_DEFINITION('2026-10-19-02-55-36-383',
'09_Anvil_Centre_Pivot_Pin_D40x98',#70854,#70833);
#70839=PRODUCT_DEFINITION('2026-10-19-02-55-51-279',
'07_Quick-Return_Handwheel_D456_6-Spoke',#70855,#70833);
#70840=PRODUCT_DEFINITION('2026-10-19-02-56-05-716',
'15_ISO_4026_M20x20_Lever_Lock_Screw',#70856,#70833);
#70841=PRODUCT_DEFINITION('2026-10-19-02-55-37-006',
'10_Ram_Guide_Gib_Wear_Plate_110x80x14.9',#70857,#70833);
#70842=PRODUCT_DEFINITION('2026-10-19-02-55-56-496',
'11_ISO_4026_M16x60_Gib_Adjust_Set_Screw',#70858,#70833);
#70843=PRODUCT_DEFINITION('2026-10-19-02-55-58-451',
'12_ISO_4035_M16_Gib_Jam_Nut',#70859,#70833);
#70844=PRODUCT_DEFINITION('2026-10-19-02-56-03-690',
'14_ISO_4026_M16x40_Hub_Set_Screw',#70860,#70833);
#70845=PRODUCT_DEFINITION('2026-10-19-02-58-13-081','04_D150_Lever_Hub',
#70861,#70833);
#70846=PRODUCT_DEFINITION('2026-10-19-02-58-48-360',
'02_Rack_Ram_90x90x855_m6_Rack',#70862,#70833);
#70847=PRODUCT_DEFINITION('2026-10-19-02-59-02-453',
'06_Ergonomic_Ball_Knob_D90_M24',#70863,#70833);
#70848=PRODUCT_DEFINITION('2026-10-19-03-02-56-883',
'01_Cast_Iron_C-Frame_NO.1_840x380_Base',#70864,#70833);
#70849=PRODUCT_DEFINITION('2026-10-19-03-03-09-768',
'13_ISO_4017_M16x30_Ram_Depth_Stop_Screw',#70865,#70833);
#70850=PRODUCT_DEFINITION_FORMATION('',$,#70885);
#70851=PRODUCT_DEFINITION_FORMATION('',$,#70886);
#70852=PRODUCT_DEFINITION_FORMATION('',$,#70887);
#70853=PRODUCT_DEFINITION_FORMATION('',$,#70888);
#70854=PRODUCT_DEFINITION_FORMATION('',$,#70889);
#70855=PRODUCT_DEFINITION_FORMATION('',$,#70890);
#70856=PRODUCT_DEFINITION_FORMATION('',$,#70891);
#70857=PRODUCT_DEFINITION_FORMATION('',$,#70892);
#70858=PRODUCT_DEFINITION_FORMATION('',$,#70893);
#70859=PRODUCT_DEFINITION_FORMATION('',$,#70894);
#70860=PRODUCT_DEFINITION_FORMATION('',$,#70895);
#70861=PRODUCT_DEFINITION_FORMATION('',$,#70896);
#70862=PRODUCT_DEFINITION_FORMATION('',$,#70897);
#70863=PRODUCT_DEFINITION_FORMATION('',$,#70898);
#70864=PRODUCT_DEFINITION_FORMATION('',$,#70899);
#70865=PRODUCT_DEFINITION_FORMATION('',$,#70900);
#70866=PRODUCT_RELATED_PRODUCT_CATEGORY('MAS-305','MAS-305',(#70885));
#70867=PRODUCT_RELATED_PRODUCT_CATEGORY(
'03_Pinion_Shaft_m6_z18_D125_Journals',
'03_Pinion_Shaft_m6_z18_D125_Journals',(#70886));
#70868=PRODUCT_RELATED_PRODUCT_CATEGORY(
'05_Operating_Lever_D40x790_M24_End',
'05_Operating_Lever_D40x790_M24_End',(#70887));
#70869=PRODUCT_RELATED_PRODUCT_CATEGORY(
'08_Rotary_Anvil_Plate_D315x45_4-Slot',
'08_Rotary_Anvil_Plate_D315x45_4-Slot',(#70888));
#70870=PRODUCT_RELATED_PRODUCT_CATEGORY(
'09_Anvil_Centre_Pivot_Pin_D40x98','09_Anvil_Centre_Pivot_Pin_D40x98',(#70889));
#70871=PRODUCT_RELATED_PRODUCT_CATEGORY(
'07_Quick-Return_Handwheel_D456_6-Spoke',
'07_Quick-Return_Handwheel_D456_6-Spoke',(#70890));
#70872=PRODUCT_RELATED_PRODUCT_CATEGORY(
'15_ISO_4026_M20x20_Lever_Lock_Screw',
'15_ISO_4026_M20x20_Lever_Lock_Screw',(#70891));
#70873=PRODUCT_RELATED_PRODUCT_CATEGORY(
'10_Ram_Guide_Gib_Wear_Plate_110x80x14.9',
'10_Ram_Guide_Gib_Wear_Plate_110x80x14.9',(#70892));
#70874=PRODUCT_RELATED_PRODUCT_CATEGORY(
'11_ISO_4026_M16x60_Gib_Adjust_Set_Screw',
'11_ISO_4026_M16x60_Gib_Adjust_Set_Screw',(#70893));
#70875=PRODUCT_RELATED_PRODUCT_CATEGORY('12_ISO_4035_M16_Gib_Jam_Nut',
'12_ISO_4035_M16_Gib_Jam_Nut',(#70894));
#70876=PRODUCT_RELATED_PRODUCT_CATEGORY(
'14_ISO_4026_M16x40_Hub_Set_Screw','14_ISO_4026_M16x40_Hub_Set_Screw',(#70895));
#70877=PRODUCT_RELATED_PRODUCT_CATEGORY('04_D150_Lever_Hub',
'04_D150_Lever_Hub',(#70896));
#70878=PRODUCT_RELATED_PRODUCT_CATEGORY('02_Rack_Ram_90x90x855_m6_Rack',
'02_Rack_Ram_90x90x855_m6_Rack',(#70897));
#70879=PRODUCT_RELATED_PRODUCT_CATEGORY(
'06_Ergonomic_Ball_Knob_D90_M24','06_Ergonomic_Ball_Knob_D90_M24',(#70898));
#70880=PRODUCT_RELATED_PRODUCT_CATEGORY(
'01_Cast_Iron_C-Frame_NO.1_840x380_Base',
'01_Cast_Iron_C-Frame_NO.1_840x380_Base',(#70899));
#70881=PRODUCT_RELATED_PRODUCT_CATEGORY(
'13_ISO_4017_M16x30_Ram_Depth_Stop_Screw',
'13_ISO_4017_M16x30_Ram_Depth_Stop_Screw',(#70900));
#70882=APPLICATION_PROTOCOL_DEFINITION('international standard',
'automotive_design',2009,#70883);
#70883=APPLICATION_CONTEXT(
'Core Data for Automotive Mechanical Design Process');
#70884=PRODUCT_CONTEXT('part definition',#70883,'mechanical');
#70885=PRODUCT('2026-10-19-02-53-34-095','MAS-305',$,(#70884));
#70886=PRODUCT('2026-10-19-02-54-55-610',
'03_Pinion_Shaft_m6_z18_D125_Journals',$,(#70884));
#70887=PRODUCT('2026-10-19-02-55-26-880',
'05_Operating_Lever_D40x790_M24_End',$,(#70884));
#70888=PRODUCT('2026-10-19-02-55-33-757',
'08_Rotary_Anvil_Plate_D315x45_4-Slot',$,(#70884));
#70889=PRODUCT('2026-10-19-02-55-36-383',
'09_Anvil_Centre_Pivot_Pin_D40x98',$,(#70884));
#70890=PRODUCT('2026-10-19-02-55-51-279',
'07_Quick-Return_Handwheel_D456_6-Spoke',$,(#70884));
#70891=PRODUCT('2026-10-19-02-56-05-716',
'15_ISO_4026_M20x20_Lever_Lock_Screw',$,(#70884));
#70892=PRODUCT('2026-10-19-02-55-37-006',
'10_Ram_Guide_Gib_Wear_Plate_110x80x14.9',$,(#70884));
#70893=PRODUCT('2026-10-19-02-55-56-496',
'11_ISO_4026_M16x60_Gib_Adjust_Set_Screw',$,(#70884));
#70894=PRODUCT('2026-10-19-02-55-58-451','12_ISO_4035_M16_Gib_Jam_Nut',
$,(#70884));
#70895=PRODUCT('2026-10-19-02-56-03-690',
'14_ISO_4026_M16x40_Hub_Set_Screw',$,(#70884));
#70896=PRODUCT('2026-10-19-02-58-13-081','04_D150_Lever_Hub',$,(#70884));
#70897=PRODUCT('2026-10-19-02-58-48-360',
'02_Rack_Ram_90x90x855_m6_Rack',$,(#70884));
#70898=PRODUCT('2026-10-19-02-59-02-453',
'06_Ergonomic_Ball_Knob_D90_M24',$,(#70884));
#70899=PRODUCT('2026-10-19-03-02-56-883',
'01_Cast_Iron_C-Frame_NO.1_840x380_Base',$,(#70884));
#70900=PRODUCT('2026-10-19-03-03-09-768',
'13_ISO_4017_M16x30_Ram_Depth_Stop_Screw',$,(#70884));
#70901=PRESENTATION_STYLE_ASSIGNMENT((#70918));
#70902=PRESENTATION_STYLE_ASSIGNMENT((#70919));
#70903=PRESENTATION_STYLE_ASSIGNMENT((#70920));
#70904=PRESENTATION_STYLE_ASSIGNMENT((#70921));
#70905=PRESENTATION_STYLE_ASSIGNMENT((#70922));
#70906=PRESENTATION_STYLE_ASSIGNMENT((#70923));
#70907=PRESENTATION_STYLE_ASSIGNMENT((#70924));
#70908=PRESENTATION_STYLE_ASSIGNMENT((#70925));
#70909=PRESENTATION_STYLE_ASSIGNMENT((#70926));
#70910=PRESENTATION_STYLE_ASSIGNMENT((#70927));
#70911=PRESENTATION_STYLE_ASSIGNMENT((#70928));
#70912=PRESENTATION_STYLE_ASSIGNMENT((#70929));
#70913=PRESENTATION_STYLE_ASSIGNMENT((#70930));
#70914=PRESENTATION_STYLE_ASSIGNMENT((#70931));
#70915=PRESENTATION_STYLE_ASSIGNMENT((#70932));
#70916=PRESENTATION_STYLE_ASSIGNMENT((#70933));
#70917=PRESENTATION_STYLE_ASSIGNMENT((#70934));
#70918=SURFACE_STYLE_USAGE(.BOTH.,#70935);
#70919=SURFACE_STYLE_USAGE(.BOTH.,#70936);
#70920=SURFACE_STYLE_USAGE(.BOTH.,#70937);
#70921=SURFACE_STYLE_USAGE(.BOTH.,#70938);
#70922=SURFACE_STYLE_USAGE(.BOTH.,#70939);
#70923=SURFACE_STYLE_USAGE(.BOTH.,#70940);
#70924=SURFACE_STYLE_USAGE(.BOTH.,#70941);
#70925=SURFACE_STYLE_USAGE(.BOTH.,#70942);
#70926=SURFACE_STYLE_USAGE(.BOTH.,#70943);
#70927=SURFACE_STYLE_USAGE(.BOTH.,#70944);
#70928=SURFACE_STYLE_USAGE(.BOTH.,#70945);
#70929=SURFACE_STYLE_USAGE(.BOTH.,#70946);
#70930=SURFACE_STYLE_USAGE(.BOTH.,#70947);
#70931=SURFACE_STYLE_USAGE(.BOTH.,#70948);
#70932=SURFACE_STYLE_USAGE(.BOTH.,#70949);
#70933=SURFACE_STYLE_USAGE(.BOTH.,#70950);
#70934=SURFACE_STYLE_USAGE(.BOTH.,#70951);
#70935=SURFACE_SIDE_STYLE('',(#70952));
#70936=SURFACE_SIDE_STYLE('',(#70953));
#70937=SURFACE_SIDE_STYLE('',(#70954));
#70938=SURFACE_SIDE_STYLE('',(#70955));
#70939=SURFACE_SIDE_STYLE('',(#70956));
#70940=SURFACE_SIDE_STYLE('',(#70957));
#70941=SURFACE_SIDE_STYLE('',(#70958));
#70942=SURFACE_SIDE_STYLE('',(#70959));
#70943=SURFACE_SIDE_STYLE('',(#70960));
#70944=SURFACE_SIDE_STYLE('',(#70961));
#70945=SURFACE_SIDE_STYLE('',(#70962));
#70946=SURFACE_SIDE_STYLE('',(#70963));
#70947=SURFACE_SIDE_STYLE('',(#70964));
#70948=SURFACE_SIDE_STYLE('',(#70965));
#70949=SURFACE_SIDE_STYLE('',(#70966));
#70950=SURFACE_SIDE_STYLE('',(#70967));
#70951=SURFACE_SIDE_STYLE('',(#70968));
#70952=SURFACE_STYLE_FILL_AREA(#70969);
#70953=SURFACE_STYLE_FILL_AREA(#70970);
#70954=SURFACE_STYLE_FILL_AREA(#70971);
#70955=SURFACE_STYLE_FILL_AREA(#70972);
#70956=SURFACE_STYLE_FILL_AREA(#70973);
#70957=SURFACE_STYLE_FILL_AREA(#70974);
#70958=SURFACE_STYLE_FILL_AREA(#70975);
#70959=SURFACE_STYLE_FILL_AREA(#70976);
#70960=SURFACE_STYLE_FILL_AREA(#70977);
#70961=SURFACE_STYLE_FILL_AREA(#70978);
#70962=SURFACE_STYLE_FILL_AREA(#70979);
#70963=SURFACE_STYLE_FILL_AREA(#70980);
#70964=SURFACE_STYLE_FILL_AREA(#70981);
#70965=SURFACE_STYLE_FILL_AREA(#70982);
#70966=SURFACE_STYLE_FILL_AREA(#70983);
#70967=SURFACE_STYLE_FILL_AREA(#70984);
#70968=SURFACE_STYLE_FILL_AREA(#70985);
#70969=FILL_AREA_STYLE('Steel - Satin',(#70986));
#70970=FILL_AREA_STYLE('MAS305_pin',(#70987));
#70971=FILL_AREA_STYLE('MAS305_lev',(#70988));
#70972=FILL_AREA_STYLE('MAS305_anv',(#70989));
#70973=FILL_AREA_STYLE('MAS305_apin',(#70990));
#70974=FILL_AREA_STYLE('MAS305_hw',(#70991));
#70975=FILL_AREA_STYLE('MAS305_lock',(#70992));
#70976=FILL_AREA_STYLE('MAS305_gib',(#70993));
#70977=FILL_AREA_STYLE('MAS305_gscr',(#70994));
#70978=FILL_AREA_STYLE('MAS305_gnut',(#70995));
#70979=FILL_AREA_STYLE('MAS305_hset',(#70996));
#70980=FILL_AREA_STYLE('MAS305_hub',(#70997));
#70981=FILL_AREA_STYLE('MAS305_ram',(#70998));
#70982=FILL_AREA_STYLE('MAS305_knob',(#70999));
#70983=FILL_AREA_STYLE('MAS305_frame',(#71000));
#70984=FILL_AREA_STYLE('MAS305_NO1_red',(#71001));
#70985=FILL_AREA_STYLE('MAS305_stop',(#71002));
#70986=FILL_AREA_STYLE_COLOUR('Steel - Satin',#71003);
#70987=FILL_AREA_STYLE_COLOUR('MAS305_pin',#71004);
#70988=FILL_AREA_STYLE_COLOUR('MAS305_lev',#71005);
#70989=FILL_AREA_STYLE_COLOUR('MAS305_anv',#71006);
#70990=FILL_AREA_STYLE_COLOUR('MAS305_apin',#71007);
#70991=FILL_AREA_STYLE_COLOUR('MAS305_hw',#71008);
#70992=FILL_AREA_STYLE_COLOUR('MAS305_lock',#71009);
#70993=FILL_AREA_STYLE_COLOUR('MAS305_gib',#71010);
#70994=FILL_AREA_STYLE_COLOUR('MAS305_gscr',#71011);
#70995=FILL_AREA_STYLE_COLOUR('MAS305_gnut',#71012);
#70996=FILL_AREA_STYLE_COLOUR('MAS305_hset',#71013);
#70997=FILL_AREA_STYLE_COLOUR('MAS305_hub',#71014);
#70998=FILL_AREA_STYLE_COLOUR('MAS305_ram',#71015);
#70999=FILL_AREA_STYLE_COLOUR('MAS305_knob',#71016);
#71000=FILL_AREA_STYLE_COLOUR('MAS305_frame',#71017);
#71001=FILL_AREA_STYLE_COLOUR('MAS305_NO1_red',#71018);
#71002=FILL_AREA_STYLE_COLOUR('MAS305_stop',#71019);
#71003=COLOUR_RGB('Steel - Satin',0.627450980392157,0.627450980392157,0.627450980392157);
#71004=COLOUR_RGB('MAS305_pin',0.243137254901961,0.250980392156863,0.266666666666667);
#71005=COLOUR_RGB('MAS305_lev',0.831372549019608,0.843137254901961,0.862745098039216);
#71006=COLOUR_RGB('MAS305_anv',0.133333333333333,0.133333333333333,0.141176470588235);
#71007=COLOUR_RGB('MAS305_apin',0.83921568627451,0.850980392156863,0.870588235294118);
#71008=COLOUR_RGB('MAS305_hw',0.807843137254902,0.819607843137255,0.843137254901961);
#71009=COLOUR_RGB('MAS305_lock',0.780392156862745,0.796078431372549,0.815686274509804);
#71010=COLOUR_RGB('MAS305_gib',0.180392156862745,0.180392156862745,0.188235294117647);
#71011=COLOUR_RGB('MAS305_gscr',0.776470588235294,0.792156862745098,0.815686274509804);
#71012=COLOUR_RGB('MAS305_gnut',0.792156862745098,0.807843137254902,0.827450980392157);
#71013=COLOUR_RGB('MAS305_hset',0.788235294117647,0.803921568627451,0.823529411764706);
#71014=COLOUR_RGB('MAS305_hub',0.117647058823529,0.117647058823529,0.125490196078431);
#71015=COLOUR_RGB('MAS305_ram',0.156862745098039,0.156862745098039,0.164705882352941);
#71016=COLOUR_RGB('MAS305_knob',0.0862745098039216,0.0862745098039216,0.0862745098039216);
#71017=COLOUR_RGB('MAS305_frame',0.101960784313725,0.101960784313725,0.109803921568627);
#71018=COLOUR_RGB('MAS305_NO1_red',0.768627450980392,0.125490196078431,
0.109803921568627);
#71019=COLOUR_RGB('MAS305_stop',0.768627450980392,0.784313725490196,0.807843137254902);
#71020=COLOUR_RGB('Dark Blue',0.08,0.2,0.34);
#71021=FILL_AREA_STYLE_COLOUR('',#71020);
#71022=FILL_AREA_STYLE('',(#71021));
#71023=SURFACE_STYLE_FILL_AREA(#71022);
#71024=SURFACE_SIDE_STYLE('',(#71023));
#71025=SURFACE_STYLE_USAGE(.BOTH.,#71024);
#71026=PRESENTATION_STYLE_ASSIGNMENT((#71025));
#71027=COLOUR_RGB('Light Blue',0.38,0.62,0.78);
#71028=FILL_AREA_STYLE_COLOUR('',#71027);
#71029=FILL_AREA_STYLE('',(#71028));
#71030=SURFACE_STYLE_FILL_AREA(#71029);
#71031=SURFACE_SIDE_STYLE('',(#71030));
#71032=SURFACE_STYLE_USAGE(.BOTH.,#71031);
#71033=PRESENTATION_STYLE_ASSIGNMENT((#71032));
#71034=COLOUR_RGB('Sky Blue',0.24,0.69,0.87);
#71035=FILL_AREA_STYLE_COLOUR('',#71034);
#71036=FILL_AREA_STYLE('',(#71035));
#71037=SURFACE_STYLE_FILL_AREA(#71036);
#71038=SURFACE_SIDE_STYLE('',(#71037));
#71039=SURFACE_STYLE_USAGE(.BOTH.,#71038);
#71040=PRESENTATION_STYLE_ASSIGNMENT((#71039));
#71041=COLOUR_RGB('Grey',0.48,0.52,0.57);
#71042=FILL_AREA_STYLE_COLOUR('',#71041);
#71043=FILL_AREA_STYLE('',(#71042));
#71044=SURFACE_STYLE_FILL_AREA(#71043);
#71045=SURFACE_SIDE_STYLE('',(#71044));
#71046=SURFACE_STYLE_USAGE(.BOTH.,#71045);
#71047=PRESENTATION_STYLE_ASSIGNMENT((#71046));
#71048=COLOUR_RGB('Black',0.12,0.14,0.17);
#71049=FILL_AREA_STYLE_COLOUR('',#71048);
#71050=FILL_AREA_STYLE('',(#71049));
#71051=SURFACE_STYLE_FILL_AREA(#71050);
#71052=SURFACE_SIDE_STYLE('',(#71051));
#71053=SURFACE_STYLE_USAGE(.BOTH.,#71052);
#71054=PRESENTATION_STYLE_ASSIGNMENT((#71053));
#71055=COLOUR_RGB('Off White',0.89,0.88,0.83);
#71056=FILL_AREA_STYLE_COLOUR('',#71055);
#71057=FILL_AREA_STYLE('',(#71056));
#71058=SURFACE_STYLE_FILL_AREA(#71057);
#71059=SURFACE_SIDE_STYLE('',(#71058));
#71060=SURFACE_STYLE_USAGE(.BOTH.,#71059);
#71061=PRESENTATION_STYLE_ASSIGNMENT((#71060));
ENDSEC;
END-ISO-10303-21;
